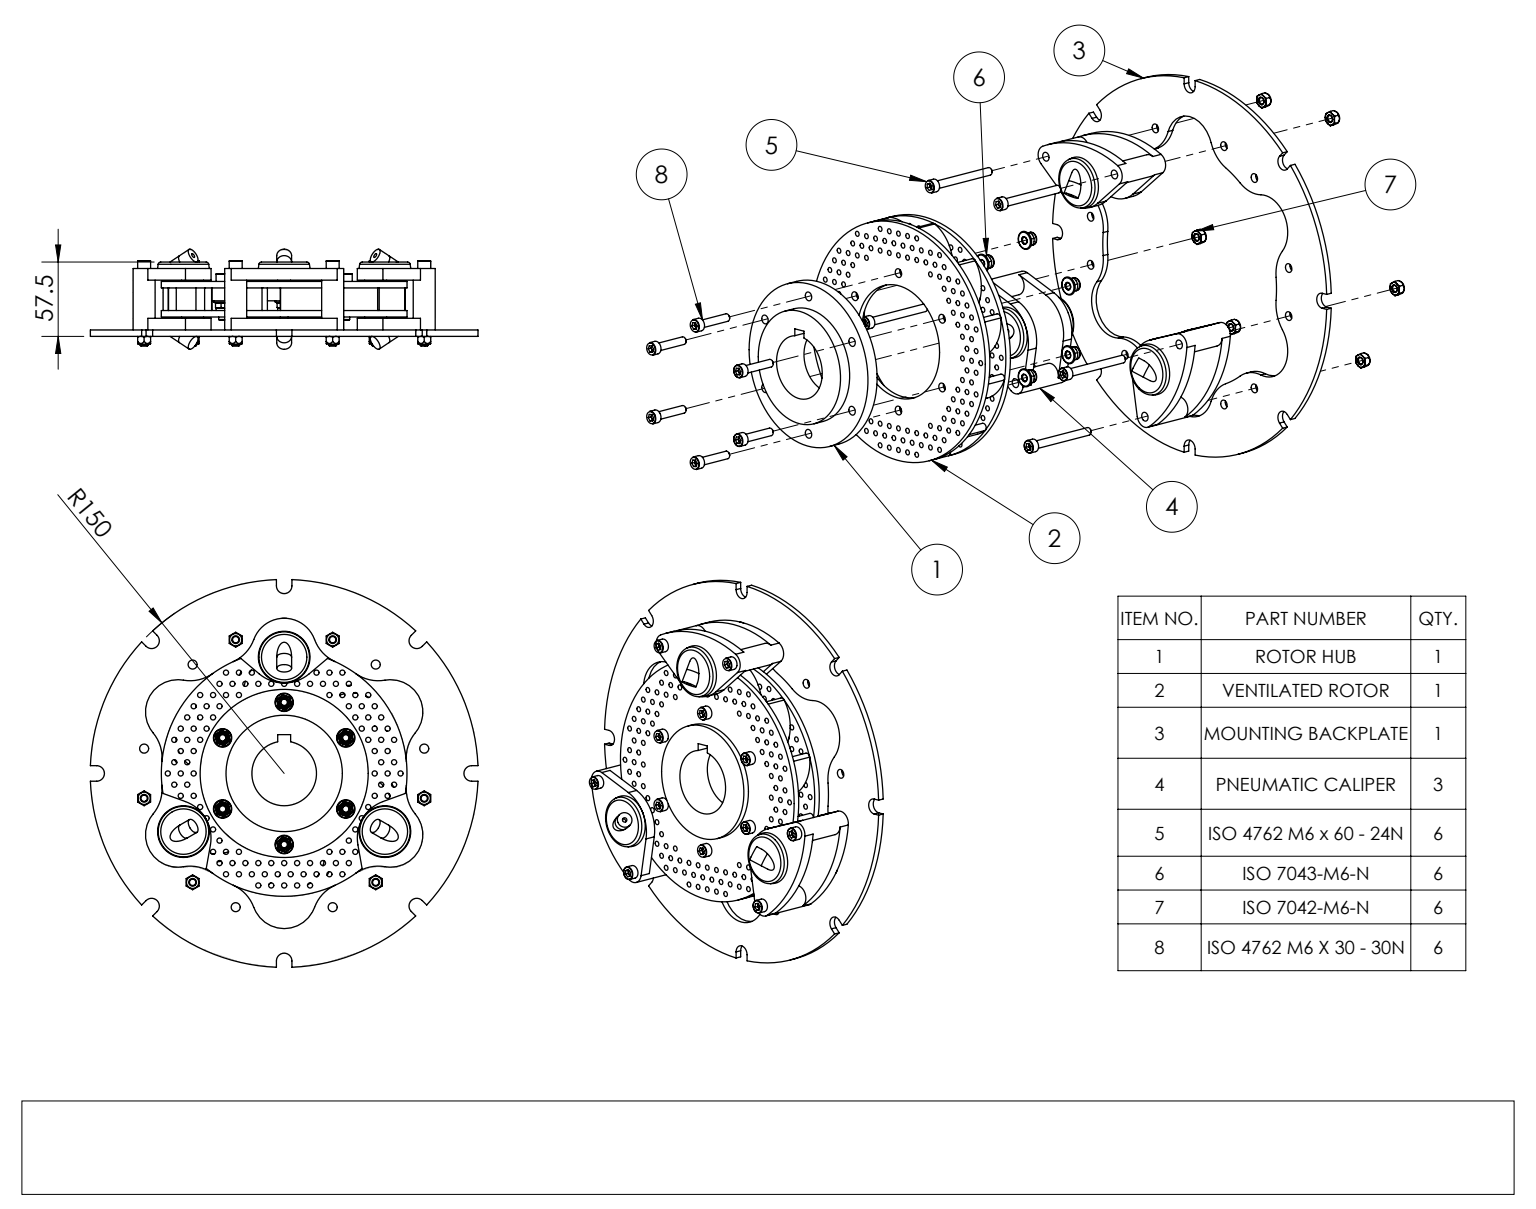
ISO-10303-21;
HEADER;
FILE_DESCRIPTION (('STEP AP214'),
    '1' );
FILE_NAME ('BR-596',
    '2026-09-21T15:58:29',
    ( '' ),
    ( '' ),
    'SwSTEP 2.0',
    'SolidWorks 2026',
    '' );
FILE_SCHEMA (( 'AUTOMOTIVE_DESIGN' ));
ENDSEC;

DATA;
#1 = ORIENTED_EDGE ( 'NONE', *, *, #25263, .F. ) ;
#2 = EDGE_CURVE ( 'NONE', #26836, #23671, #14788, .T. ) ;
#3 = ORIENTED_EDGE ( 'NONE', *, *, #6672, .T. ) ;
#4 = VERTEX_POINT ( 'NONE', #16752 ) ;
#5 = DIRECTION ( 'NONE',  ( 0.000000000000000000, 0.000000000000000000, 1.000000000000000000 ) ) ;
#6 = AXIS2_PLACEMENT_3D ( 'NONE', #11763, #3538, #9529 ) ;
#7 = CARTESIAN_POINT ( 'NONE',  ( 73.47608876694671665, 59.13646009116074964, -4.999999999999997335 ) ) ;
#8 = ADVANCED_FACE ( 'NONE', ( #25357 ), #3421, .T. ) ;
#9 = AXIS2_PLACEMENT_3D ( 'NONE', #11158, #31391, #28593 ) ;
#10 = DIRECTION ( 'NONE',  ( -1.000000000000000000, 0.000000000000000000, 0.000000000000000000 ) ) ;
#11 = DIRECTION ( 'NONE',  ( 0.000000000000000000, 0.000000000000000000, 1.000000000000000000 ) ) ;
#12 = FACE_OUTER_BOUND ( 'NONE', #34219, .T. ) ;
#13 = EDGE_CURVE ( 'NONE', #31164, #27343, #2215, .T. ) ;
#14 = ORIENTED_EDGE ( 'NONE', *, *, #31079, .F. ) ;
#15 = DIRECTION ( 'NONE',  ( 0.000000000000000000, 0.000000000000000000, 1.000000000000000000 ) ) ;
#16 = CARTESIAN_POINT ( 'NONE',  ( 4.999999999999997335, 0.000000000000000000, 0.000000000000000000 ) ) ;
#17 = DIRECTION ( 'NONE',  ( 1.000000000000000000, 0.000000000000000000, 0.000000000000000000 ) ) ;
#18 = EDGE_LOOP ( 'NONE', ( #28205, #32238, #16851 ) ) ;
#19 = AXIS2_PLACEMENT_3D ( 'NONE', #6620, #12200, #4183 ) ;
#20 = FACE_OUTER_BOUND ( 'NONE', #1538, .T. ) ;
#21 = CARTESIAN_POINT ( 'NONE',  ( -85.00000337463092137, -25.98076211353322051, -9.999999999999998224 ) ) ;
#22 = EDGE_CURVE ( 'NONE', #8678, #8115, #12991, .T. ) ;
#23 = ORIENTED_EDGE ( 'NONE', *, *, #7418, .F. ) ;
#24 = EDGE_CURVE ( 'NONE', #14526, #29968, #7006, .T. ) ;
#25 = ORIENTED_EDGE ( 'NONE', *, *, #3813, .F. ) ;
#26 = DIRECTION ( 'NONE',  ( 0.000000000000000000, 0.4999999999999951150, -0.8660254037844414832 ) ) ;
#27 = EDGE_CURVE ( 'NONE', #13680, #28909, #27960, .T. ) ;
#28 = CARTESIAN_POINT ( 'NONE',  ( 31.46585318596250502, 86.45172111230321832, 12.49999999999999822 ) ) ;
#29 = AXIS2_PLACEMENT_3D ( 'NONE', #25718, #14617, #11988 ) ;
#30 = DIRECTION ( 'NONE',  ( 0.000000000000000000, 0.000000000000000000, 1.000000000000000000 ) ) ;
#31 = EDGE_CURVE ( 'NONE', #24795, #10704, #408, .T. ) ;
#32 = DIRECTION ( 'NONE',  ( 0.000000000000000000, 0.000000000000000000, -1.000000000000000000 ) ) ;
#33 = VERTEX_POINT ( 'NONE', #15201 ) ;
#34 = ORIENTED_EDGE ( 'NONE', *, *, #16794, .F. ) ;
#35 = AXIS2_PLACEMENT_3D ( 'NONE', #3567, #23609, #24168 ) ;
#36 = DIRECTION ( 'NONE',  ( 0.000000000000000000, 0.000000000000000000, 1.000000000000000000 ) ) ;
#37 = CARTESIAN_POINT ( 'NONE',  ( -5.999999999999998224, -145.0000000000000568, 27.50000000000000000 ) ) ;
#38 = ORIENTED_EDGE ( 'NONE', *, *, #10995, .T. ) ;
#39 = DIRECTION ( 'NONE',  ( 0.000000000000000000, 0.000000000000000000, -1.000000000000000000 ) ) ;
#40 = VERTEX_POINT ( 'NONE', #29073 ) ;
#41 = B_SPLINE_CURVE_WITH_KNOTS ( 'NONE', 3,
 ( #1307, #24180, #18746, #30167, #7133, #7874, #14025, #11030, #2597, #10859, #22124, #25848, #25677, #17230, #22672, #5430, #8588, #5792, #22296, #5042, #34557, #25296, #13675, #2430, #10681, #28652, #33922, #25131, #25473, #19674, #2985, #16478, #17025, #14220, #34121 ),
 .UNSPECIFIED., .F., .F.,
 ( 4, 2, 1, 1, 2, 2, 1, 2, 2, 2, 2, 1, 2, 2, 1, 2, 2, 1, 1, 2, 4 ),
 ( 0.05563282717606015532, 0.06778080578355423491, 0.07992878439104830757, 0.1042247416060363280, 0.1163727202135303451, 0.1285206988210243761, 0.1528166560360122717, 0.1771126132510001672, 0.1892605918584941982, 0.2014085704659882570, 0.2500004848959641035, 0.2985923993259401166, 0.3107403779334341754, 0.3228883565409281786, 0.3471843137559161296, 0.3714802709709040252, 0.3836282495783980284, 0.3957762281858920317, 0.4200721854008799272, 0.4322201640083740415, 0.4443681426158681003 ),
 .UNSPECIFIED. ) ;
#42 = CARTESIAN_POINT ( 'NONE',  ( -51.68138994340220904, 113.8157894736842053, 27.50000000000000000 ) ) ;
#43 = LINE ( 'NONE', #5489, #22981 ) ;
#44 = EDGE_CURVE ( 'NONE', #12727, #16632, #5220, .T. ) ;
#45 = DIRECTION ( 'NONE',  ( 0.000000000000000000, 0.000000000000000000, 1.000000000000000000 ) ) ;
#46 = ORIENTED_EDGE ( 'NONE', *, *, #8957, .F. ) ;
#47 = ORIENTED_EDGE ( 'NONE', *, *, #25069, .T. ) ;
#48 = DIRECTION ( 'NONE',  ( 0.000000000000000000, 0.000000000000000000, 1.000000000000000000 ) ) ;
#49 = LINE ( 'NONE', #17110, #26195 ) ;
#50 = DIRECTION ( 'NONE',  ( 1.000000000000000000, 0.000000000000000000, 0.000000000000000000 ) ) ;
#51 = ORIENTED_EDGE ( 'NONE', *, *, #17262, .T. ) ;
#52 = CARTESIAN_POINT ( 'NONE',  ( 7.122621931239992550E-13, 68.00000000000000000, -49.86348611802629449 ) ) ;
#53 = AXIS2_PLACEMENT_3D ( 'NONE', #21369, #24177, #27163 ) ;
#54 = FACE_BOUND ( 'NONE', #30415, .T. ) ;
#55 = EDGE_CURVE ( 'NONE', #24891, #6532, #23685, .T. ) ;
#56 = DIRECTION ( 'NONE',  ( 1.000000000000000000, 0.000000000000000000, 0.000000000000000000 ) ) ;
#57 = CARTESIAN_POINT ( 'NONE',  ( 9.999996625368625658, 86.60254037844397601, 12.50000000000000000 ) ) ;
#58 = DIRECTION ( 'NONE',  ( 1.000000000000000000, 0.000000000000000000, 0.000000000000000000 ) ) ;
#59 = CYLINDRICAL_SURFACE ( 'NONE', #323, 2.000000000000001776 ) ;
#60 = CARTESIAN_POINT ( 'NONE',  ( 89.99999662536828282, 0.000000000000000000, 17.49999999999999645 ) ) ;
#61 = FACE_OUTER_BOUND ( 'NONE', #20749, .T. ) ;
#62 = ORIENTED_EDGE ( 'NONE', *, *, #28158, .F. ) ;
#63 = CARTESIAN_POINT ( 'NONE',  ( 34.00000000000068923, 58.88972745734143643, 12.49999999999999822 ) ) ;
#64 = DIRECTION ( 'NONE',  ( 0.000000000000000000, 0.000000000000000000, -1.000000000000000000 ) ) ;
#65 = LINE ( 'NONE', #14323, #21127 ) ;
#66 = EDGE_LOOP ( 'NONE', ( #17669, #12617 ) ) ;
#67 = EDGE_CURVE ( 'NONE', #35240, #2856, #17838, .T. ) ;
#68 = VERTEX_POINT ( 'NONE', #26089 ) ;
#69 = ORIENTED_EDGE ( 'NONE', *, *, #4639, .T. ) ;
#70 = EDGE_CURVE ( 'NONE', #12832, #7029, #18901, .T. ) ;
#71 = EDGE_CURVE ( 'NONE', #553, #16094, #23467, .T. ) ;
#72 = DIRECTION ( 'NONE',  ( 0.000000000000000000, 0.000000000000000000, 1.000000000000000000 ) ) ;
#73 = FACE_OUTER_BOUND ( 'NONE', #6428, .T. ) ;
#74 = CARTESIAN_POINT ( 'NONE',  ( -5.750000000000000000, 96.68456697298042002, 32.49999999999999289 ) ) ;
#75 = EDGE_LOOP ( 'NONE', ( #16524, #10873, #23457, #7165 ) ) ;
#76 = CIRCLE ( 'NONE', #28807, 2.000000000000001776 ) ;
#77 = DIRECTION ( 'NONE',  ( 1.000000000000000000, 0.000000000000000000, 0.000000000000000000 ) ) ;
#78 = ORIENTED_EDGE ( 'NONE', *, *, #9389, .F. ) ;
#79 = DIRECTION ( 'NONE',  ( -0.000000000000000000, -0.000000000000000000, -1.000000000000000000 ) ) ;
#80 = EDGE_LOOP ( 'NONE', ( #13593, #3847 ) ) ;
#81 = CYLINDRICAL_SURFACE ( 'NONE', #36890, 3.000000000000002665 ) ;
#82 = ORIENTED_EDGE ( 'NONE', *, *, #8215, .F. ) ;
#83 = ORIENTED_EDGE ( 'NONE', *, *, #27457, .T. ) ;
#84 = FACE_OUTER_BOUND ( 'NONE', #29361, .T. ) ;
#85 = DIRECTION ( 'NONE',  ( 1.000000000000000000, 0.000000000000000000, 0.000000000000000000 ) ) ;
#86 = DIRECTION ( 'NONE',  ( 0.000000000000000000, 0.000000000000000000, 1.000000000000000000 ) ) ;
#87 = ORIENTED_EDGE ( 'NONE', *, *, #14475, .T. ) ;
#88 = DIRECTION ( 'NONE',  ( 0.000000000000000000, 0.000000000000000000, 1.000000000000000000 ) ) ;
#89 = EDGE_CURVE ( 'NONE', #15444, #13344, #33274, .T. ) ;
#90 = DIRECTION ( 'NONE',  ( 0.000000000000000000, 0.000000000000000000, 1.000000000000000000 ) ) ;
#91 = CARTESIAN_POINT ( 'NONE',  ( 0.000000000000000000, 0.000000000000000000, -4.599999999999999645 ) ) ;
#92 = EDGE_LOOP ( 'NONE', ( #21704, #496, #2169, #36469 ) ) ;
#93 = CYLINDRICAL_SURFACE ( 'NONE', #7565, 2.000000000000001776 ) ;
#94 = DIRECTION ( 'NONE',  ( 0.000000000000000000, 0.000000000000000000, 1.000000000000000000 ) ) ;
#95 = CIRCLE ( 'NONE', #3102, 2.000000000000001776 ) ;
#96 = ORIENTED_EDGE ( 'NONE', *, *, #17102, .T. ) ;
#97 = DIRECTION ( 'NONE',  ( 1.000000000000000000, 0.000000000000000000, 0.000000000000000000 ) ) ;
#98 = CIRCLE ( 'NONE', #10881, 2.000000000000001776 ) ;
#99 = FACE_OUTER_BOUND ( 'NONE', #4741, .T. ) ;
#100 = CYLINDRICAL_SURFACE ( 'NONE', #2791, 2.000000000000001776 ) ;
#101 = CARTESIAN_POINT ( 'NONE',  ( 77.99999662536832545, -34.64101615137759183, -9.999999999999998224 ) ) ;
#102 = ORIENTED_EDGE ( 'NONE', *, *, #25257, .T. ) ;
#103 = DIRECTION ( 'NONE',  ( 1.000000000000000000, 0.000000000000000000, 0.000000000000000000 ) ) ;
#104 = FACE_OUTER_BOUND ( 'NONE', #24735, .T. ) ;
#105 = VERTEX_POINT ( 'NONE', #9030 ) ;
#106 = ORIENTED_EDGE ( 'NONE', *, *, #23165, .T. ) ;
#107 = EDGE_CURVE ( 'NONE', #34831, #10183, #17101, .T. ) ;
#108 = FACE_OUTER_BOUND ( 'NONE', #27387, .T. ) ;
#109 = CARTESIAN_POINT ( 'NONE',  ( 7.999996625368656744, -69.28203230275519786, 17.49999999999999645 ) ) ;
#110 = DIRECTION ( 'NONE',  ( -1.000000000000000000, -4.625929269271482956E-15, 0.000000000000000000 ) ) ;
#111 = VERTEX_POINT ( 'NONE', #9201 ) ;
#112 = CIRCLE ( 'NONE', #7327, 33.00000000000002132 ) ;
#113 = DIRECTION ( 'NONE',  ( 0.000000000000000000, 0.000000000000000000, 1.000000000000000000 ) ) ;
#114 = VERTEX_POINT ( 'NONE', #394 ) ;
#115 = CYLINDRICAL_SURFACE ( 'NONE', #8938, 2.000000000000001776 ) ;
#116 = ORIENTED_EDGE ( 'NONE', *, *, #4433, .F. ) ;
#117 = DIRECTION ( 'NONE',  ( 1.000000000000000000, 0.000000000000000000, 0.000000000000000000 ) ) ;
#118 = DIRECTION ( 'NONE',  ( -0.7071067811865463515, 0.7071067811865487940, 0.000000000000000000 ) ) ;
#119 = CARTESIAN_POINT ( 'NONE',  ( 0.000000000000000000, 0.000000000000000000, 12.49999999999999822 ) ) ;
#120 = ORIENTED_EDGE ( 'NONE', *, *, #22119, .T. ) ;
#121 = EDGE_CURVE ( 'NONE', #28672, #5777, #21894, .T. ) ;
#122 = DIRECTION ( 'NONE',  ( -0.4999999999999919509, 0.8660254037844432595, 0.000000000000000000 ) ) ;
#123 = CARTESIAN_POINT ( 'NONE',  ( -65.00000337463106348, -60.62177826491083010, -9.999999999999998224 ) ) ;
#124 = DIRECTION ( 'NONE',  ( -1.000000000000000000, 0.000000000000000000, 0.000000000000000000 ) ) ;
#125 = DIRECTION ( 'NONE',  ( -1.000000000000000000, 0.000000000000000000, 0.000000000000000000 ) ) ;
#126 = VERTEX_POINT ( 'NONE', #20628 ) ;
#127 = CARTESIAN_POINT ( 'NONE',  ( -56.67878100130369035, 27.78182860042797131, 12.49999999999999822 ) ) ;
#128 = DIRECTION ( 'NONE',  ( 0.000000000000000000, 0.000000000000000000, -1.000000000000000000 ) ) ;
#129 = DIRECTION ( 'NONE',  ( -1.000000000000000000, 0.000000000000000000, 0.000000000000000000 ) ) ;
#130 = ORIENTED_EDGE ( 'NONE', *, *, #1368, .T. ) ;
#131 = EDGE_CURVE ( 'NONE', #32452, #18237, #7927, .T. ) ;
#132 = EDGE_LOOP ( 'NONE', ( #17716, #15446, #15780, #32806 ) ) ;
#133 = CIRCLE ( 'NONE', #36688, 33.00000000000001421 ) ;
#134 = ORIENTED_EDGE ( 'NONE', *, *, #2252, .T. ) ;
#135 = DIRECTION ( 'NONE',  ( 1.000000000000000000, 0.000000000000000000, 0.000000000000000000 ) ) ;
#136 = CARTESIAN_POINT ( 'NONE',  ( -20.00000337463123756, -86.60254037844400443, -9.999999999999998224 ) ) ;
#137 = EDGE_CURVE ( 'NONE', #22617, #21874, #32058, .T. ) ;
#138 = CARTESIAN_POINT ( 'NONE',  ( 71.99999662536838230, -34.64101615137759183, -9.999999999999998224 ) ) ;
#139 = CARTESIAN_POINT ( 'NONE',  ( 98.28784258492957804, -106.7731239591692116, 32.50000000000000000 ) ) ;
#140 = DIRECTION ( 'NONE',  ( -1.000000000000000000, -9.765850679573131385E-15, 0.000000000000000000 ) ) ;
#141 = CARTESIAN_POINT ( 'NONE',  ( -5.000000000000000888, 3.082654106983011122, -4.288941049016753659 ) ) ;
#142 = ORIENTED_EDGE ( 'NONE', *, *, #26390, .F. ) ;
#143 = ORIENTED_EDGE ( 'NONE', *, *, #17525, .F. ) ;
#144 = CIRCLE ( 'NONE', #10915, 3.499999999999996003 ) ;
#145 = FACE_OUTER_BOUND ( 'NONE', #19323, .T. ) ;
#146 = FACE_OUTER_BOUND ( 'NONE', #12482, .T. ) ;
#147 = DIRECTION ( 'NONE',  ( 0.000000000000000000, 0.000000000000000000, 1.000000000000000000 ) ) ;
#148 = VERTEX_POINT ( 'NONE', #32628 ) ;
#149 = PRODUCT_DEFINITION_CONTEXT ( 'detailed design', #18530, 'design' ) ;
#150 = EDGE_CURVE ( 'NONE', #5895, #27049, #26455, .T. ) ;
#151 = FACE_BOUND ( 'NONE', #17768, .T. ) ;
#152 = ORIENTED_EDGE ( 'NONE', *, *, #34112, .F. ) ;
#153 = CIRCLE ( 'NONE', #7373, 2.000000000000001776 ) ;
#154 = ORIENTED_EDGE ( 'NONE', *, *, #13664, .T. ) ;
#155 = EDGE_CURVE ( 'NONE', #32663, #9761, #30082, .T. ) ;
#156 = AXIS2_PLACEMENT_3D ( 'NONE', #424, #5891, #17129 ) ;
#157 = CARTESIAN_POINT ( 'NONE',  ( 81.99999662536832545, -17.32050807568879591, -9.999999999999998224 ) ) ;
#158 = ORIENTED_EDGE ( 'NONE', *, *, #26934, .T. ) ;
#159 = ADVANCED_FACE ( 'NONE', ( #762 ), #32267, .F. ) ;
#160 = PRODUCT ( 'Pneumatic caliper', 'Pneumatic caliper', '', ( #18111 ) ) ;
#161 = CARTESIAN_POINT ( 'NONE',  ( 47.99999662536846756, 51.96152422706637708, -5.000000000000000000 ) ) ;
#162 = CARTESIAN_POINT ( 'NONE',  ( -2.448772250512182280E-15, 99.94802294027086020, -19.99999999999999645 ) ) ;
#163 = ORIENTED_EDGE ( 'NONE', *, *, #28659, .F. ) ;
#164 = ORIENTED_EDGE ( 'NONE', *, *, #35718, .T. ) ;
#165 = EDGE_CURVE ( 'NONE', #35067, #9776, #18024, .T. ) ;
#166 = AXIS2_PLACEMENT_3D ( 'NONE', #2144, #21659, #19396 ) ;
#167 = VERTEX_POINT ( 'NONE', #9594 ) ;
#168 = ORIENTED_EDGE ( 'NONE', *, *, #20538, .F. ) ;
#169 = AXIS2_PLACEMENT_3D ( 'NONE', #10141, #18184, #29613 ) ;
#170 = EDGE_CURVE ( 'NONE', #35280, #21315, #27084, .T. ) ;
#171 = ORIENTED_EDGE ( 'NONE', *, *, #5884, .T. ) ;
#172 = DIRECTION ( 'NONE',  ( 0.000000000000000000, 0.000000000000000000, 1.000000000000000000 ) ) ;
#173 = FILL_AREA_STYLE_COLOUR ( '', #11405 ) ;
#174 = DIRECTION ( 'NONE',  ( 0.000000000000000000, 0.000000000000000000, 1.000000000000000000 ) ) ;
#175 = CARTESIAN_POINT ( 'NONE',  ( -37.50000000000000000, 103.4105893997321886, -19.99999999999999645 ) ) ;
#176 = DIRECTION ( 'NONE',  ( 0.000000000000000000, 0.000000000000000000, 1.000000000000000000 ) ) ;
#177 = ORIENTED_EDGE ( 'NONE', *, *, #12686, .T. ) ;
#178 = CARTESIAN_POINT ( 'NONE',  ( 0.000000000000000000, 0.000000000000000000, -15.00000000000000000 ) ) ;
#179 = CARTESIAN_POINT ( 'NONE',  ( 76.99999662536836809, -8.660254037844401509, -5.000000000000000000 ) ) ;
#180 = AXIS2_PLACEMENT_3D ( 'NONE', #17663, #11656, #14493 ) ;
#181 = CARTESIAN_POINT ( 'NONE',  ( -87.00000337463093558, 25.98076211353317433, -9.999999999999998224 ) ) ;
#182 = VERTEX_POINT ( 'NONE', #6760 ) ;
#183 = LINE ( 'NONE', #25523, #9480 ) ;
#184 = CARTESIAN_POINT ( 'NONE',  ( -67.00000337463102085, 43.30127018922198801, -9.999999999999998224 ) ) ;
#185 = ORIENTED_EDGE ( 'NONE', *, *, #1729, .T. ) ;
#186 = EDGE_LOOP ( 'NONE', ( #37032, #34199, #35351 ) ) ;
#187 = ADVANCED_FACE ( 'NONE', ( #3211 ), #1327, .T. ) ;
#188 = DIRECTION ( 'NONE',  ( 0.7071067811865512365, 0.7071067811865439090, -0.000000000000000000 ) ) ;
#189 = DIRECTION ( 'NONE',  ( -1.000000000000000000, 0.000000000000000000, 0.000000000000000000 ) ) ;
#190 = DIRECTION ( 'NONE',  ( 0.000000000000000000, 0.000000000000000000, 1.000000000000000000 ) ) ;
#191 = FACE_OUTER_BOUND ( 'NONE', #12059, .T. ) ;
#192 = ORIENTED_EDGE ( 'NONE', *, *, #24443, .F. ) ;
#193 = ORIENTED_EDGE ( 'NONE', *, *, #28677, .F. ) ;
#194 = CIRCLE ( 'NONE', #12140, 30.00000000000000000 ) ;
#195 = FACE_OUTER_BOUND ( 'NONE', #26488, .T. ) ;
#196 = EDGE_CURVE ( 'NONE', #666, #24271, #33682, .T. ) ;
#197 = CARTESIAN_POINT ( 'NONE',  ( 0.000000000000000000, 0.000000000000000000, 13.31572692736085095 ) ) ;
#198 = CYLINDRICAL_SURFACE ( 'NONE', #3922, 2.000000000000001776 ) ;
#199 = CIRCLE ( 'NONE', #27130, 2.000000000000001776 ) ;
#200 = VERTEX_POINT ( 'NONE', #18959 ) ;
#201 = ADVANCED_FACE ( 'NONE', ( #30385 ), #30581, .F. ) ;
#202 = DIRECTION ( 'NONE',  ( 0.000000000000000000, 0.000000000000000000, -1.000000000000000000 ) ) ;
#203 = VERTEX_POINT ( 'NONE', #33394 ) ;
#204 = ORIENTED_EDGE ( 'NONE', *, *, #23510, .F. ) ;
#205 = CIRCLE ( 'NONE', #19978, 1.999999999999998224 ) ;
#206 = CARTESIAN_POINT ( 'NONE',  ( -55.00000337463107059, 43.30127018922197379, -9.999999999999998224 ) ) ;
#207 = AXIS2_PLACEMENT_3D ( 'NONE', #7351, #10726, #24618 ) ;
#208 = LINE ( 'NONE', #6596, #28035 ) ;
#209 = EDGE_LOOP ( 'NONE', ( #36772, #14646 ) ) ;
#210 = VERTEX_POINT ( 'NONE', #1504 ) ;
#211 = FACE_OUTER_BOUND ( 'NONE', #12219, .T. ) ;
#212 = CIRCLE ( 'NONE', #9335, 3.500000000000003109 ) ;
#213 = DIRECTION ( 'NONE',  ( 0.000000000000000000, 0.000000000000000000, 1.000000000000000000 ) ) ;
#214 = DIRECTION ( 'NONE',  ( -1.000000000000000000, 0.000000000000000000, 0.000000000000000000 ) ) ;
#215 = EDGE_CURVE ( 'NONE', #20361, #36249, #4334, .T. ) ;
#216 = ORIENTED_EDGE ( 'NONE', *, *, #28158, .T. ) ;
#217 = CARTESIAN_POINT ( 'NONE',  ( 54.99999662536846046, -43.30127018922200222, -9.999999999999998224 ) ) ;
#218 = FACE_BOUND ( 'NONE', #809, .T. ) ;
#219 = LINE ( 'NONE', #29087, #28624 ) ;
#220 = DIRECTION ( 'NONE',  ( 1.000000000000000000, 0.000000000000000000, 0.000000000000000000 ) ) ;
#221 = CARTESIAN_POINT ( 'NONE',  ( -13.00000337463126066, 77.94228634059957983, 17.49999999999999645 ) ) ;
#222 = DIRECTION ( 'NONE',  ( 1.000000000000000000, 0.000000000000000000, 0.000000000000000000 ) ) ;
#223 = CIRCLE ( 'NONE', #20559, 2.000000000000000000 ) ;
#224 = DIRECTION ( 'NONE',  ( 0.000000000000000000, 0.000000000000000000, 1.000000000000000000 ) ) ;
#225 = DIRECTION ( 'NONE',  ( 0.000000000000000000, 0.000000000000000000, -1.000000000000000000 ) ) ;
#226 = ORIENTED_EDGE ( 'NONE', *, *, #20326, .F. ) ;
#227 = CARTESIAN_POINT ( 'NONE',  ( -60.00000337463108480, -51.96152422706641971, -9.999999999999998224 ) ) ;
#228 = DIRECTION ( 'NONE',  ( 0.000000000000000000, 0.000000000000000000, -1.000000000000000000 ) ) ;
#229 = CARTESIAN_POINT ( 'NONE',  ( 0.000000000000000000, -55.00000000000000000, 5.000000000000000888 ) ) ;
#230 = VECTOR ( 'NONE', #24200, 1000.000000000000000 ) ;
#231 = ORIENTED_EDGE ( 'NONE', *, *, #33765, .T. ) ;
#232 = EDGE_LOOP ( 'NONE', ( #6616, #28930, #1676, #8816 ) ) ;
#233 = EDGE_CURVE ( 'NONE', #35279, #34770, #16155, .T. ) ;
#234 = ORIENTED_EDGE ( 'NONE', *, *, #11721, .F. ) ;
#235 = CIRCLE ( 'NONE', #13432, 1.999999999999998224 ) ;
#236 = DIRECTION ( 'NONE',  ( -1.000000000000000000, 0.000000000000000000, 0.000000000000000000 ) ) ;
#237 = CYLINDRICAL_SURFACE ( 'NONE', #14553, 2.000000000000001776 ) ;
#238 = EDGE_CURVE ( 'NONE', #20810, #35505, #23500, .T. ) ;
#239 = CARTESIAN_POINT ( 'NONE',  ( 79.99999662536833966, 34.64101615137759183, -5.000000000000000000 ) ) ;
#240 = EDGE_LOOP ( 'NONE', ( #25593, #21234, #28289, #3164 ) ) ;
#241 = EDGE_CURVE ( 'NONE', #35128, #3947, #28283, .T. ) ;
#242 = DIRECTION ( 'NONE',  ( 0.8660254037844418162, 0.4999999999999946709, 0.000000000000000000 ) ) ;
#243 = ORIENTED_EDGE ( 'NONE', *, *, #24473, .T. ) ;
#244 = CARTESIAN_POINT ( 'NONE',  ( -70.00000337463099243, 51.96152422706637708, -5.000000000000000000 ) ) ;
#246 = EDGE_CURVE ( 'NONE', #24313, #6247, #31847, .T. ) ;
#245 = VERTEX_POINT ( 'NONE', #21754 ) ;
#247 = CARTESIAN_POINT ( 'NONE',  ( -47.63139720814438505, -27.49999999999955591, -5.000000000000000888 ) ) ;
#248 = ORIENTED_EDGE ( 'NONE', *, *, #1490, .F. ) ;
#249 = EDGE_CURVE ( 'NONE', #20086, #13680, #36679, .T. ) ;
#250 = ORIENTED_EDGE ( 'NONE', *, *, #33993, .T. ) ;
#251 = CIRCLE ( 'NONE', #9840, 27.00000000000001421 ) ;
#252 = FACE_OUTER_BOUND ( 'NONE', #33217, .T. ) ;
#253 = CARTESIAN_POINT ( 'NONE',  ( -31.00000000000027356, -58.88972745734168512, -4.999999999999997335 ) ) ;
#254 = CARTESIAN_POINT ( 'NONE',  ( -3.374631303565411855E-06, -86.60254037844400443, -9.999999999999998224 ) ) ;
#255 = ORIENTED_EDGE ( 'NONE', *, *, #21076, .T. ) ;
#256 = DIRECTION ( 'NONE',  ( 1.000000000000000000, 0.000000000000000000, 0.000000000000000000 ) ) ;
#257 = EDGE_CURVE ( 'NONE', #28630, #6061, #8948, .T. ) ;
#258 = AXIS2_PLACEMENT_3D ( 'NONE', #28130, #2453, #13872 ) ;
#259 = CARTESIAN_POINT ( 'NONE',  ( 0.000000000000000000, 0.000000000000000000, 12.49999999999999822 ) ) ;
#260 = AXIS2_PLACEMENT_3D ( 'NONE', #12321, #32216, #32783 ) ;
#261 = EDGE_CURVE ( 'NONE', #2865, #30153, #36198, .T. ) ;
#262 = DIRECTION ( 'NONE',  ( -1.000000000000000000, 0.000000000000000000, 0.000000000000000000 ) ) ;
#263 = ADVANCED_FACE ( 'NONE', ( #24402 ), #10505, .F. ) ;
#264 = EDGE_LOOP ( 'NONE', ( #8446, #2459 ) ) ;
#265 = VECTOR ( 'NONE', #23619, 1000.000000000000000 ) ;
#266 = CARTESIAN_POINT ( 'NONE',  ( 51.99999662536848888, -51.96152422706640550, 12.50000000000000000 ) ) ;
#267 = CARTESIAN_POINT ( 'NONE',  ( 0.000000000000000000, 0.000000000000000000, -6.000000000000000000 ) ) ;
#268 = EDGE_CURVE ( 'NONE', #8353, #34330, #5962, .T. ) ;
#269 = ORIENTED_EDGE ( 'NONE', *, *, #4961, .F. ) ;
#270 = CARTESIAN_POINT ( 'NONE',  ( -40.00000337463113453, 69.28203230275516944, -9.999999999999998224 ) ) ;
#271 = CARTESIAN_POINT ( 'NONE',  ( 68.00000000000000000, 0.000000000000000000, -49.86348611802629449 ) ) ;
#272 = FACE_OUTER_BOUND ( 'NONE', #19222, .T. ) ;
#273 = DIRECTION ( 'NONE',  ( 1.000000000000000000, 0.000000000000000000, 0.000000000000000000 ) ) ;
#274 = DIRECTION ( 'NONE',  ( 1.000000000000000000, 0.000000000000000000, 0.000000000000000000 ) ) ;
#275 = AXIS2_PLACEMENT_3D ( 'NONE', #18372, #12551, #4489 ) ;
#276 = ORIENTED_EDGE ( 'NONE', *, *, #16312, .T. ) ;
#277 = AXIS2_PLACEMENT_3D ( 'NONE', #26246, #15000, #11980 ) ;
#278 = CARTESIAN_POINT ( 'NONE',  ( 3.057313426867659167, 4.281874658697558900, -4.057628883416042775 ) ) ;
#279 = DIRECTION ( 'NONE',  ( 0.000000000000000000, 0.000000000000000000, 1.000000000000000000 ) ) ;
#280 = B_SPLINE_CURVE_WITH_KNOTS ( 'NONE', 3,
 ( #34801, #31774, #15096, #20918, #14722, #278, #26525, #21088, #35175, #6104 ),
 .UNSPECIFIED., .F., .F.,
 ( 4, 2, 2, 2, 4 ),
 ( 8.020416891258658357E-20, 0.001528561485809837349, 0.003057122971619673831, 0.004585684457429509663, 0.006114245943239347662 ),
 .UNSPECIFIED. ) ;
#281 = VERTEX_POINT ( 'NONE', #22145 ) ;
#282 = CIRCLE ( 'NONE', #23627, 2.000000000000001776 ) ;
#283 = ORIENTED_EDGE ( 'NONE', *, *, #11463, .F. ) ;
#284 = ORIENTED_EDGE ( 'NONE', *, *, #26597, .T. ) ;
#285 =( LENGTH_UNIT ( ) NAMED_UNIT ( * ) SI_UNIT ( .MILLI., .METRE. ) );
#286 = DIRECTION ( 'NONE',  ( 0.000000000000000000, 0.000000000000000000, 1.000000000000000000 ) ) ;
#287 = DIRECTION ( 'NONE',  ( -1.000000000000000000, 0.000000000000000000, 0.000000000000000000 ) ) ;
#288 = AXIS2_PLACEMENT_3D ( 'NONE', #11552, #26000, #31627 ) ;
#289 = CIRCLE ( 'NONE', #2710, 2.000000000000001776 ) ;
#290 = DIRECTION ( 'NONE',  ( 0.000000000000000000, 0.000000000000000000, -1.000000000000000000 ) ) ;
#291 = ORIENTED_EDGE ( 'NONE', *, *, #20174, .T. ) ;
#292 = FACE_OUTER_BOUND ( 'NONE', #26627, .T. ) ;
#293 = ORIENTED_EDGE ( 'NONE', *, *, #27242, .F. ) ;
#294 = FACE_BOUND ( 'NONE', #33628, .T. ) ;
#295 = DIRECTION ( 'NONE',  ( 1.000000000000000000, 0.000000000000000000, 0.000000000000000000 ) ) ;
#296 = CIRCLE ( 'NONE', #6888, 2.000000000000001776 ) ;
#297 = CARTESIAN_POINT ( 'NONE',  ( -60.00000337463104216, 34.64101615137757051, -9.999999999999998224 ) ) ;
#298 = CIRCLE ( 'NONE', #6279, 95.00000000000001421 ) ;
#299 = DIRECTION ( 'NONE',  ( 0.000000000000000000, 0.000000000000000000, 1.000000000000000000 ) ) ;
#300 = DIRECTION ( 'NONE',  ( 0.000000000000000000, 0.000000000000000000, 1.000000000000000000 ) ) ;
#301 = VECTOR ( 'NONE', #9104, 1000.000000000000000 ) ;
#302 = AXIS2_PLACEMENT_3D ( 'NONE', #13859, #25139, #31280 ) ;
#303 = DIRECTION ( 'NONE',  ( 0.000000000000000000, 0.000000000000000000, 1.000000000000000000 ) ) ;
#304 = CARTESIAN_POINT ( 'NONE',  ( 64.99999662536839651, -43.30127018922199511, -9.999999999999998224 ) ) ;
#305 = DIRECTION ( 'NONE',  ( 0.000000000000000000, 0.000000000000000000, 1.000000000000000000 ) ) ;
#306 = EDGE_CURVE ( 'NONE', #32244, #30221, #25138, .T. ) ;
#307 = ORIENTED_EDGE ( 'NONE', *, *, #13420, .T. ) ;
#308 = CARTESIAN_POINT ( 'NONE',  ( -40.00000337463113453, -69.28203230275519786, 17.49999999999999645 ) ) ;
#309 = CYLINDRICAL_SURFACE ( 'NONE', #34030, 2.000000000000001776 ) ;
#310 = VECTOR ( 'NONE', #20718, 1000.000000000000000 ) ;
#311 = CARTESIAN_POINT ( 'NONE',  ( -48.49679504533954599, -67.96280346788670101, 12.50000000000000000 ) ) ;
#312 = AXIS2_PLACEMENT_3D ( 'NONE', #1612, #13051, #12846 ) ;
#313 = CIRCLE ( 'NONE', #17111, 33.00000000000001421 ) ;
#314 = EDGE_LOOP ( 'NONE', ( #13805, #27625, #5618, #19237 ) ) ;
#315 = ORIENTED_EDGE ( 'NONE', *, *, #9812, .T. ) ;
#316 = APPLICATION_CONTEXT ( 'automotive_design' ) ;
#317 = ORIENTED_EDGE ( 'NONE', *, *, #23310, .F. ) ;
#318 = CYLINDRICAL_SURFACE ( 'NONE', #26736, 2.000000000000001776 ) ;
#319 = CARTESIAN_POINT ( 'NONE',  ( -4.749999999999999112, 0.000000000000000000, 0.000000000000000000 ) ) ;
#320 = VECTOR ( 'NONE', #25378, 1000.000000000000000 ) ;
#321 = LINE ( 'NONE', #703, #22374 ) ;
#322 = CARTESIAN_POINT ( 'NONE',  ( 0.000000000000000000, 0.000000000000000000, -6.000000000000000000 ) ) ;
#323 = AXIS2_PLACEMENT_3D ( 'NONE', #34020, #22562, #31540 ) ;
#324 = CARTESIAN_POINT ( 'NONE',  ( 34.99999662536855283, -77.94228634059960825, -9.999999999999998224 ) ) ;
#325 = VECTOR ( 'NONE', #1638, 1000.000000000000000 ) ;
#326 = EDGE_CURVE ( 'NONE', #14473, #5023, #12520, .T. ) ;
#327 = AXIS2_PLACEMENT_3D ( 'NONE', #16910, #9026, #2860 ) ;
#328 = DIRECTION ( 'NONE',  ( 1.000000000000000000, 0.000000000000000000, 0.000000000000000000 ) ) ;
#329 = EDGE_CURVE ( 'NONE', #27070, #4355, #10750, .T. ) ;
#330 = ORIENTED_EDGE ( 'NONE', *, *, #17401, .T. ) ;
#331 = ORIENTED_EDGE ( 'NONE', *, *, #15606, .T. ) ;
#332 = DIRECTION ( 'NONE',  ( 1.000000000000000000, 0.000000000000000000, 0.000000000000000000 ) ) ;
#333 = DIRECTION ( 'NONE',  ( 0.000000000000000000, 0.000000000000000000, 1.000000000000000000 ) ) ;
#334 = LINE ( 'NONE', #8600, #4130 ) ;
#335 = ORIENTED_EDGE ( 'NONE', *, *, #20881, .T. ) ;
#336 = AXIS2_PLACEMENT_3D ( 'NONE', #30480, #30096, #21491 ) ;
#337 = EDGE_CURVE ( 'NONE', #3085, #32118, #36511, .T. ) ;
#338 = FACE_BOUND ( 'NONE', #19821, .T. ) ;
#339 = EDGE_LOOP ( 'NONE', ( #32117, #28572, #22647 ) ) ;
#340 = ORIENTED_EDGE ( 'NONE', *, *, #13858, .F. ) ;
#341 = CARTESIAN_POINT ( 'NONE',  ( 31.99999662536857770, -69.28203230275519786, 17.49999999999999645 ) ) ;
#342 = ORIENTED_EDGE ( 'NONE', *, *, #22958, .F. ) ;
#343 = FILL_AREA_STYLE_COLOUR ( '', #32786 ) ;
#344 = DIRECTION ( 'NONE',  ( 1.000000000000000000, 0.000000000000000000, 0.000000000000000000 ) ) ;
#345 = AXIS2_PLACEMENT_3D ( 'NONE', #12956, #10173, #16343 ) ;
#346 = CARTESIAN_POINT ( 'NONE',  ( 35.99999999999999289, 0.000000000000000000, 0.000000000000000000 ) ) ;
#347 = EDGE_CURVE ( 'NONE', #5750, #19941, #18596, .T. ) ;
#348 = ORIENTED_EDGE ( 'NONE', *, *, #23113, .F. ) ;
#349 = ORIENTED_EDGE ( 'NONE', *, *, #15856, .F. ) ;
#350 = PRESENTATION_LAYER_ASSIGNMENT (  '', '', ( #29690 ) ) ;
#351 = CIRCLE ( 'NONE', #30901, 27.00000000000001421 ) ;
#352 = ORIENTED_EDGE ( 'NONE', *, *, #4867, .T. ) ;
#353 = VECTOR ( 'NONE', #6522, 1000.000000000000000 ) ;
#354 = AXIS2_PLACEMENT_3D ( 'NONE', #1393, #4597, #16033 ) ;
#355 = EDGE_LOOP ( 'NONE', ( #5631, #10944 ) ) ;
#356 = CIRCLE ( 'NONE', #29106, 2.000000000000001776 ) ;
#357 = VERTEX_POINT ( 'NONE', #11426 ) ;
#358 = CARTESIAN_POINT ( 'NONE',  ( 64.99999662536839651, -60.62177826491080168, 12.50000000000000000 ) ) ;
#359 = DIRECTION ( 'NONE',  ( 0.000000000000000000, 0.000000000000000000, 1.000000000000000000 ) ) ;
#360 = CARTESIAN_POINT ( 'NONE',  ( 61.99999662536842493, 51.96152422706639129, -9.999999999999998224 ) ) ;
#361 = CARTESIAN_POINT ( 'NONE',  ( 67.30619744049005249, 84.18124734178236679, 32.50000000000000000 ) ) ;
#362 = DIRECTION ( 'NONE',  ( 0.000000000000000000, 0.000000000000000000, 1.000000000000000000 ) ) ;
#363 = ORIENTED_EDGE ( 'NONE', *, *, #17772, .T. ) ;
#364 = DIRECTION ( 'NONE',  ( 4.625929269271481378E-15, 1.000000000000000000, 0.000000000000000000 ) ) ;
#365 = VECTOR ( 'NONE', #5528, 1000.000000000000000 ) ;
#366 = CARTESIAN_POINT ( 'NONE',  ( -3.374631289687624047E-06, -69.28203230275519786, 17.49999999999999645 ) ) ;
#367 = EDGE_CURVE ( 'NONE', #31278, #23804, #18545, .T. ) ;
#368 = DIRECTION ( 'NONE',  ( 0.000000000000000000, 0.000000000000000000, 1.000000000000000000 ) ) ;
#369 = ORIENTED_EDGE ( 'NONE', *, *, #22241, .T. ) ;
#370 = DIRECTION ( 'NONE',  ( 1.000000000000000000, 0.000000000000000000, 0.000000000000000000 ) ) ;
#371 = CARTESIAN_POINT ( 'NONE',  ( -50.00000337463112032, -51.96152422706641971, -9.999999999999998224 ) ) ;
#372 = ORIENTED_EDGE ( 'NONE', *, *, #6789, .F. ) ;
#373 = AXIS2_PLACEMENT_3D ( 'NONE', #34364, #17849, #12387 ) ;
#374 = VERTEX_POINT ( 'NONE', #8609 ) ;
#375 = CARTESIAN_POINT ( 'NONE',  ( -145.0000000000000000, 6.000000000001517009, 32.50000000000000000 ) ) ;
#376 = CIRCLE ( 'NONE', #15948, 2.000000000000001776 ) ;
#377 = PRODUCT_DEFINITION ( 'UNKNOWN', '', #6977, #25310 ) ;
#378 = DIRECTION ( 'NONE',  ( -1.000000000000000000, 0.000000000000000000, 0.000000000000000000 ) ) ;
#379 = DIRECTION ( 'NONE',  ( 1.000000000000000000, 0.000000000000000000, 0.000000000000000000 ) ) ;
#380 = DIRECTION ( 'NONE',  ( 0.000000000000000000, 0.000000000000000000, -1.000000000000000000 ) ) ;
#381 = EDGE_CURVE ( 'NONE', #31393, #2483, #23330, .T. ) ;
#382 = AXIS2_PLACEMENT_3D ( 'NONE', #31082, #5410, #34450 ) ;
#383 = ORIENTED_EDGE ( 'NONE', *, *, #2638, .F. ) ;
#384 = AXIS2_PLACEMENT_3D ( 'NONE', #15641, #24247, #35700 ) ;
#385 = AXIS2_PLACEMENT_3D ( 'NONE', #13978, #33868, #34423 ) ;
#386 = CARTESIAN_POINT ( 'NONE',  ( 44.99999662536851019, 77.94228634059959404, -9.999999999999998224 ) ) ;
#387 = CARTESIAN_POINT ( 'NONE',  ( 46.99999662536849598, 60.62177826491077326, -9.999999999999998224 ) ) ;
#388 = CARTESIAN_POINT ( 'NONE',  ( 3.000000000000000000, 0.000000000000000000, 0.000000000000000000 ) ) ;
#389 = AXIS2_PLACEMENT_3D ( 'NONE', #3869, #35759, #30111 ) ;
#390 = ADVANCED_FACE ( 'NONE', ( #34309 ), #8442, .F. ) ;
#391 = ORIENTED_EDGE ( 'NONE', *, *, #32304, .T. ) ;
#392 = CARTESIAN_POINT ( 'NONE',  ( 3.000000000000000000, 1.467624384280029615, 2.541999999999997151 ) ) ;
#393 = VERTEX_POINT ( 'NONE', #19504 ) ;
#394 = CARTESIAN_POINT ( 'NONE',  ( 96.53048327204960799, 102.5304832720492527, 32.50000000000000000 ) ) ;
#395 = CIRCLE ( 'NONE', #5209, 2.000000000000001776 ) ;
#396 = DIRECTION ( 'NONE',  ( 0.000000000000000000, 0.000000000000000000, 1.000000000000000000 ) ) ;
#397 = CARTESIAN_POINT ( 'NONE',  ( -8.000003374631278419, -69.28203230275519786, -9.999999999999998224 ) ) ;
#398 = ORIENTED_EDGE ( 'NONE', *, *, #9596, .T. ) ;
#399 = ORIENTED_EDGE ( 'NONE', *, *, #27886, .T. ) ;
#400 = CARTESIAN_POINT ( 'NONE',  ( 0.000000000000000000, 0.000000000000000000, -0.3851141460153411078 ) ) ;
#401 = VECTOR ( 'NONE', #13709, 1000.000000000000000 ) ;
#402 = CARTESIAN_POINT ( 'NONE',  ( 54.99999662536846046, -43.30127018922200222, -5.000000000000000000 ) ) ;
#403 = FACE_OUTER_BOUND ( 'NONE', #1715, .T. ) ;
#404 = EDGE_CURVE ( 'NONE', #30547, #29314, #28481, .T. ) ;
#405 = CIRCLE ( 'NONE', #23176, 2.000000000000001776 ) ;
#406 = VERTEX_POINT ( 'NONE', #31295 ) ;
#407 = CARTESIAN_POINT ( 'NONE',  ( -75.00000337463097821, -8.660254037844422825, -5.000000000000000000 ) ) ;
#408 = CIRCLE ( 'NONE', #21379, 95.00000000000000000 ) ;
#409 = FACE_BOUND ( 'NONE', #25954, .T. ) ;
#410 = DIRECTION ( 'NONE',  ( 0.000000000000000000, 0.000000000000000000, 1.000000000000000000 ) ) ;
#411 = CARTESIAN_POINT ( 'NONE',  ( 84.99999662536832545, 25.98076211353319565, -5.000000000000000000 ) ) ;
#412 = CARTESIAN_POINT ( 'NONE',  ( -55.27226924886181791, -77.26562141134519379, 27.50000000000000000 ) ) ;
#413 = STYLED_ITEM ( 'NONE', ( #19324 ), #17045 ) ;
#414 = CYLINDRICAL_SURFACE ( 'NONE', #5727, 2.000000000000001776 ) ;
#415 = EDGE_CURVE ( 'NONE', #9776, #6234, #17336, .T. ) ;
#416 = AXIS2_PLACEMENT_3D ( 'NONE', #33124, #10826, #22083 ) ;
#417 = CIRCLE ( 'NONE', #24987, 2.000000000000001776 ) ;
#418 = CARTESIAN_POINT ( 'NONE',  ( -72.00000337463100664, 34.64101615137758472, -9.999999999999998224 ) ) ;
#419 = EDGE_CURVE ( 'NONE', #33801, #10648, #30929, .T. ) ;
#420 = FACE_OUTER_BOUND ( 'NONE', #10081, .T. ) ;
#421 = ORIENTED_EDGE ( 'NONE', *, *, #12604, .F. ) ;
#422 = DIRECTION ( 'NONE',  ( -1.000000000000000000, 0.000000000000000000, 0.000000000000000000 ) ) ;
#423 = DIRECTION ( 'NONE',  ( 0.8191520442889913545, 1.003171929053524254E-16, -0.5735764363510468256 ) ) ;
#424 = CARTESIAN_POINT ( 'NONE',  ( 0.000000000000000000, 0.000000000000000000, 32.50000000000000000 ) ) ;
#425 = AXIS2_PLACEMENT_3D ( 'NONE', #16423, #2545, #16814 ) ;
#426 = ORIENTED_EDGE ( 'NONE', *, *, #31754, .T. ) ;
#427 = AXIS2_PLACEMENT_3D ( 'NONE', #36028, #27183, #30185 ) ;
#428 = ORIENTED_EDGE ( 'NONE', *, *, #23008, .T. ) ;
#429 = EDGE_LOOP ( 'NONE', ( #21064, #7984 ) ) ;
#430 = CARTESIAN_POINT ( 'NONE',  ( 3.000000000000000000, 0.000000000000000000, -25.03750572909317285 ) ) ;
#431 = DIRECTION ( 'NONE',  ( 1.000000000000000000, 0.000000000000000000, 0.000000000000000000 ) ) ;
#432 = CARTESIAN_POINT ( 'NONE',  ( -30.00000337463118427, 69.28203230275516944, -9.999999999999998224 ) ) ;
#433 = ORIENTED_EDGE ( 'NONE', *, *, #32932, .F. ) ;
#434 = CIRCLE ( 'NONE', #22609, 3.500000000000003109 ) ;
#435 = CIRCLE ( 'NONE', #1059, 2.000000000000001776 ) ;
#436 = CARTESIAN_POINT ( 'NONE',  ( 51.68138994340220904, -113.8157894736842053, 32.50002500000000083 ) ) ;
#437 = EDGE_CURVE ( 'NONE', #14230, #21660, #8801, .T. ) ;
#438 = AXIS2_PLACEMENT_3D ( 'NONE', #22022, #2338, #36089 ) ;
#439 = ORIENTED_EDGE ( 'NONE', *, *, #25001, .T. ) ;
#440 = CARTESIAN_POINT ( 'NONE',  ( -18.19096825468298206, -112.1612438786420256, 32.50000000000000000 ) ) ;
#441 = ORIENTED_EDGE ( 'NONE', *, *, #21012, .F. ) ;
#442 = LINE ( 'NONE', #35143, #33928 ) ;
#443 = ORIENTED_EDGE ( 'NONE', *, *, #11812, .T. ) ;
#444 = ORIENTED_EDGE ( 'NONE', *, *, #10489, .T. ) ;
#445 = CIRCLE ( 'NONE', #21413, 2.000000000000001776 ) ;
#446 = AXIS2_PLACEMENT_3D ( 'NONE', #13189, #27434, #32882 ) ;
#447 = CARTESIAN_POINT ( 'NONE',  ( -65.00000337463104927, -43.30127018922202353, -9.999999999999998224 ) ) ;
#448 = LINE ( 'NONE', #18241, #25630 ) ;
#449 = DIRECTION ( 'NONE',  ( 0.000000000000000000, 0.000000000000000000, 1.000000000000000000 ) ) ;
#450 = ORIENTED_EDGE ( 'NONE', *, *, #35879, .F. ) ;
#451 = CARTESIAN_POINT ( 'NONE',  ( 6.249999999999998224, 0.000000000000000000, -3.250000000000001332 ) ) ;
#452 = AXIS2_PLACEMENT_3D ( 'NONE', #7985, #34244, #8372 ) ;
#453 = DIRECTION ( 'NONE',  ( -0.000000000000000000, 0.000000000000000000, -1.000000000000000000 ) ) ;
#454 = CARTESIAN_POINT ( 'NONE',  ( 35.19434990244975126, -52.39915983220758022, 12.49999999999999822 ) ) ;
#455 = EDGE_CURVE ( 'NONE', #28642, #34166, #20183, .T. ) ;
#456 = ORIENTED_EDGE ( 'NONE', *, *, #33462, .T. ) ;
#457 = FACE_OUTER_BOUND ( 'NONE', #6118, .T. ) ;
#459 = CARTESIAN_POINT ( 'NONE',  ( -55.00000337463107059, 60.62177826491078747, -9.999999999999998224 ) ) ;
#458 = AXIS2_PLACEMENT_3D ( 'NONE', #31556, #28758, #23130 ) ;
#460 = VERTEX_POINT ( 'NONE', #14249 ) ;
#461 = EDGE_CURVE ( 'NONE', #15417, #12117, #25697, .T. ) ;
#462 = CARTESIAN_POINT ( 'NONE',  ( 79.83584911142594365, 32.64776363509508883, 12.50000000000000000 ) ) ;
#463 = AXIS2_PLACEMENT_3D ( 'NONE', #20717, #23541, #16991 ) ;
#464 = VECTOR ( 'NONE', #22327, 1000.000000000000000 ) ;
#465 = DIRECTION ( 'NONE',  ( 1.000000000000000000, 0.000000000000000000, 0.000000000000000000 ) ) ;
#466 = DIRECTION ( 'NONE',  ( 0.000000000000000000, 0.000000000000000000, -1.000000000000000000 ) ) ;
#468 = VECTOR ( 'NONE', #869, 1000.000000000000000 ) ;
#467 = CARTESIAN_POINT ( 'NONE',  ( 59.99999662536845335, 34.64101615137759893, -5.000000000000000000 ) ) ;
#469 = EDGE_CURVE ( 'NONE', #105, #36472, #11048, .T. ) ;
#470 = LINE ( 'NONE', #31594, #559 ) ;
#471 = CIRCLE ( 'NONE', #6443, 2.000000000000001776 ) ;
#472 = CARTESIAN_POINT ( 'NONE',  ( -37.00000337463116296, 60.62177826491077326, -5.000000000000000000 ) ) ;
#473 = ORIENTED_EDGE ( 'NONE', *, *, #22699, .T. ) ;
#474 = DIRECTION ( 'NONE',  ( 0.000000000000000000, 0.000000000000000000, 1.000000000000000000 ) ) ;
#475 = EDGE_CURVE ( 'NONE', #21726, #32663, #25496, .T. ) ;
#476 = DIRECTION ( 'NONE',  ( -1.000000000000000000, 0.000000000000000000, 0.000000000000000000 ) ) ;
#477 = DIRECTION ( 'NONE',  ( -0.000000000000000000, -0.000000000000000000, 1.000000000000000000 ) ) ;
#478 = ADVANCED_FACE ( 'NONE', ( #16501 ), #22494, .F. ) ;
#479 = ORIENTED_EDGE ( 'NONE', *, *, #28678, .T. ) ;
#480 = ORIENTED_EDGE ( 'NONE', *, *, #7602, .T. ) ;
#481 = ORIENTED_EDGE ( 'NONE', *, *, #15113, .F. ) ;
#482 = DIRECTION ( 'NONE',  ( 0.8660254037844347108, -0.5000000000000067724, 0.000000000000000000 ) ) ;
#483 = CARTESIAN_POINT ( 'NONE',  ( 35.99999999999999289, 0.000000000000000000, 2.445500000000000007 ) ) ;
#484 = DIRECTION ( 'NONE',  ( 0.000000000000000000, 0.000000000000000000, 1.000000000000000000 ) ) ;
#485 = CIRCLE ( 'NONE', #14278, 2.000000000000001776 ) ;
#486 = EDGE_CURVE ( 'NONE', #21666, #32300, #22317, .T. ) ;
#487 = EDGE_CURVE ( 'NONE', #18803, #9986, #30966, .T. ) ;
#488 = PRODUCT_DEFINITION_SHAPE ( 'NONE', 'NONE',  #14827 ) ;
#489 = EDGE_CURVE ( 'NONE', #8845, #17624, #29750, .T. ) ;
#490 = AXIS2_PLACEMENT_3D ( 'NONE', #34543, #3216, #9032 ) ;
#491 = CARTESIAN_POINT ( 'NONE',  ( 95.00000000000001421, 0.000000000000000000, 27.50000000000000000 ) ) ;
#493 = EDGE_CURVE ( 'NONE', #20027, #19694, #7016, .T. ) ;
#492 = ORIENTED_EDGE ( 'NONE', *, *, #13456, .T. ) ;
#494 = EDGE_CURVE ( 'NONE', #22235, #8449, #26177, .T. ) ;
#495 = DIRECTION ( 'NONE',  ( 0.000000000000000000, 0.000000000000000000, 1.000000000000000000 ) ) ;
#496 = ORIENTED_EDGE ( 'NONE', *, *, #6778, .F. ) ;
#497 = CIRCLE ( 'NONE', #16671, 2.000000000000001776 ) ;
#498 = AXIS2_PLACEMENT_3D ( 'NONE', #15560, #26807, #26606 ) ;
#499 = FACE_BOUND ( 'NONE', #23878, .T. ) ;
#500 = AXIS2_PLACEMENT_3D ( 'NONE', #24873, #22243, #28401 ) ;
#501 = VECTOR ( 'NONE', #13470, 1000.000000000000000 ) ;
#502 = DIRECTION ( 'NONE',  ( 0.000000000000000000, 0.000000000000000000, 1.000000000000000000 ) ) ;
#503 = CARTESIAN_POINT ( 'NONE',  ( 49.99999662536848177, -51.96152422706640550, -5.000000000000000000 ) ) ;
#504 = ORIENTED_EDGE ( 'NONE', *, *, #24797, .F. ) ;
#505 = CARTESIAN_POINT ( 'NONE',  ( 5.236872748402765509, 0.5087250997262705576, -4.057689166958450500 ) ) ;
#506 = APPLICATION_PROTOCOL_DEFINITION ( 'draft international standard', 'automotive_design', 1998, #5099 ) ;
#507 = AXIS2_PLACEMENT_3D ( 'NONE', #23833, #9582, #9188 ) ;
#508 = DIRECTION ( 'NONE',  ( 0.000000000000000000, 0.000000000000000000, 1.000000000000000000 ) ) ;
#509 = CIRCLE ( 'NONE', #25684, 33.00000000000001421 ) ;
#510 = CARTESIAN_POINT ( 'NONE',  ( -65.00000337463106348, -60.62177826491083010, -5.000000000000000000 ) ) ;
#511 = CARTESIAN_POINT ( 'NONE',  ( -6.284666409917640040E-14, -6.000000000000000000, 27.50000000000000000 ) ) ;
#512 = ORIENTED_EDGE ( 'NONE', *, *, #1242, .T. ) ;
#513 = CARTESIAN_POINT ( 'NONE',  ( 46.99999662536851019, 77.94228634059959404, -9.999999999999998224 ) ) ;
#514 = CARTESIAN_POINT ( 'NONE',  ( 79.99999662536833966, 34.64101615137759183, 12.50000000000000000 ) ) ;
#515 = AXIS2_PLACEMENT_3D ( 'NONE', #34654, #34457, #12285 ) ;
#516 = CARTESIAN_POINT ( 'NONE',  ( -77.00000337463097821, 43.30127018922197379, -9.999999999999998224 ) ) ;
#517 = ORIENTED_EDGE ( 'NONE', *, *, #24288, .F. ) ;
#518 = EDGE_LOOP ( 'NONE', ( #20740, #16897, #25527, #2907, #12930 ) ) ;
#519 = VECTOR ( 'NONE', #3730, 1000.000000000000000 ) ;
#520 = VERTEX_POINT ( 'NONE', #10263 ) ;
#521 = AXIS2_PLACEMENT_3D ( 'NONE', #20689, #29495, #32120 ) ;
#522 = LINE ( 'NONE', #18315, #353 ) ;
#523 = FACE_OUTER_BOUND ( 'NONE', #3503, .T. ) ;
#524 = VECTOR ( 'NONE', #22950, 1000.000000000000000 ) ;
#525 = CARTESIAN_POINT ( 'NONE',  ( 96.53048327204888324, -102.5304832720499633, 27.50000000000000000 ) ) ;
#526 = PLANE ( 'NONE',  #25503 ) ;
#527 = CARTESIAN_POINT ( 'NONE',  ( 149.8799519615616589, 5.999999999999476863, 32.55002500000000509 ) ) ;
#529 = CYLINDRICAL_SURFACE ( 'NONE', #4228, 2.000000000000000000 ) ;
#528 = CIRCLE ( 'NONE', #2341, 27.00000000000001421 ) ;
#530 = VERTEX_POINT ( 'NONE', #7444 ) ;
#532 = ORIENTED_EDGE ( 'NONE', *, *, #24422, .F. ) ;
#531 = EDGE_CURVE ( 'NONE', #35883, #4900, #15393, .T. ) ;
#533 = LINE ( 'NONE', #26023, #19487 ) ;
#534 = VECTOR ( 'NONE', #24717, 1000.000000000000000 ) ;
#535 = DIRECTION ( 'NONE',  ( 1.000000000000000000, 0.000000000000000000, 0.000000000000000000 ) ) ;
#536 = EDGE_CURVE ( 'NONE', #19811, #13357, #11783, .T. ) ;
#537 = CARTESIAN_POINT ( 'NONE',  ( -37.50000000000000000, 103.4105893997321886, 27.49999999999999645 ) ) ;
#538 = VERTEX_POINT ( 'NONE', #33526 ) ;
#539 = CARTESIAN_POINT ( 'NONE',  ( -3.374631303565411855E-06, -86.60254037844400443, 12.50000000000000000 ) ) ;
#540 = CIRCLE ( 'NONE', #34686, 5.999999999999999112 ) ;
#541 = ORIENTED_EDGE ( 'NONE', *, *, #11291, .F. ) ;
#542 = ORIENTED_EDGE ( 'NONE', *, *, #25215, .T. ) ;
#543 = AXIS2_PLACEMENT_3D ( 'NONE', #29779, #32409, #21345 ) ;
#544 = CARTESIAN_POINT ( 'NONE',  ( 40.98360655737705116, 111.1639425680974398, -19.99999999999999645 ) ) ;
#545 = VERTEX_POINT ( 'NONE', #15886 ) ;
#546 = CARTESIAN_POINT ( 'NONE',  ( -15.00000337463126066, 77.94228634059957983, 12.50000000000000000 ) ) ;
#547 = CARTESIAN_POINT ( 'NONE',  ( -25.00000337463120914, 77.94228634059957983, -5.000000000000000000 ) ) ;
#548 = PLANE ( 'NONE',  #20272 ) ;
#549 = AXIS2_PLACEMENT_3D ( 'NONE', #29523, #28026, #13587 ) ;
#550 = VERTEX_POINT ( 'NONE', #27865 ) ;
#551 = ORIENTED_EDGE ( 'NONE', *, *, #18723, .F. ) ;
#552 = AXIS2_PLACEMENT_3D ( 'NONE', #10097, #4282, #15895 ) ;
#553 = VERTEX_POINT ( 'NONE', #35970 ) ;
#554 = EDGE_CURVE ( 'NONE', #14180, #7296, #6835, .T. ) ;
#555 = ORIENTED_EDGE ( 'NONE', *, *, #20326, .T. ) ;
#556 = VECTOR ( 'NONE', #15858, 1000.000000000000000 ) ;
#557 = ORIENTED_EDGE ( 'NONE', *, *, #18007, .T. ) ;
#558 = CARTESIAN_POINT ( 'NONE',  ( -2.500000000000022204, 4.330127018922177662, 0.000000000000000000 ) ) ;
#559 = VECTOR ( 'NONE', #17364, 1000.000000000000000 ) ;
#560 = ORIENTED_EDGE ( 'NONE', *, *, #23769, .T. ) ;
#561 = DIRECTION ( 'NONE',  ( 0.000000000000000000, 0.000000000000000000, 1.000000000000000000 ) ) ;
#562 = CARTESIAN_POINT ( 'NONE',  ( 82.38629821025696742, 72.56049487126330177, 32.49999999999998579 ) ) ;
#563 = DIRECTION ( 'NONE',  ( 0.000000000000000000, 0.000000000000000000, 1.000000000000000000 ) ) ;
#564 = ORIENTED_EDGE ( 'NONE', *, *, #32404, .T. ) ;
#565 = DIRECTION ( 'NONE',  ( 1.000000000000000000, 0.000000000000000000, 0.000000000000000000 ) ) ;
#566 = ADVANCED_FACE ( 'NONE', ( #36328 ), #1621, .T. ) ;
#567 = CARTESIAN_POINT ( 'NONE',  ( 31.46585318596250502, 86.45172111230321832, -4.999999999999997335 ) ) ;
#568 = VECTOR ( 'NONE', #23561, 1000.000000000000000 ) ;
#569 = DIRECTION ( 'NONE',  ( 0.000000000000000000, 0.000000000000000000, 1.000000000000000000 ) ) ;
#570 = EDGE_LOOP ( 'NONE', ( #30471, #6213, #2466, #12851 ) ) ;
#571 = FACE_OUTER_BOUND ( 'NONE', #12516, .T. ) ;
#572 = CIRCLE ( 'NONE', #33545, 2.000000000000000000 ) ;
#573 = DIRECTION ( 'NONE',  ( 1.000000000000000000, 0.000000000000000000, 0.000000000000000000 ) ) ;
#574 = EDGE_LOOP ( 'NONE', ( #29728, #17619, #5808 ) ) ;
#575 = VERTEX_POINT ( 'NONE', #13630 ) ;
#576 = CARTESIAN_POINT ( 'NONE',  ( 3.368272016354729725, 78.44802294027070388, 32.49999999999999289 ) ) ;
#577 = DIRECTION ( 'NONE',  ( -0.000000000000000000, -0.000000000000000000, 1.000000000000000000 ) ) ;
#578 = EDGE_CURVE ( 'NONE', #33610, #19047, #7627, .T. ) ;
#579 = DIRECTION ( 'NONE',  ( 1.000000000000000000, 0.000000000000000000, 0.000000000000000000 ) ) ;
#580 = CARTESIAN_POINT ( 'NONE',  ( -4.999999999999999112, 2.691270400161067666, -1.881368198414903548 ) ) ;
#581 = ORIENTED_EDGE ( 'NONE', *, *, #7822, .T. ) ;
#582 = CIRCLE ( 'NONE', #23347, 2.000000000000001776 ) ;
#583 = DIRECTION ( 'NONE',  ( 1.000000000000000000, 0.000000000000000000, 0.000000000000000000 ) ) ;
#584 = CARTESIAN_POINT ( 'NONE',  ( -85.00000337463092137, 25.98076211353317433, -9.999999999999998224 ) ) ;
#585 = DIRECTION ( 'NONE',  ( 0.000000000000000000, -0.000000000000000000, 1.000000000000000000 ) ) ;
#586 = AXIS2_PLACEMENT_3D ( 'NONE', #7498, #4888, #30917 ) ;
#587 = ORIENTED_EDGE ( 'NONE', *, *, #4431, .F. ) ;
#588 = VECTOR ( 'NONE', #15784, 1000.000000000000000 ) ;
#589 = FACE_OUTER_BOUND ( 'NONE', #27728, .T. ) ;
#590 = CIRCLE ( 'NONE', #1189, 2.000000000000001776 ) ;
#591 = ORIENTED_EDGE ( 'NONE', *, *, #22851, .F. ) ;
#592 = DIRECTION ( 'NONE',  ( 1.000000000000000000, 0.000000000000000000, 0.000000000000000000 ) ) ;
#593 = CARTESIAN_POINT ( 'NONE',  ( 0.000000000000000000, 0.000000000000000000, -6.000000000000000000 ) ) ;
#594 = AXIS2_PLACEMENT_3D ( 'NONE', #28395, #2721, #11351 ) ;
#595 = EDGE_CURVE ( 'NONE', #13005, #8407, #4838, .T. ) ;
#596 = CARTESIAN_POINT ( 'NONE',  ( 4.279621169095998212, -62.97617850287780072, -4.999999999999997335 ) ) ;
#597 = ORIENTED_EDGE ( 'NONE', *, *, #25808, .T. ) ;
#598 = VERTEX_POINT ( 'NONE', #27124 ) ;
#599 = PLANE ( 'NONE',  #19659 ) ;
#600 = EDGE_CURVE ( 'NONE', #15155, #20425, #19004, .T. ) ;
#601 = DIRECTION ( 'NONE',  ( 0.000000000000000000, 0.000000000000000000, 1.000000000000000000 ) ) ;
#602 = CARTESIAN_POINT ( 'NONE',  ( -5.000003374631307729, 77.94228634059957983, -5.000000000000000000 ) ) ;
#603 = VERTEX_POINT ( 'NONE', #27313 ) ;
#604 = CARTESIAN_POINT ( 'NONE',  ( -10.00000337463125000, -86.60254037844400443, -9.999999999999998224 ) ) ;
#605 = FACE_BOUND ( 'NONE', #24109, .T. ) ;
#606 = CIRCLE ( 'NONE', #19787, 27.00000000000001421 ) ;
#607 = EDGE_CURVE ( 'NONE', #27018, #35698, #9402, .T. ) ;
#608 = CARTESIAN_POINT ( 'NONE',  ( 3.000000000000000000, 0.000000000000000000, 2.541999999999999815 ) ) ;
#609 = LINE ( 'NONE', #1339, #13284 ) ;
#610 = DIRECTION ( 'NONE',  ( -0.000000000000000000, -0.000000000000000000, 1.000000000000000000 ) ) ;
#611 = CIRCLE ( 'NONE', #14987, 2.000000000000000000 ) ;
#612 = EDGE_LOOP ( 'NONE', ( #26487, #9451, #450, #4104, #36029, #18289 ) ) ;
#613 = FACE_OUTER_BOUND ( 'NONE', #23040, .T. ) ;
#614 = FILL_AREA_STYLE ('',( #23664 ) ) ;
#615 = EDGE_CURVE ( 'NONE', #4570, #3560, #17776, .T. ) ;
#616 = AXIS2_PLACEMENT_3D ( 'NONE', #20434, #3187, #26434 ) ;
#617 = FACE_OUTER_BOUND ( 'NONE', #10249, .T. ) ;
#618 = ORIENTED_EDGE ( 'NONE', *, *, #36591, .T. ) ;
#619 = CARTESIAN_POINT ( 'NONE',  ( 1.999996625368710257, -69.28203230275519786, -9.999999999999998224 ) ) ;
#620 = CARTESIAN_POINT ( 'NONE',  ( -1.738521435313295838, 5.045405839192962816, -4.085926550512736455 ) ) ;
#621 = AXIS2_PLACEMENT_3D ( 'NONE', #34504, #28693, #34320 ) ;
#622 = DIRECTION ( 'NONE',  ( 0.000000000000000000, 0.000000000000000000, 1.000000000000000000 ) ) ;
#623 = VERTEX_POINT ( 'NONE', #30682 ) ;
#624 = ORIENTED_EDGE ( 'NONE', *, *, #18049, .F. ) ;
#625 = VERTEX_POINT ( 'NONE', #19092 ) ;
#626 = CARTESIAN_POINT ( 'NONE',  ( 3.357433326862127476, -3.835087656846213555, -0.07080520455423547355 ) ) ;
#627 = EDGE_CURVE ( 'NONE', #19009, #36783, #8211, .T. ) ;
#628 = DIRECTION ( 'NONE',  ( -1.000000000000000000, 0.000000000000000000, 0.000000000000000000 ) ) ;
#629 = DIRECTION ( 'NONE',  ( -0.000000000000000000, 0.000000000000000000, -1.000000000000000000 ) ) ;
#630 = VERTEX_POINT ( 'NONE', #10639 ) ;
#631 = EDGE_LOOP ( 'NONE', ( #37043, #1357 ) ) ;
#632 = DIRECTION ( 'NONE',  ( -0.000000000000000000, -0.000000000000000000, 1.000000000000000000 ) ) ;
#633 = EDGE_LOOP ( 'NONE', ( #17490, #25632, #16229, #1140, #21792 ) ) ;
#634 = CYLINDRICAL_SURFACE ( 'NONE', #1798, 2.000000000000001776 ) ;
#635 = ORIENTED_EDGE ( 'NONE', *, *, #13792, .F. ) ;
#636 = CARTESIAN_POINT ( 'NONE',  ( 52.39915983220795681, 35.19434990244919703, 12.49999999999999822 ) ) ;
#637 = ORIENTED_EDGE ( 'NONE', *, *, #2357, .T. ) ;
#638 = ORIENTED_EDGE ( 'NONE', *, *, #3699, .F. ) ;
#639 = EDGE_CURVE ( 'NONE', #14986, #12253, #2835, .T. ) ;
#640 = FACE_OUTER_BOUND ( 'NONE', #21210, .T. ) ;
#641 = CARTESIAN_POINT ( 'NONE',  ( -98.28784258492883907, 106.7731239591698937, 32.50000000000000000 ) ) ;
#642 = EDGE_CURVE ( 'NONE', #7415, #15541, #36961, .T. ) ;
#644 = CIRCLE ( 'NONE', #15017, 3.000000000000006661 ) ;
#643 = CYLINDRICAL_SURFACE ( 'NONE', #1498, 30.00000000000000000 ) ;
#645 = ORIENTED_EDGE ( 'NONE', *, *, #31138, .F. ) ;
#646 = DIRECTION ( 'NONE',  ( -0.000000000000000000, -0.000000000000000000, 1.000000000000000000 ) ) ;
#647 = FACE_OUTER_BOUND ( 'NONE', #33083, .T. ) ;
#648 = CARTESIAN_POINT ( 'NONE',  ( -5.000000000000001776, 2.092572385047308359, -4.100081683154419565 ) ) ;
#649 = ORIENTED_EDGE ( 'NONE', *, *, #1353, .F. ) ;
#650 = CARTESIAN_POINT ( 'NONE',  ( 82.99999662536831124, -25.98076211353319565, -9.999999999999998224 ) ) ;
#651 = DIRECTION ( 'NONE',  ( 1.000000000000000000, 0.000000000000000000, 0.000000000000000000 ) ) ;
#652 = ORIENTED_EDGE ( 'NONE', *, *, #5571, .T. ) ;
#653 = DIRECTION ( 'NONE',  ( 0.000000000000000000, 0.000000000000000000, 1.000000000000000000 ) ) ;
#654 = ADVANCED_FACE ( 'NONE', ( #5002 ), #21520, .F. ) ;
#655 = CARTESIAN_POINT ( 'NONE',  ( 14.99999662536859901, 77.94228634059957983, -9.999999999999998224 ) ) ;
#656 = DIRECTION ( 'NONE',  ( 0.000000000000000000, 0.000000000000000000, 1.000000000000000000 ) ) ;
#657 = CARTESIAN_POINT ( 'NONE',  ( 2.500000000000000000, 0.000000000000000000, -5.624496230895140947 ) ) ;
#658 = DIRECTION ( 'NONE',  ( -0.000000000000000000, -0.000000000000000000, 1.000000000000000000 ) ) ;
#659 = EDGE_CURVE ( 'NONE', #25006, #4037, #16002, .T. ) ;
#660 = LINE ( 'NONE', #31939, #34328 ) ;
#661 = ORIENTED_EDGE ( 'NONE', *, *, #1413, .T. ) ;
#662 = FACE_OUTER_BOUND ( 'NONE', #1246, .T. ) ;
#663 = CARTESIAN_POINT ( 'NONE',  ( 62.99999662536841072, 25.98076211353318854, 17.49999999999999645 ) ) ;
#664 = DIRECTION ( 'NONE',  ( 1.000000000000000000, 0.000000000000000000, 0.000000000000000000 ) ) ;
#665 = ORIENTED_EDGE ( 'NONE', *, *, #34374, .T. ) ;
#666 = VERTEX_POINT ( 'NONE', #28244 ) ;
#667 = ORIENTED_EDGE ( 'NONE', *, *, #30676, .T. ) ;
#668 = CIRCLE ( 'NONE', #30002, 2.000000000000000000 ) ;
#669 = DIRECTION ( 'NONE',  ( 1.000000000000000000, 0.000000000000000000, 0.000000000000000000 ) ) ;
#670 = CARTESIAN_POINT ( 'NONE',  ( 0.000000000000000000, 0.000000000000000000, 12.49999999999999822 ) ) ;
#671 = CARTESIAN_POINT ( 'NONE',  ( -78.00000337463094979, 17.32050807568878525, -5.000000000000000000 ) ) ;
#672 = CARTESIAN_POINT ( 'NONE',  ( 67.99999662536836809, -51.96152422706639840, 12.50000000000000000 ) ) ;
#673 = EDGE_CURVE ( 'NONE', #16100, #33530, #36691, .T. ) ;
#674 = DIRECTION ( 'NONE',  ( 0.000000000000000000, 0.000000000000000000, 1.000000000000000000 ) ) ;
#675 = ORIENTED_EDGE ( 'NONE', *, *, #18137, .F. ) ;
#676 = DIRECTION ( 'NONE',  ( 1.000000000000000000, 0.000000000000000000, 0.000000000000000000 ) ) ;
#677 = ORIENTED_EDGE ( 'NONE', *, *, #11143, .T. ) ;
#678 = FACE_BOUND ( 'NONE', #26621, .T. ) ;
#679 = EDGE_CURVE ( 'NONE', #31822, #13995, #25431, .T. ) ;
#680 = FACE_OUTER_BOUND ( 'NONE', #28882, .T. ) ;
#681 = EDGE_CURVE ( 'NONE', #4131, #30183, #32146, .T. ) ;
#682 = DIRECTION ( 'NONE',  ( 1.000000000000000000, 0.000000000000000000, 0.000000000000000000 ) ) ;
#683 = EDGE_CURVE ( 'NONE', #26110, #31910, #34436, .T. ) ;
#684 = EDGE_LOOP ( 'NONE', ( #31991, #3562, #3930, #7996 ) ) ;
#685 = DIRECTION ( 'NONE',  ( 0.000000000000000000, 0.000000000000000000, 1.000000000000000000 ) ) ;
#686 = CIRCLE ( 'NONE', #33621, 3.000000000000007550 ) ;
#687 = CARTESIAN_POINT ( 'NONE',  ( 47.63139720814438505, -27.49999999999955946, 10.70000000000000107 ) ) ;
#688 = CARTESIAN_POINT ( 'NONE',  ( 29.99999662536857770, -69.28203230275519786, 12.50000000000000000 ) ) ;
#689 = DIRECTION ( 'NONE',  ( -0.000000000000000000, 1.625241993126352989E-15, 1.000000000000000000 ) ) ;
#690 = DIRECTION ( 'NONE',  ( 0.000000000000000000, 0.000000000000000000, -1.000000000000000000 ) ) ;
#691 = VERTEX_POINT ( 'NONE', #5196 ) ;
#692 = CYLINDRICAL_SURFACE ( 'NONE', #6427, 5.750000000000005329 ) ;
#693 = DIRECTION ( 'NONE',  ( -1.000000000000000000, 0.000000000000000000, 0.000000000000000000 ) ) ;
#694 = CARTESIAN_POINT ( 'NONE',  ( 149.8799519615616589, 5.999999999999476863, 27.50000000000000000 ) ) ;
#695 = VERTEX_POINT ( 'NONE', #8386 ) ;
#696 = ORIENTED_EDGE ( 'NONE', *, *, #22729, .F. ) ;
#697 = EDGE_CURVE ( 'NONE', #34083, #21168, #25636, .T. ) ;
#698 = VERTEX_POINT ( 'NONE', #11372 ) ;
#699 = DIRECTION ( 'NONE',  ( -0.000000000000000000, -0.000000000000000000, -1.000000000000000000 ) ) ;
#700 = PLANE ( 'NONE',  #28473 ) ;
#701 = ORIENTED_EDGE ( 'NONE', *, *, #12852, .F. ) ;
#702 = CIRCLE ( 'NONE', #28823, 2.000000000000001776 ) ;
#703 = CARTESIAN_POINT ( 'NONE',  ( -83.00000337463092137, -25.98076211353322051, -9.999999999999998224 ) ) ;
#704 = DIRECTION ( 'NONE',  ( -1.000000000000000000, 0.000000000000000000, 0.000000000000000000 ) ) ;
#705 = FACE_OUTER_BOUND ( 'NONE', #31997, .T. ) ;
#706 = EDGE_LOOP ( 'NONE', ( #6808, #12784, #32734, #8007 ) ) ;
#707 = ORIENTED_EDGE ( 'NONE', *, *, #14675, .T. ) ;
#708 = CARTESIAN_POINT ( 'NONE',  ( -45.00000337463112743, -60.62177826491080168, 12.50000000000000000 ) ) ;
#709 = EDGE_CURVE ( 'NONE', #31147, #12977, #28614, .T. ) ;
#710 = FACE_OUTER_BOUND ( 'NONE', #35150, .T. ) ;
#711 = EDGE_CURVE ( 'NONE', #22882, #22692, #14376, .T. ) ;
#712 = DIRECTION ( 'NONE',  ( 0.000000000000000000, 0.000000000000000000, 1.000000000000000000 ) ) ;
#713 = ORIENTED_EDGE ( 'NONE', *, *, #26824, .T. ) ;
#714 = FACE_BOUND ( 'NONE', #20933, .T. ) ;
#715 = EDGE_LOOP ( 'NONE', ( #3359, #25390, #2714, #32200 ) ) ;
#716 = VERTEX_POINT ( 'NONE', #23179 ) ;
#717 = EDGE_CURVE ( 'NONE', #28135, #24339, #28066, .T. ) ;
#718 = CARTESIAN_POINT ( 'NONE',  ( -65.00000337463102085, 25.98076211353317433, -9.999999999999998224 ) ) ;
#719 = VERTEX_POINT ( 'NONE', #31606 ) ;
#720 =( NAMED_UNIT ( * ) SI_UNIT ( $, .STERADIAN. ) SOLID_ANGLE_UNIT ( ) );
#721 = CARTESIAN_POINT ( 'NONE',  ( 40.98360655737705116, 111.1639425680974398, 27.49999999999999645 ) ) ;
#722 = CIRCLE ( 'NONE', #22285, 27.00000000000001776 ) ;
#723 = CYLINDRICAL_SURFACE ( 'NONE', #543, 2.000000000000001776 ) ;
#724 = DIRECTION ( 'NONE',  ( 0.000000000000000000, -1.034244904716769672E-15, -1.000000000000000000 ) ) ;
#725 = VERTEX_POINT ( 'NONE', #2743 ) ;
#726 = ORIENTED_EDGE ( 'NONE', *, *, #70, .F. ) ;
#727 = EDGE_CURVE ( 'NONE', #10440, #26731, #22992, .T. ) ;
#728 = ORIENTED_EDGE ( 'NONE', *, *, #34251, .T. ) ;
#729 = EDGE_CURVE ( 'NONE', #6234, #9776, #26632, .T. ) ;
#730 = ORIENTED_EDGE ( 'NONE', *, *, #12828, .F. ) ;
#731 = VERTEX_POINT ( 'NONE', #2393 ) ;
#732 = EDGE_CURVE ( 'NONE', #13981, #15311, #19439, .T. ) ;
#733 = DIRECTION ( 'NONE',  ( -1.000000000000000000, 0.000000000000000000, -0.000000000000000000 ) ) ;
#734 = EDGE_CURVE ( 'NONE', #35238, #6394, #7477, .T. ) ;
#735 = CARTESIAN_POINT ( 'NONE',  ( -37.50000000000000000, -103.4105893997321743, 32.50000000000000000 ) ) ;
#736 = ORIENTED_EDGE ( 'NONE', *, *, #15630, .T. ) ;
#737 = FACE_BOUND ( 'NONE', #17060, .T. ) ;
#738 = CARTESIAN_POINT ( 'NONE',  ( 105.8342059669409281, 39.11274920687675660, 32.50000000000000000 ) ) ;
#739 = DIRECTION ( 'NONE',  ( 1.000000000000000000, 0.000000000000000000, 0.000000000000000000 ) ) ;
#740 = ORIENTED_EDGE ( 'NONE', *, *, #13061, .T. ) ;
#741 = CARTESIAN_POINT ( 'NONE',  ( -22.00000337463124112, 69.28203230275516944, -9.999999999999998224 ) ) ;
#742 = AXIS2_PLACEMENT_3D ( 'NONE', #35133, #6623, #15055 ) ;
#743 = DIRECTION ( 'NONE',  ( -1.000000000000000000, 0.000000000000000000, 0.000000000000000000 ) ) ;
#744 = PLANE ( 'NONE',  #1446 ) ;
#745 = VERTEX_POINT ( 'NONE', #8736 ) ;
#746 = CARTESIAN_POINT ( 'NONE',  ( 13.89091430021463935, 62.33939050065170306, 12.49999999999999822 ) ) ;
#747 = CYLINDRICAL_SURFACE ( 'NONE', #18394, 2.000000000000001776 ) ;
#748 = ORIENTED_EDGE ( 'NONE', *, *, #21903, .T. ) ;
#749 = EDGE_LOOP ( 'NONE', ( #27988, #21421, #30787, #25803 ) ) ;
#750 = CARTESIAN_POINT ( 'NONE',  ( -7.041719095097282852E-16, 78.44802294027068967, 32.49999999999999289 ) ) ;
#751 = FACE_OUTER_BOUND ( 'NONE', #21916, .T. ) ;
#752 = DIRECTION ( 'NONE',  ( 0.000000000000000000, 0.000000000000000000, 1.000000000000000000 ) ) ;
#753 = AXIS2_PLACEMENT_3D ( 'NONE', #3835, #26714, #32706 ) ;
#754 = CARTESIAN_POINT ( 'NONE',  ( -4.999999999999999112, 1.831554690317574341, -1.158389257021580576 ) ) ;
#755 = VERTEX_POINT ( 'NONE', #25262 ) ;
#756 = ADVANCED_FACE ( 'NONE', ( #5558 ), #5945, .F. ) ;
#757 = CARTESIAN_POINT ( 'NONE',  ( -62.00000337463104927, 34.64101615137757051, 12.50000000000000000 ) ) ;
#758 = DIRECTION ( 'NONE',  ( 1.000000000000000000, 0.000000000000000000, 0.000000000000000000 ) ) ;
#759 = ORIENTED_EDGE ( 'NONE', *, *, #20397, .T. ) ;
#760 = CARTESIAN_POINT ( 'NONE',  ( -68.00000337463099243, 34.64101615137758472, 17.49999999999999645 ) ) ;
#761 = ORIENTED_EDGE ( 'NONE', *, *, #12359, .F. ) ;
#762 = FACE_OUTER_BOUND ( 'NONE', #15936, .T. ) ;
#763 = DIRECTION ( 'NONE',  ( 1.000000000000000000, 0.000000000000000000, 0.000000000000000000 ) ) ;
#764 = CARTESIAN_POINT ( 'NONE',  ( -5.000000000000000000, 24.49489742783178414, 15.00000000000000000 ) ) ;
#765 = ORIENTED_EDGE ( 'NONE', *, *, #33305, .T. ) ;
#766 = ORIENTED_EDGE ( 'NONE', *, *, #35554, .F. ) ;
#767 = LINE ( 'NONE', #10464, #5296 ) ;
#768 = DIRECTION ( 'NONE',  ( 0.000000000000000000, 0.000000000000000000, 1.000000000000000000 ) ) ;
#769 = LINE ( 'NONE', #35993, #5932 ) ;
#770 = ORIENTED_EDGE ( 'NONE', *, *, #3390, .F. ) ;
#771 = CARTESIAN_POINT ( 'NONE',  ( -72.00000337463100664, -17.32050807568882078, 17.49999999999999645 ) ) ;
#772 = CIRCLE ( 'NONE', #2581, 3.000000000000002665 ) ;
#773 = ADVANCED_FACE ( 'NONE', ( #14178 ), #33878, .F. ) ;
#774 = B_SPLINE_CURVE_WITH_KNOTS ( 'NONE', 3,
 ( #8176, #19617, #16816, #18875, #13614, #30843 ),
 .UNSPECIFIED., .F., .F.,
 ( 4, 2, 4 ),
 ( 0.000000000000000000, 0.0002514304509865738471, 0.0005028609019731476943 ),
 .UNSPECIFIED. ) ;
#775 = FACE_BOUND ( 'NONE', #29543, .T. ) ;
#776 = DIRECTION ( 'NONE',  ( 0.000000000000000000, 0.000000000000000000, 1.000000000000000000 ) ) ;
#777 = CARTESIAN_POINT ( 'NONE',  ( 0.000000000000000000, 0.000000000000000000, 2.266666666666666607 ) ) ;
#778 = DIRECTION ( 'NONE',  ( 0.000000000000000000, 0.000000000000000000, 1.000000000000000000 ) ) ;
#779 = ORIENTED_EDGE ( 'NONE', *, *, #8998, .T. ) ;
#780 = CARTESIAN_POINT ( 'NONE',  ( 62.99999662536839651, -43.30127018922199511, -5.000000000000000000 ) ) ;
#781 = PRODUCT_DEFINITION_SHAPE ( 'NONE', 'NONE',  #37111 ) ;
#782 = CARTESIAN_POINT ( 'NONE',  ( -2.500000000000000444, 3.061616997868383634E-16, -5.700000000000000178 ) ) ;
#783 = CARTESIAN_POINT ( 'NONE',  ( -32.00000337463119848, -69.28203230275522628, -9.999999999999998224 ) ) ;
#784 = ORIENTED_EDGE ( 'NONE', *, *, #3551, .F. ) ;
#785 = DIRECTION ( 'NONE',  ( -0.000000000000000000, -0.000000000000000000, -1.000000000000000000 ) ) ;
#786 = CARTESIAN_POINT ( 'NONE',  ( 36.97203788309026606, -58.48108235278833433, -4.999999999999997335 ) ) ;
#787 = AXIS2_PLACEMENT_3D ( 'NONE', #34385, #9057, #8687 ) ;
#788 = CARTESIAN_POINT ( 'NONE',  ( -60.00000337463108480, -51.96152422706641971, -9.999999999999998224 ) ) ;
#789 = ORIENTED_EDGE ( 'NONE', *, *, #19478, .T. ) ;
#790 = AXIS2_PLACEMENT_3D ( 'NONE', #20031, #32206, #6536 ) ;
#791 = EDGE_LOOP ( 'NONE', ( #7696, #29616, #13253, #10658 ) ) ;
#792 = VERTEX_POINT ( 'NONE', #3121 ) ;
#793 = CARTESIAN_POINT ( 'NONE',  ( 4.191707736911197912, -3.353419101626359478, -0.2701150775514091773 ) ) ;
#794 = DIRECTION ( 'NONE',  ( 1.000000000000000000, 0.000000000000000000, 0.000000000000000000 ) ) ;
#795 = DIRECTION ( 'NONE',  ( -1.000000000000000000, 0.000000000000000000, 0.000000000000000000 ) ) ;
#796 = ORIENTED_EDGE ( 'NONE', *, *, #30510, .T. ) ;
#797 = ORIENTED_EDGE ( 'NONE', *, *, #31619, .F. ) ;
#798 = EDGE_LOOP ( 'NONE', ( #23448, #6697, #696, #2063 ) ) ;
#799 = EDGE_CURVE ( 'NONE', #33595, #36282, #8557, .T. ) ;
#800 = EDGE_CURVE ( 'NONE', #167, #22384, #5680, .T. ) ;
#801 = AXIS2_PLACEMENT_3D ( 'NONE', #454, #8709, #11888 ) ;
#802 = LINE ( 'NONE', #10191, #24500 ) ;
#803 = CIRCLE ( 'NONE', #9770, 2.000000000000001776 ) ;
#804 = ORIENTED_EDGE ( 'NONE', *, *, #25973, .T. ) ;
#805 = CARTESIAN_POINT ( 'NONE',  ( 2.577124608817066953, -119.9999535335656162, 32.50000000000000000 ) ) ;
#806 = EDGE_CURVE ( 'NONE', #8770, #16892, #29355, .T. ) ;
#807 = VERTEX_POINT ( 'NONE', #1041 ) ;
#808 = CYLINDRICAL_SURFACE ( 'NONE', #12350, 2.000000000000000000 ) ;
#809 = EDGE_LOOP ( 'NONE', ( #29970, #18235 ) ) ;
#810 = AXIS2_PLACEMENT_3D ( 'NONE', #9275, #29702, #32516 ) ;
#811 = ORIENTED_EDGE ( 'NONE', *, *, #30891, .F. ) ;
#812 = EDGE_CURVE ( 'NONE', #10608, #13259, #17726, .T. ) ;
#813 = CYLINDRICAL_SURFACE ( 'NONE', #32755, 30.00000000000000000 ) ;
#814 = FACE_BOUND ( 'NONE', #2745, .T. ) ;
#815 = CARTESIAN_POINT ( 'NONE',  ( -23.49188638668713480, -103.5527587461262442, 32.50001250000000397 ) ) ;
#816 = VERTEX_POINT ( 'NONE', #31784 ) ;
#817 = ORIENTED_EDGE ( 'NONE', *, *, #3496, .F. ) ;
#818 = CARTESIAN_POINT ( 'NONE',  ( 84.99999662536831124, -25.98076211353319565, 12.50000000000000000 ) ) ;
#819 = DIRECTION ( 'NONE',  ( 0.000000000000000000, 0.000000000000000000, 1.000000000000000000 ) ) ;
#820 = CARTESIAN_POINT ( 'NONE',  ( -45.00000337463111322, 60.62177826491077326, -5.000000000000000000 ) ) ;
#821 = CIRCLE ( 'NONE', #26565, 2.000000000000001776 ) ;
#822 = ORIENTED_EDGE ( 'NONE', *, *, #12407, .F. ) ;
#823 = CARTESIAN_POINT ( 'NONE',  ( -70.00000337463102085, -51.96152422706641971, 12.50000000000000000 ) ) ;
#824 = LINE ( 'NONE', #20902, #10192 ) ;
#825 = ORIENTED_EDGE ( 'NONE', *, *, #23189, .T. ) ;
#826 = EDGE_CURVE ( 'NONE', #5699, #16797, #15258, .T. ) ;
#827 = DIRECTION ( 'NONE',  ( 1.000000000000000000, 0.000000000000000000, 0.000000000000000000 ) ) ;
#828 = LINE ( 'NONE', #12240, #30455 ) ;
#829 = DIRECTION ( 'NONE',  ( 0.000000000000000000, 0.000000000000000000, -1.000000000000000000 ) ) ;
#830 = CARTESIAN_POINT ( 'NONE',  ( -8.000003374631278419, -69.28203230275519786, 17.49999999999999645 ) ) ;
#831 = AXIS2_PLACEMENT_3D ( 'NONE', #34408, #28226, #31762 ) ;
#832 = DIRECTION ( 'NONE',  ( 1.000000000000000000, 0.000000000000000000, 0.000000000000000000 ) ) ;
#833 = AXIS2_PLACEMENT_3D ( 'NONE', #2841, #5634, #5469 ) ;
#834 = LINE ( 'NONE', #21084, #6157 ) ;
#835 = EDGE_LOOP ( 'NONE', ( #25371, #30049 ) ) ;
#836 = CARTESIAN_POINT ( 'NONE',  ( 74.99999662536836809, -8.660254037844401509, -5.000000000000000000 ) ) ;
#837 = CARTESIAN_POINT ( 'NONE',  ( -68.00000337463102085, -34.64101615137762025, -5.000000000000000000 ) ) ;
#838 = DIRECTION ( 'NONE',  ( -1.000000000000000000, 0.000000000000000000, 0.000000000000000000 ) ) ;
#839 = ORIENTED_EDGE ( 'NONE', *, *, #21442, .F. ) ;
#840 = EDGE_LOOP ( 'NONE', ( #9665, #15054 ) ) ;
#841 = ORIENTED_EDGE ( 'NONE', *, *, #18335, .T. ) ;
#842 = ADVANCED_FACE ( 'NONE', ( #26365 ), #3674, .F. ) ;
#843 = PLANE ( 'NONE',  #24821 ) ;
#844 = FACE_OUTER_BOUND ( 'NONE', #14924, .T. ) ;
#845 = CARTESIAN_POINT ( 'NONE',  ( -6.069707180676227632E-15, 5.773502691896268857, -5.700000000000000178 ) ) ;
#846 = AXIS2_PLACEMENT_3D ( 'NONE', #8926, #5744, #482 ) ;
#847 = CARTESIAN_POINT ( 'NONE',  ( 29.99999662536856349, 69.28203230275518365, 17.49999999999999645 ) ) ;
#848 = CARTESIAN_POINT ( 'NONE',  ( -72.00000337463100664, -2.404119930384582903E-14, -9.999999999999998224 ) ) ;
#849 = ORIENTED_EDGE ( 'NONE', *, *, #6512, .F. ) ;
#850 = CARTESIAN_POINT ( 'NONE',  ( -83.00000337463092137, -8.660254037844422825, -9.999999999999998224 ) ) ;
#851 = EDGE_CURVE ( 'NONE', #36107, #18101, #12892, .T. ) ;
#852 = ORIENTED_EDGE ( 'NONE', *, *, #32604, .T. ) ;
#853 = FACE_BOUND ( 'NONE', #31139, .T. ) ;
#854 = AXIS2_PLACEMENT_3D ( 'NONE', #593, #17839, #15403 ) ;
#855 = EDGE_CURVE ( 'NONE', #30871, #2722, #28965, .T. ) ;
#856 = CARTESIAN_POINT ( 'NONE',  ( 19.31922176934805435, 76.99660315353983719, -11.00000000000000000 ) ) ;
#857 = CIRCLE ( 'NONE', #21821, 2.000000000000001776 ) ;
#858 = CARTESIAN_POINT ( 'NONE',  ( 0.000000000000000000, 0.000000000000000000, -5.000000000000000000 ) ) ;
#859 = VERTEX_POINT ( 'NONE', #6113 ) ;
#860 = LINE ( 'NONE', #3858, #22442 ) ;
#861 = DIRECTION ( 'NONE',  ( 0.000000000000000000, 0.000000000000000000, 1.000000000000000000 ) ) ;
#862 = DIRECTION ( 'NONE',  ( -1.000000000000000000, 0.000000000000000000, 0.000000000000000000 ) ) ;
#863 = AXIS2_PLACEMENT_3D ( 'NONE', #5084, #16525, #22516 ) ;
#864 = FACE_OUTER_BOUND ( 'NONE', #1884, .T. ) ;
#865 = DIRECTION ( 'NONE',  ( 1.000000000000000000, 0.000000000000000000, 0.000000000000000000 ) ) ;
#866 = ORIENTED_EDGE ( 'NONE', *, *, #31804, .F. ) ;
#867 = CARTESIAN_POINT ( 'NONE',  ( 51.67316999614278217, 68.18636315956837279, 12.50000000000000000 ) ) ;
#868 = VECTOR ( 'NONE', #29592, 1000.000000000000000 ) ;
#869 = DIRECTION ( 'NONE',  ( 0.000000000000000000, 0.000000000000000000, 1.000000000000000000 ) ) ;
#870 = CARTESIAN_POINT ( 'NONE',  ( 69.99999662536839651, -3.469446951953614189E-15, 12.50000000000000000 ) ) ;
#871 = ORIENTED_EDGE ( 'NONE', *, *, #36928, .T. ) ;
#872 = AXIS2_PLACEMENT_3D ( 'NONE', #12562, #12163, #34891 ) ;
#873 = EDGE_CURVE ( 'NONE', #24444, #18009, #21278, .T. ) ;
#874 = ORIENTED_EDGE ( 'NONE', *, *, #19101, .F. ) ;
#875 = VERTEX_POINT ( 'NONE', #6840 ) ;
#876 = CARTESIAN_POINT ( 'NONE',  ( 9.999996625368655856, -86.60254037844400443, -5.000000000000000000 ) ) ;
#877 = CARTESIAN_POINT ( 'NONE',  ( -72.72667006429185221, -101.6652913307173662, 27.50000000000000000 ) ) ;
#878 = VECTOR ( 'NONE', #28436, 1000.000000000000000 ) ;
#879 = EDGE_CURVE ( 'NONE', #21303, #29936, #13484, .T. ) ;
#880 = AXIS2_PLACEMENT_3D ( 'NONE', #11968, #17424, #28839 ) ;
#881 = AXIS2_PLACEMENT_3D ( 'NONE', #8194, #34259, #31066 ) ;
#882 = CARTESIAN_POINT ( 'NONE',  ( 0.000000000000000000, 0.000000000000000000, -4.599999999999999645 ) ) ;
#883 = AXIS2_PLACEMENT_3D ( 'NONE', #35948, #19415, #7250 ) ;
#884 = EDGE_CURVE ( 'NONE', #12035, #22989, #33869, .T. ) ;
#885 = CARTESIAN_POINT ( 'NONE',  ( -77.00000337463097821, 43.30127018922197379, -9.999999999999998224 ) ) ;
#886 = CARTESIAN_POINT ( 'NONE',  ( 57.99999662536842493, -51.96152422706639840, 12.50000000000000000 ) ) ;
#887 = DIRECTION ( 'NONE',  ( 0.000000000000000000, 0.000000000000000000, 1.000000000000000000 ) ) ;
#888 = ORIENTED_EDGE ( 'NONE', *, *, #23980, .F. ) ;
#889 = ORIENTED_EDGE ( 'NONE', *, *, #8422, .F. ) ;
#890 = CARTESIAN_POINT ( 'NONE',  ( 3.000000000000000000, 2.935248768560057453, -3.903127820947815962E-15 ) ) ;
#891 = CARTESIAN_POINT ( 'NONE',  ( -51.68138994340220904, -113.8157894736842053, 32.50002500000000083 ) ) ;
#892 = ORIENTED_EDGE ( 'NONE', *, *, #31404, .F. ) ;
#893 = CARTESIAN_POINT ( 'NONE',  ( -5.170224855064533998, -2.788471980053888188, -4.289066185948688492 ) ) ;
#894 = ORIENTED_EDGE ( 'NONE', *, *, #9878, .T. ) ;
#895 = B_SPLINE_CURVE_WITH_KNOTS ( 'NONE', 3,
 ( #8671, #10768, #25766, #37009, #36459, #33643 ),
 .UNSPECIFIED., .F., .F.,
 ( 4, 2, 4 ),
 ( 0.003058795990767219572, 0.004586520967003283183, 0.006114245943239346795 ),
 .UNSPECIFIED. ) ;
#896 = VECTOR ( 'NONE', #1089, 1000.000000000000000 ) ;
#897 = EDGE_CURVE ( 'NONE', #17193, #19877, #2112, .T. ) ;
#898 = FACE_BOUND ( 'NONE', #36335, .T. ) ;
#899 = ORIENTED_EDGE ( 'NONE', *, *, #233, .T. ) ;
#900 = ORIENTED_EDGE ( 'NONE', *, *, #13295, .F. ) ;
#901 = CARTESIAN_POINT ( 'NONE',  ( -94.55012560584668790, 9.234378588655390629, 27.50000000000000000 ) ) ;
#902 = VERTEX_POINT ( 'NONE', #671 ) ;
#903 = CARTESIAN_POINT ( 'NONE',  ( -63.10544949267008974, -59.98094631475026262, -5.000000000000000000 ) ) ;
#904 = DIRECTION ( 'NONE',  ( 1.000000000000000000, 0.000000000000000000, 0.000000000000000000 ) ) ;
#905 = DIRECTION ( 'NONE',  ( 0.000000000000000000, 0.000000000000000000, 1.000000000000000000 ) ) ;
#906 = EDGE_LOOP ( 'NONE', ( #34279, #5541, #36794 ) ) ;
#907 = ORIENTED_EDGE ( 'NONE', *, *, #26589, .T. ) ;
#908 = ORIENTED_EDGE ( 'NONE', *, *, #1147, .T. ) ;
#909 = EDGE_LOOP ( 'NONE', ( #21439, #34161, #11256, #12333, #4938 ) ) ;
#910 = EDGE_CURVE ( 'NONE', #8144, #9228, #21096, .T. ) ;
#911 = VERTEX_POINT ( 'NONE', #18278 ) ;
#913 = DIRECTION ( 'NONE',  ( 0.000000000000000000, 0.000000000000000000, 1.000000000000000000 ) ) ;
#912 = AXIS2_PLACEMENT_3D ( 'NONE', #18681, #29729, #36300 ) ;
#914 = DIRECTION ( 'NONE',  ( 0.000000000000000000, 0.000000000000000000, 1.000000000000000000 ) ) ;
#915 = EDGE_CURVE ( 'NONE', #21808, #7036, #34459, .T. ) ;
#916 = ORIENTED_EDGE ( 'NONE', *, *, #2941, .T. ) ;
#917 = AXIS2_PLACEMENT_3D ( 'NONE', #8500, #13762, #25212 ) ;
#918 = CARTESIAN_POINT ( 'NONE',  ( -35.00000337463116296, 60.62177826491077326, -9.999999999999998224 ) ) ;
#919 = DIRECTION ( 'NONE',  ( 0.000000000000000000, 0.000000000000000000, -1.000000000000000000 ) ) ;
#920 = CARTESIAN_POINT ( 'NONE',  ( 65.44550000000002399, 0.000000000000000000, 0.000000000000000000 ) ) ;
#921 = CIRCLE ( 'NONE', #14715, 27.00000000000001066 ) ;
#922 = EDGE_LOOP ( 'NONE', ( #32769, #22190, #15278, #22129 ) ) ;
#923 = AXIS2_PLACEMENT_3D ( 'NONE', #31422, #14380, #8742 ) ;
#924 = FACE_OUTER_BOUND ( 'NONE', #20592, .T. ) ;
#925 = EDGE_CURVE ( 'NONE', #25902, #22136, #23069, .T. ) ;
#926 = AXIS2_PLACEMENT_3D ( 'NONE', #28788, #28957, #26356 ) ;
#927 = CARTESIAN_POINT ( 'NONE',  ( 46.00000000000000000, 103.4105893997321743, -19.99999999999999645 ) ) ;
#928 = AXIS2_PLACEMENT_3D ( 'NONE', #26837, #26283, #3955 ) ;
#929 = CARTESIAN_POINT ( 'NONE',  ( 37.99999662536853151, -69.28203230275519786, 12.50000000000000000 ) ) ;
#930 = ORIENTED_EDGE ( 'NONE', *, *, #5467, .F. ) ;
#931 = PLANE ( 'NONE',  #1685 ) ;
#932 = EDGE_CURVE ( 'NONE', #8794, #23016, #6904, .T. ) ;
#933 = DIRECTION ( 'NONE',  ( 1.000000000000000000, 0.000000000000000000, 0.000000000000000000 ) ) ;
#934 = EDGE_CURVE ( 'NONE', #953, #6746, #26534, .T. ) ;
#935 = ORIENTED_EDGE ( 'NONE', *, *, #19624, .F. ) ;
#936 = AXIS2_PLACEMENT_3D ( 'NONE', #30512, #16262, #33521 ) ;
#937 = ORIENTED_EDGE ( 'NONE', *, *, #24324, .F. ) ;
#938 = LINE ( 'NONE', #12358, #6254 ) ;
#939 = LINE ( 'NONE', #6031, #30693 ) ;
#940 = DIRECTION ( 'NONE',  ( 0.000000000000000000, 0.000000000000000000, 1.000000000000000000 ) ) ;
#941 = DIRECTION ( 'NONE',  ( 0.000000000000000000, 0.000000000000000000, 1.000000000000000000 ) ) ;
#942 = VERTEX_POINT ( 'NONE', #35187 ) ;
#943 = EDGE_CURVE ( 'NONE', #36107, #2483, #9102, .T. ) ;
#944 = DIRECTION ( 'NONE',  ( 0.000000000000000000, 0.000000000000000000, 1.000000000000000000 ) ) ;
#945 = EDGE_CURVE ( 'NONE', #2623, #23562, #30850, .T. ) ;
#946 = CARTESIAN_POINT ( 'NONE',  ( 64.99999662536839651, -60.62177826491080168, 17.49999999999999645 ) ) ;
#947 = ADVANCED_FACE ( 'NONE', ( #26919 ), #20364, .F. ) ;
#948 = ORIENTED_EDGE ( 'NONE', *, *, #26845, .F. ) ;
#949 = EDGE_CURVE ( 'NONE', #34902, #24063, #3319, .T. ) ;
#950 = EDGE_CURVE ( 'NONE', #15883, #26378, #23725, .T. ) ;
#951 = CIRCLE ( 'NONE', #25501, 65.00000000000000000 ) ;
#952 = CARTESIAN_POINT ( 'NONE',  ( -62.97617850287781494, -4.279621169095772615, 12.49999999999999822 ) ) ;
#953 = VERTEX_POINT ( 'NONE', #16261 ) ;
#954 = AXIS2_PLACEMENT_3D ( 'NONE', #30315, #18885, #12300 ) ;
#955 = AXIS2_PLACEMENT_3D ( 'NONE', #4511, #24395, #36023 ) ;
#956 = CIRCLE ( 'NONE', #34476, 2.000000000000000000 ) ;
#957 = DIRECTION ( 'NONE',  ( 0.000000000000000000, 0.000000000000000000, 1.000000000000000000 ) ) ;
#958 = VECTOR ( 'NONE', #35917, 1000.000000000000000 ) ;
#959 = CARTESIAN_POINT ( 'NONE',  ( -3.374631327851540519E-06, 86.60254037844397601, -5.000000000000000000 ) ) ;
#960 = AXIS2_PLACEMENT_3D ( 'NONE', #19464, #27895, #25458 ) ;
#961 = CARTESIAN_POINT ( 'NONE',  ( -75.00000337463097821, 8.660254037844374864, 12.50000000000000000 ) ) ;
#962 = ORIENTED_EDGE ( 'NONE', *, *, #11615, .T. ) ;
#963 = EDGE_LOOP ( 'NONE', ( #4579, #25349, #35849, #2137 ) ) ;
#964 = CIRCLE ( 'NONE', #30303, 2.000000000000001776 ) ;
#965 = CIRCLE ( 'NONE', #3965, 2.000000000000001776 ) ;
#966 = DIRECTION ( 'NONE',  ( 1.000000000000000000, 0.000000000000000000, 0.000000000000000000 ) ) ;
#967 = EDGE_LOOP ( 'NONE', ( #28944, #3441 ) ) ;
#968 = CARTESIAN_POINT ( 'NONE',  ( -68.00000337463100664, -17.32050807568882078, 17.49999999999999645 ) ) ;
#969 = CARTESIAN_POINT ( 'NONE',  ( -50.00000337463110611, -69.28203230275519786, -9.999999999999998224 ) ) ;
#970 = CARTESIAN_POINT ( 'NONE',  ( 17.99999662536861678, -69.28203230275519786, -5.000000000000000000 ) ) ;
#971 = CARTESIAN_POINT ( 'NONE',  ( -45.00000000000000000, 0.000000000000000000, -15.00000000000000000 ) ) ;
#972 = CYLINDRICAL_SURFACE ( 'NONE', #26727, 2.000000000000001776 ) ;
#973 = ORIENTED_EDGE ( 'NONE', *, *, #22437, .F. ) ;
#974 = DIRECTION ( 'NONE',  ( 0.000000000000000000, 0.000000000000000000, 1.000000000000000000 ) ) ;
#975 = AXIS2_PLACEMENT_3D ( 'NONE', #823, #1018, #3654 ) ;
#976 = CYLINDRICAL_SURFACE ( 'NONE', #1827, 3.500000000000003109 ) ;
#977 = DIRECTION ( 'NONE',  ( 0.000000000000000000, 0.000000000000000000, 1.000000000000000000 ) ) ;
#978 = ORIENTED_EDGE ( 'NONE', *, *, #16782, .T. ) ;
#979 = FACE_OUTER_BOUND ( 'NONE', #1371, .T. ) ;
#980 = DIRECTION ( 'NONE',  ( 0.000000000000000000, 0.000000000000000000, 1.000000000000000000 ) ) ;
#981 = DIRECTION ( 'NONE',  ( 0.000000000000000000, 0.000000000000000000, 1.000000000000000000 ) ) ;
#982 = AXIS2_PLACEMENT_3D ( 'NONE', #6069, #26123, #12207 ) ;
#983 = AXIS2_PLACEMENT_3D ( 'NONE', #1559, #4573, #18819 ) ;
#984 = CIRCLE ( 'NONE', #23122, 2.000000000000001776 ) ;
#985 = VERTEX_POINT ( 'NONE', #2388 ) ;
#986 = AXIS2_PLACEMENT_3D ( 'NONE', #19892, #19180, #30599 ) ;
#987 = ORIENTED_EDGE ( 'NONE', *, *, #34811, .T. ) ;
#988 = CIRCLE ( 'NONE', #389, 2.000000000000001776 ) ;
#989 = CARTESIAN_POINT ( 'NONE',  ( -50.00000337463112032, -51.96152422706641971, -5.000000000000000000 ) ) ;
#990 = CARTESIAN_POINT ( 'NONE',  ( 49.99999662536846756, 51.96152422706637708, -9.999999999999998224 ) ) ;
#991 = DIRECTION ( 'NONE',  ( 0.000000000000000000, 0.000000000000000000, 1.000000000000000000 ) ) ;
#992 = ORIENTED_EDGE ( 'NONE', *, *, #21226, .F. ) ;
#993 = ORIENTED_EDGE ( 'NONE', *, *, #35591, .T. ) ;
#994 = ORIENTED_EDGE ( 'NONE', *, *, #17122, .F. ) ;
#995 = VECTOR ( 'NONE', #19238, 1000.000000000000000 ) ;
#996 = FACE_OUTER_BOUND ( 'NONE', #23548, .T. ) ;
#997 = EDGE_LOOP ( 'NONE', ( #28170, #14819 ) ) ;
#998 = EDGE_CURVE ( 'NONE', #15802, #18239, #5937, .T. ) ;
#999 = FACE_OUTER_BOUND ( 'NONE', #16357, .T. ) ;
#1000 = VERTEX_POINT ( 'NONE', #25083 ) ;
#1001 = DIRECTION ( 'NONE',  ( -1.000000000000000000, 0.000000000000000000, 0.000000000000000000 ) ) ;
#1002 = EDGE_LOOP ( 'NONE', ( #30017, #31364, #12211, #17517 ) ) ;
#1003 = CIRCLE ( 'NONE', #23764, 2.000000000000001776 ) ;
#1004 = EDGE_LOOP ( 'NONE', ( #26799, #907, #2975, #34427 ) ) ;
#1005 =( NAMED_UNIT ( * ) SI_UNIT ( $, .STERADIAN. ) SOLID_ANGLE_UNIT ( ) );
#1006 = FACE_OUTER_BOUND ( 'NONE', #8509, .T. ) ;
#1007 = CIRCLE ( 'NONE', #6381, 2.000000000000001776 ) ;
#1008 = CARTESIAN_POINT ( 'NONE',  ( 93.55673653615997409, 16.49657687835710362, 12.49999999999999822 ) ) ;
#1009 = ORIENTED_EDGE ( 'NONE', *, *, #1750, .F. ) ;
#1010 = ORIENTED_EDGE ( 'NONE', *, *, #2395, .T. ) ;
#1011 = DIRECTION ( 'NONE',  ( -0.000000000000000000, -0.000000000000000000, 1.000000000000000000 ) ) ;
#1012 = DIRECTION ( 'NONE',  ( -1.000000000000000000, 0.000000000000000000, 0.000000000000000000 ) ) ;
#1013 = VECTOR ( 'NONE', #2939, 1000.000000000000000 ) ;
#1014 = CARTESIAN_POINT ( 'NONE',  ( 21.99999662536862033, -69.28203230275519786, -9.999999999999998224 ) ) ;
#1015 = DIRECTION ( 'NONE',  ( 0.000000000000000000, -0.5000000000000013323, -0.8660254037844379305 ) ) ;
#1016 = AXIS2_PLACEMENT_3D ( 'NONE', #1384, #21079, #21258 ) ;
#1017 = ORIENTED_EDGE ( 'NONE', *, *, #32627, .F. ) ;
#1018 = DIRECTION ( 'NONE',  ( 0.000000000000000000, 0.000000000000000000, 1.000000000000000000 ) ) ;
#1019 = DIRECTION ( 'NONE',  ( 1.000000000000000000, 0.000000000000000000, 0.000000000000000000 ) ) ;
#1020 = ORIENTED_EDGE ( 'NONE', *, *, #1892, .T. ) ;
#1021 = DIRECTION ( 'NONE',  ( 0.000000000000000000, 0.000000000000000000, 1.000000000000000000 ) ) ;
#1022 = CARTESIAN_POINT ( 'NONE',  ( -53.00000337463106348, 43.30127018922197379, -9.999999999999998224 ) ) ;
#1023 = DIRECTION ( 'NONE',  ( 0.000000000000000000, 0.000000000000000000, 1.000000000000000000 ) ) ;
#1024 = EDGE_CURVE ( 'NONE', #2754, #11413, #27298, .T. ) ;
#1025 = CARTESIAN_POINT ( 'NONE',  ( -48.00000337463110611, -69.28203230275519786, -9.999999999999998224 ) ) ;
#1026 = VECTOR ( 'NONE', #13351, 1000.000000000000000 ) ;
#1027 = CARTESIAN_POINT ( 'NONE',  ( -33.99999999999999289, 103.4105893997321886, -19.99999999999999645 ) ) ;
#1028 = CARTESIAN_POINT ( 'NONE',  ( 9.999996625368655856, -69.28203230275519786, 17.49999999999999645 ) ) ;
#1029 = ORIENTED_EDGE ( 'NONE', *, *, #11490, .T. ) ;
#1030 = CARTESIAN_POINT ( 'NONE',  ( 77.99999662536833966, 17.32050807568879236, -9.999999999999998224 ) ) ;
#1031 = CIRCLE ( 'NONE', #24408, 3.000000000000002665 ) ;
#1032 = CARTESIAN_POINT ( 'NONE',  ( -56.67878100130369035, 27.78182860042797131, -4.999999999999997335 ) ) ;
#1033 = LINE ( 'NONE', #12458, #22337 ) ;
#1034 = CIRCLE ( 'NONE', #21993, 2.000000000000001776 ) ;
#1035 = ORIENTED_EDGE ( 'NONE', *, *, #24175, .F. ) ;
#1036 = ORIENTED_EDGE ( 'NONE', *, *, #15845, .T. ) ;
#1037 = ORIENTED_EDGE ( 'NONE', *, *, #29724, .T. ) ;
#1038 = CIRCLE ( 'NONE', #14201, 2.000000000000001776 ) ;
#1039 = FACE_OUTER_BOUND ( 'NONE', #15280, .T. ) ;
#1040 = CARTESIAN_POINT ( 'NONE',  ( 0.000000000000000000, 55.00000000000000000, -15.00000000000000000 ) ) ;
#1041 = CARTESIAN_POINT ( 'NONE',  ( -23.00000337463121980, -77.94228634059963667, -9.999999999999998224 ) ) ;
#1042 = CIRCLE ( 'NONE', #36971, 2.000000000000001776 ) ;
#1043 = AXIS2_PLACEMENT_3D ( 'NONE', #27055, #12989, #4375 ) ;
#1044 = DIRECTION ( 'NONE',  ( 1.000000000000000000, 0.000000000000000000, 0.000000000000000000 ) ) ;
#1045 = CARTESIAN_POINT ( 'NONE',  ( 69.99999662536838230, -34.64101615137759183, 17.49999999999999645 ) ) ;
#1046 = EDGE_LOOP ( 'NONE', ( #22360, #11853, #18757, #7790, #2460, #9786 ) ) ;
#1047 = EDGE_CURVE ( 'NONE', #27815, #5261, #964, .T. ) ;
#1048 = CARTESIAN_POINT ( 'NONE',  ( 44.99999662536851019, 77.94228634059959404, -9.999999999999998224 ) ) ;
#1049 = ORIENTED_EDGE ( 'NONE', *, *, #165, .T. ) ;
#1050 = FACE_BOUND ( 'NONE', #27215, .T. ) ;
#1051 = CIRCLE ( 'NONE', #5850, 2.000000000000001776 ) ;
#1052 = CARTESIAN_POINT ( 'NONE',  ( 66.00000000000000000, 0.000000000000000000, 0.000000000000000000 ) ) ;
#1053 = CIRCLE ( 'NONE', #33994, 95.00000000000001421 ) ;
#1054 = VERTEX_POINT ( 'NONE', #13816 ) ;
#1055 = CARTESIAN_POINT ( 'NONE',  ( -60.93295298010992411, -19.13981058454771755, 12.49999999999999822 ) ) ;
#1056 = CIRCLE ( 'NONE', #24436, 2.000000000000001776 ) ;
#1057 = AXIS2_PLACEMENT_3D ( 'NONE', #1167, #24039, #35484 ) ;
#1058 = DIRECTION ( 'NONE',  ( -0.9788780789851958541, -0.2044448739446721452, 0.000000000000000000 ) ) ;
#1059 = AXIS2_PLACEMENT_3D ( 'NONE', #21546, #35806, #33152 ) ;
#1060 = DIRECTION ( 'NONE',  ( 0.000000000000000000, 0.000000000000000000, 1.000000000000000000 ) ) ;
#1061 = AXIS2_PLACEMENT_3D ( 'NONE', #22379, #8133, #22771 ) ;
#1062 = CARTESIAN_POINT ( 'NONE',  ( 47.63139720814418610, 27.49999999999988987, -10.00000000000000000 ) ) ;
#1063 = CARTESIAN_POINT ( 'NONE',  ( -40.00000337463113453, -69.28203230275519786, -5.000000000000000000 ) ) ;
#1064 = ADVANCED_FACE ( 'NONE', ( #19431 ), #5188, .F. ) ;
#1065 = ORIENTED_EDGE ( 'NONE', *, *, #33685, .T. ) ;
#1066 = CARTESIAN_POINT ( 'NONE',  ( 0.000000000000000000, 0.000000000000000000, -5.000000000000000000 ) ) ;
#1067 = CYLINDRICAL_SURFACE ( 'NONE', #23786, 2.000000000000001776 ) ;
#1068 = FACE_OUTER_BOUND ( 'NONE', #28300, .T. ) ;
#1069 = EDGE_CURVE ( 'NONE', #7812, #13352, #36887, .T. ) ;
#1070 = ORIENTED_EDGE ( 'NONE', *, *, #28796, .T. ) ;
#1071 = CIRCLE ( 'NONE', #5871, 2.000000000000001776 ) ;
#1072 = VERTEX_POINT ( 'NONE', #27856 ) ;
#1073 = ORIENTED_EDGE ( 'NONE', *, *, #23008, .F. ) ;
#1074 = EDGE_CURVE ( 'NONE', #17068, #21597, #33308, .T. ) ;
#1075 = CARTESIAN_POINT ( 'NONE',  ( 0.000000000000000000, 55.00000000000000000, -10.00000000000000178 ) ) ;
#1076 = AXIS2_PLACEMENT_3D ( 'NONE', #7946, #19931, #31356 ) ;
#1077 = CARTESIAN_POINT ( 'NONE',  ( -27.00000337463120914, 77.94228634059957983, -9.999999999999998224 ) ) ;
#1078 = DIRECTION ( 'NONE',  ( 1.000000000000000000, 0.000000000000000000, 0.000000000000000000 ) ) ;
#1079 = EDGE_CURVE ( 'NONE', #21959, #18966, #18933, .T. ) ;
#1080 = AXIS2_PLACEMENT_3D ( 'NONE', #23094, #15030, #8849 ) ;
#1081 = CARTESIAN_POINT ( 'NONE',  ( 70.47608876694671665, 59.13646009116074964, 12.49999999999999822 ) ) ;
#1082 = CARTESIAN_POINT ( 'NONE',  ( 37.50000000000000000, 103.4105893997321743, -19.99999999999999645 ) ) ;
#1083 = AXIS2_PLACEMENT_3D ( 'NONE', #4604, #30814, #13385 ) ;
#1084 = AXIS2_PLACEMENT_3D ( 'NONE', #2463, #36213, #13884 ) ;
#1085 = DIRECTION ( 'NONE',  ( 0.000000000000000000, 0.000000000000000000, 1.000000000000000000 ) ) ;
#1086 = EDGE_LOOP ( 'NONE', ( #35105, #22460, #36309, #3044 ) ) ;
#1087 = AXIS2_PLACEMENT_3D ( 'NONE', #24691, #35407, #10071 ) ;
#1088 = ORIENTED_EDGE ( 'NONE', *, *, #5950, .F. ) ;
#1089 = DIRECTION ( 'NONE',  ( 0.000000000000000000, 0.000000000000000000, 1.000000000000000000 ) ) ;
#1090 = AXIS2_PLACEMENT_3D ( 'NONE', #23449, #35457, #14620 ) ;
#1091 = DIRECTION ( 'NONE',  ( 0.000000000000000000, 0.000000000000000000, -1.000000000000000000 ) ) ;
#1092 = VERTEX_POINT ( 'NONE', #7438 ) ;
#1093 = DIRECTION ( 'NONE',  ( -1.000000000000000000, 0.000000000000000000, 0.000000000000000000 ) ) ;
#1094 = VERTEX_POINT ( 'NONE', #10981 ) ;
#1095 = AXIS2_PLACEMENT_3D ( 'NONE', #24644, #4937, #10373 ) ;
#1096 = ADVANCED_FACE ( 'NONE', ( #4641 ), #16081, .F. ) ;
#1097 = DIRECTION ( 'NONE',  ( 0.000000000000000000, -0.8660254037844420383, -0.4999999999999945599 ) ) ;
#1098 = ORIENTED_EDGE ( 'NONE', *, *, #4957, .T. ) ;
#1099 = ORIENTED_EDGE ( 'NONE', *, *, #3575, .F. ) ;
#1100 = DIRECTION ( 'NONE',  ( 0.000000000000000000, 0.000000000000000000, 1.000000000000000000 ) ) ;
#1101 = ORIENTED_EDGE ( 'NONE', *, *, #5950, .T. ) ;
#1102 = AXIS2_PLACEMENT_3D ( 'NONE', #22107, #13103, #24557 ) ;
#1103 = EDGE_CURVE ( 'NONE', #35240, #21723, #21928, .T. ) ;
#1104 = PRODUCT_DEFINITION_SHAPE ( 'NONE', 'NONE',  #37123 ) ;
#1105 = DIRECTION ( 'NONE',  ( 0.000000000000000000, 0.000000000000000000, 1.000000000000000000 ) ) ;
#1106 = TOROIDAL_SURFACE ( 'NONE', #22662, 4.700000000000000178, 0.2999999999999999889 ) ;
#1107 = CARTESIAN_POINT ( 'NONE',  ( 4.180704885107411783, 3.359771601077109260, -5.801655677627843843 ) ) ;
#1108 = DIRECTION ( 'NONE',  ( 1.000000000000000000, 0.000000000000000000, 0.000000000000000000 ) ) ;
#1109 = EDGE_CURVE ( 'NONE', #15541, #7415, #6337, .T. ) ;
#1110 = VERTEX_POINT ( 'NONE', #16626 ) ;
#1111 = ORIENTED_EDGE ( 'NONE', *, *, #5859, .T. ) ;
#1112 = AXIS2_PLACEMENT_3D ( 'NONE', #7901, #19336, #19521 ) ;
#1113 = ORIENTED_EDGE ( 'NONE', *, *, #12601, .F. ) ;
#1114 = CIRCLE ( 'NONE', #35845, 2.000000000000000000 ) ;
#1115 = ORIENTED_EDGE ( 'NONE', *, *, #14379, .F. ) ;
#1116 = VECTOR ( 'NONE', #33369, 1000.000000000000000 ) ;
#1117 = ORIENTED_EDGE ( 'NONE', *, *, #28870, .T. ) ;
#1118 = DIRECTION ( 'NONE',  ( 1.000000000000000000, 0.000000000000000000, 0.000000000000000000 ) ) ;
#1119 = LINE ( 'NONE', #4305, #27581 ) ;
#1120 = ORIENTED_EDGE ( 'NONE', *, *, #709, .T. ) ;
#1121 = DIRECTION ( 'NONE',  ( -1.000000000000000000, 0.000000000000000000, 0.000000000000000000 ) ) ;
#1122 = CARTESIAN_POINT ( 'NONE',  ( 97.20669606277387231, 67.55917549538906997, 32.49999999999999289 ) ) ;
#1123 = DIRECTION ( 'NONE',  ( 0.000000000000000000, 0.000000000000000000, 1.000000000000000000 ) ) ;
#1124 = CIRCLE ( 'NONE', #13086, 95.00000000000001421 ) ;
#1125 = VERTEX_POINT ( 'NONE', #36130 ) ;
#1126 = CARTESIAN_POINT ( 'NONE',  ( 5.000000000000000888, -2.886751345948134873, -2.080000000000000071 ) ) ;
#1127 = AXIS2_PLACEMENT_3D ( 'NONE', #25556, #11105, #22757 ) ;
#1128 = CARTESIAN_POINT ( 'NONE',  ( 2.999996625368645198, 77.94228634059957983, 12.50000000000000000 ) ) ;
#1129 = EDGE_CURVE ( 'NONE', #35481, #15444, #20708, .T. ) ;
#1130 = DIRECTION ( 'NONE',  ( 0.000000000000000000, 0.000000000000000000, 1.000000000000000000 ) ) ;
#1131 = ORIENTED_EDGE ( 'NONE', *, *, #27826, .T. ) ;
#1132 = DIRECTION ( 'NONE',  ( 0.000000000000000000, 0.000000000000000000, 1.000000000000000000 ) ) ;
#1133 = CARTESIAN_POINT ( 'NONE',  ( 21.99999662536859191, 69.28203230275516944, -9.999999999999998224 ) ) ;
#1134 = ORIENTED_EDGE ( 'NONE', *, *, #35531, .T. ) ;
#1135 = VERTEX_POINT ( 'NONE', #28239 ) ;
#1136 = CARTESIAN_POINT ( 'NONE',  ( 4.467624384280048488, 0.000000000000000000, 0.000000000000000000 ) ) ;
#1137 = VECTOR ( 'NONE', #19117, 1000.000000000000000 ) ;
#1138 = LINE ( 'NONE', #32821, #11547 ) ;
#1139 = DIRECTION ( 'NONE',  ( 0.000000000000000000, 0.000000000000000000, 1.000000000000000000 ) ) ;
#1140 = ORIENTED_EDGE ( 'NONE', *, *, #5610, .F. ) ;
#1141 = CIRCLE ( 'NONE', #14312, 2.000000000000001776 ) ;
#1142 = DIRECTION ( 'NONE',  ( 0.000000000000000000, 0.000000000000000000, 1.000000000000000000 ) ) ;
#1143 = DIRECTION ( 'NONE',  ( 1.000000000000000000, 0.000000000000000000, 0.000000000000000000 ) ) ;
#1144 = ADVANCED_FACE ( 'NONE', ( #2556 ), #28058, .F. ) ;
#1145 = ORIENTED_EDGE ( 'NONE', *, *, #27137, .T. ) ;
#1146 = AXIS2_PLACEMENT_3D ( 'NONE', #33482, #1791, #19048 ) ;
#1147 = EDGE_CURVE ( 'NONE', #8445, #4612, #10257, .T. ) ;
#1148 = LINE ( 'NONE', #15588, #32767 ) ;
#1149 = ORIENTED_EDGE ( 'NONE', *, *, #2072, .F. ) ;
#1150 = AXIS2_PLACEMENT_3D ( 'NONE', #16145, #35836, #30371 ) ;
#1151 = DIRECTION ( 'NONE',  ( 1.000000000000000000, 0.000000000000000000, 0.000000000000000000 ) ) ;
#1152 = EDGE_CURVE ( 'NONE', #3514, #5093, #3808, .T. ) ;
#1153 = DIRECTION ( 'NONE',  ( -0.000000000000000000, -0.000000000000000000, 1.000000000000000000 ) ) ;
#1154 = AXIS2_PLACEMENT_3D ( 'NONE', #29769, #23981, #32780 ) ;
#1155 = DIRECTION ( 'NONE',  ( 1.000000000000000000, 0.000000000000000000, 0.000000000000000000 ) ) ;
#1156 = EDGE_CURVE ( 'NONE', #30650, #21828, #6105, .T. ) ;
#1157 = ORIENTED_EDGE ( 'NONE', *, *, #34773, .T. ) ;
#1158 = AXIS2_PLACEMENT_3D ( 'NONE', #18655, #15470, #18473 ) ;
#1159 = ORIENTED_EDGE ( 'NONE', *, *, #12376, .F. ) ;
#1160 = ADVANCED_FACE ( 'NONE', ( #104 ), #36862, .F. ) ;
#1161 = ADVANCED_FACE ( 'NONE', ( #2940 ), #9094, .F. ) ;
#1162 = AXIS2_PLACEMENT_3D ( 'NONE', #27745, #7331, #35846 ) ;
#1163 = EDGE_LOOP ( 'NONE', ( #23509, #19777, #32309, #19486, #17635 ) ) ;
#1164 = CARTESIAN_POINT ( 'NONE',  ( 4.242640687119292764, 4.242640687119187071, 27.50000000000000000 ) ) ;
#1165 = VECTOR ( 'NONE', #23204, 1000.000000000000000 ) ;
#1166 = CARTESIAN_POINT ( 'NONE',  ( 0.000000000000000000, 0.000000000000000000, -6.000000000000000000 ) ) ;
#1167 = CARTESIAN_POINT ( 'NONE',  ( 64.99999662536841072, -25.98076211353320275, 17.49999999999999645 ) ) ;
#1168 = CARTESIAN_POINT ( 'NONE',  ( -73.00000337463097821, -8.660254037844422825, -5.000000000000000000 ) ) ;
#1169 = CARTESIAN_POINT ( 'NONE',  ( -8.000003374631249997, -86.60254037844400443, -9.999999999999998224 ) ) ;
#1170 = EDGE_CURVE ( 'NONE', #9726, #1919, #14589, .T. ) ;
#1171 = ORIENTED_EDGE ( 'NONE', *, *, #26583, .T. ) ;
#1172 = DIRECTION ( 'NONE',  ( 0.000000000000000000, 0.000000000000000000, -1.000000000000000000 ) ) ;
#1173 = EDGE_CURVE ( 'NONE', #17720, #12612, #31236, .T. ) ;
#1174 = DIRECTION ( 'NONE',  ( 1.000000000000000000, 0.000000000000000000, 0.000000000000000000 ) ) ;
#1175 = EDGE_CURVE ( 'NONE', #30254, #25902, #5739, .T. ) ;
#1176 = LINE ( 'NONE', #20856, #10978 ) ;
#1177 = ORIENTED_EDGE ( 'NONE', *, *, #12201, .T. ) ;
#1178 = CARTESIAN_POINT ( 'NONE',  ( -34.00000000000027711, -58.88972745734168512, -4.999999999999997335 ) ) ;
#1179 = DIRECTION ( 'NONE',  ( 1.000000000000000000, 0.000000000000000000, 0.000000000000000000 ) ) ;
#1180 = DIRECTION ( 'NONE',  ( -0.000000000000000000, -0.000000000000000000, 1.000000000000000000 ) ) ;
#1181 = AXIS2_PLACEMENT_3D ( 'NONE', #26923, #11728, #23741 ) ;
#1182 = EDGE_LOOP ( 'NONE', ( #19164, #37024 ) ) ;
#1183 = ORIENTED_EDGE ( 'NONE', *, *, #215, .F. ) ;
#1184 = DIRECTION ( 'NONE',  ( 1.000000000000000000, 0.000000000000000000, 0.000000000000000000 ) ) ;
#1185 = CARTESIAN_POINT ( 'NONE',  ( 69.99999662536839651, 34.64101615137758472, 12.50000000000000000 ) ) ;
#1186 = CARTESIAN_POINT ( 'NONE',  ( -53.00000337463109190, -60.62177826491083010, -9.999999999999998224 ) ) ;
#1187 = ORIENTED_EDGE ( 'NONE', *, *, #32304, .F. ) ;
#1188 = EDGE_LOOP ( 'NONE', ( #33444, #30548, #5664, #10870 ) ) ;
#1189 = AXIS2_PLACEMENT_3D ( 'NONE', #28308, #7717, #13883 ) ;
#1190 = ORIENTED_EDGE ( 'NONE', *, *, #24796, .T. ) ;
#1191 = CARTESIAN_POINT ( 'NONE',  ( -50.00000337463109190, 69.28203230275518365, -9.999999999999998224 ) ) ;
#1192 = EDGE_CURVE ( 'NONE', #12047, #25810, #10398, .T. ) ;
#1193 = ORIENTED_EDGE ( 'NONE', *, *, #196, .T. ) ;
#1194 = ADVANCED_FACE ( 'NONE', ( #37063 ), #17719, .F. ) ;
#1195 = VERTEX_POINT ( 'NONE', #20169 ) ;
#1196 = CYLINDRICAL_SURFACE ( 'NONE', #14748, 3.500000000000003109 ) ;
#1197 = ORIENTED_EDGE ( 'NONE', *, *, #18865, .T. ) ;
#1198 = ORIENTED_EDGE ( 'NONE', *, *, #21038, .T. ) ;
#1199 = DIRECTION ( 'NONE',  ( 0.000000000000000000, 0.000000000000000000, 1.000000000000000000 ) ) ;
#1200 = DIRECTION ( 'NONE',  ( -0.000000000000000000, -0.000000000000000000, 1.000000000000000000 ) ) ;
#1201 = ORIENTED_EDGE ( 'NONE', *, *, #3906, .T. ) ;
#1202 = ORIENTED_EDGE ( 'NONE', *, *, #22250, .T. ) ;
#1203 = EDGE_CURVE ( 'NONE', #14529, #21657, #26559, .T. ) ;
#1204 = CARTESIAN_POINT ( 'NONE',  ( 3.000000000000000000, 0.000000000000000000, -6.000000000000001776 ) ) ;
#1205 = DIRECTION ( 'NONE',  ( 1.000000000000000000, 0.000000000000000000, 0.000000000000000000 ) ) ;
#1206 = CIRCLE ( 'NONE', #22169, 0.5671001622691687061 ) ;
#1207 = CYLINDRICAL_SURFACE ( 'NONE', #4899, 95.00000000000000000 ) ;
#1208 = CARTESIAN_POINT ( 'NONE',  ( -4.999999999999538147, 1.069480574179262788, -3.973098401497047405 ) ) ;
#1209 = ORIENTED_EDGE ( 'NONE', *, *, #23387, .T. ) ;
#1210 = CARTESIAN_POINT ( 'NONE',  ( -23.00000337463120559, 77.94228634059957983, -5.000000000000000000 ) ) ;
#1211 = ORIENTED_EDGE ( 'NONE', *, *, #22703, .F. ) ;
#1212 = AXIS2_PLACEMENT_3D ( 'NONE', #6059, #25767, #35115 ) ;
#1213 = DIRECTION ( 'NONE',  ( 0.000000000000000000, 0.000000000000000000, -1.000000000000000000 ) ) ;
#1214 = CARTESIAN_POINT ( 'NONE',  ( -4.242640687119273224, -4.242640687119226151, 32.50000000000000000 ) ) ;
#1215 = VECTOR ( 'NONE', #21555, 1000.000000000000000 ) ;
#1216 = CYLINDRICAL_SURFACE ( 'NONE', #1016, 2.000000000000001776 ) ;
#1217 = EDGE_CURVE ( 'NONE', #24448, #33082, #4139, .T. ) ;
#1218 = DIRECTION ( 'NONE',  ( 0.000000000000000000, 0.000000000000000000, 1.000000000000000000 ) ) ;
#1219 = EDGE_CURVE ( 'NONE', #26696, #14320, #21772, .T. ) ;
#1220 = CARTESIAN_POINT ( 'NONE',  ( 69.99999662536839651, -17.32050807568879947, -9.999999999999998224 ) ) ;
#1221 = EDGE_CURVE ( 'NONE', #29589, #29318, #16985, .T. ) ;
#1222 = EDGE_CURVE ( 'NONE', #29771, #34151, #3222, .T. ) ;
#1223 = DIRECTION ( 'NONE',  ( -1.000000000000000000, 0.000000000000000000, 0.000000000000000000 ) ) ;
#1224 = VERTEX_POINT ( 'NONE', #20518 ) ;
#1225 = DIRECTION ( 'NONE',  ( 0.000000000000000000, 0.000000000000000000, 1.000000000000000000 ) ) ;
#1226 = DIRECTION ( 'NONE',  ( 0.8660254037844344888, -0.5000000000000069944, 0.000000000000000000 ) ) ;
#1227 = CARTESIAN_POINT ( 'NONE',  ( 82.99999662536831124, -25.98076211353319565, -5.000000000000000000 ) ) ;
#1228 = ORIENTED_EDGE ( 'NONE', *, *, #33762, .F. ) ;
#1229 = ORIENTED_EDGE ( 'NONE', *, *, #4111, .F. ) ;
#1230 = ORIENTED_EDGE ( 'NONE', *, *, #7457, .F. ) ;
#1231 = DIRECTION ( 'NONE',  ( -1.000000000000000000, 0.000000000000000000, 0.000000000000000000 ) ) ;
#1232 = CARTESIAN_POINT ( 'NONE',  ( -31.74999999999995737, 0.000000000000000000, 0.000000000000000000 ) ) ;
#1233 = DIRECTION ( 'NONE',  ( 1.000000000000000000, 0.000000000000000000, 0.000000000000000000 ) ) ;
#1234 = AXIS2_PLACEMENT_3D ( 'NONE', #35121, #9785, #9429 ) ;
#1235 = DIRECTION ( 'NONE',  ( 1.000000000000000000, 0.000000000000000000, 0.000000000000000000 ) ) ;
#1236 = FACE_OUTER_BOUND ( 'NONE', #31327, .T. ) ;
#1237 = CARTESIAN_POINT ( 'NONE',  ( -75.00000337463097821, 43.30127018922197379, 17.49999999999999645 ) ) ;
#1238 = ORIENTED_EDGE ( 'NONE', *, *, #28621, .T. ) ;
#1239 = FACE_OUTER_BOUND ( 'NONE', #35151, .T. ) ;
#1240 = ORIENTED_EDGE ( 'NONE', *, *, #2218, .T. ) ;
#1241 = FACE_BOUND ( 'NONE', #25011, .T. ) ;
#1242 = EDGE_CURVE ( 'NONE', #8606, #35191, #24182, .T. ) ;
#1243 = DIRECTION ( 'NONE',  ( -0.000000000000000000, -0.000000000000000000, 1.000000000000000000 ) ) ;
#1244 = FACE_BOUND ( 'NONE', #25604, .T. ) ;
#1245 = SURFACE_STYLE_USAGE ( .BOTH. , #13045 ) ;
#1246 = EDGE_LOOP ( 'NONE', ( #23678, #30155, #171, #5798 ) ) ;
#1247 = DIRECTION ( 'NONE',  ( -0.000000000000000000, -0.000000000000000000, 1.000000000000000000 ) ) ;
#1248 = ITEM_DEFINED_TRANSFORMATION ( 'NONE', 'NONE', #1599,  #21385 ) ;
#1249 = DIRECTION ( 'NONE',  ( 0.000000000000000000, 0.000000000000000000, 1.000000000000000000 ) ) ;
#1250 = DIRECTION ( 'NONE',  ( -1.000000000000000000, 0.000000000000000000, 0.000000000000000000 ) ) ;
#1251 = DIRECTION ( 'NONE',  ( 1.000000000000000000, 0.000000000000000000, 0.000000000000000000 ) ) ;
#1252 = ORIENTED_EDGE ( 'NONE', *, *, #7122, .T. ) ;
#1253 = DIRECTION ( 'NONE',  ( 0.000000000000000000, 0.000000000000000000, 1.000000000000000000 ) ) ;
#1254 = CARTESIAN_POINT ( 'NONE',  ( 54.99999662536844625, 60.62177826491077326, -9.999999999999998224 ) ) ;
#1255 = DIRECTION ( 'NONE',  ( 0.000000000000000000, 0.000000000000000000, 1.000000000000000000 ) ) ;
#1256 = ORIENTED_EDGE ( 'NONE', *, *, #13954, .F. ) ;
#1257 = ORIENTED_EDGE ( 'NONE', *, *, #6342, .T. ) ;
#1258 = AXIS2_PLACEMENT_3D ( 'NONE', #15742, #21175, #12552 ) ;
#1259 = EDGE_CURVE ( 'NONE', #36782, #30643, #4413, .T. ) ;
#1260 = ORIENTED_EDGE ( 'NONE', *, *, #23433, .T. ) ;
#1261 = DIRECTION ( 'NONE',  ( 1.000000000000000000, 0.000000000000000000, 0.000000000000000000 ) ) ;
#1262 = CARTESIAN_POINT ( 'NONE',  ( 0.000000000000000000, 95.00000000000001421, 32.50000000000000000 ) ) ;
#1263 = DIRECTION ( 'NONE',  ( -1.000000000000000000, 0.000000000000000000, 0.000000000000000000 ) ) ;
#1264 = CARTESIAN_POINT ( 'NONE',  ( 0.000000000000000000, 0.000000000000000000, -5.000000000000000000 ) ) ;
#1265 = CARTESIAN_POINT ( 'NONE',  ( 59.99999662536842493, -51.96152422706639840, -5.000000000000000000 ) ) ;
#1266 = APPLICATION_CONTEXT ( 'automotive_design' ) ;
#1267 = FACE_OUTER_BOUND ( 'NONE', #16876, .T. ) ;
#1268 = EDGE_LOOP ( 'NONE', ( #35515, #24367, #17572, #340 ) ) ;
#1269 = ORIENTED_EDGE ( 'NONE', *, *, #404, .F. ) ;
#1270 = DIRECTION ( 'NONE',  ( 0.000000000000000000, 0.000000000000000000, 1.000000000000000000 ) ) ;
#1271 = CARTESIAN_POINT ( 'NONE',  ( -56.29165124598871017, -32.49999999999966604, 12.49999999999999822 ) ) ;
#1272 = EDGE_LOOP ( 'NONE', ( #23070, #25854, #7139 ) ) ;
#1273 = DIRECTION ( 'NONE',  ( 1.000000000000000000, 0.000000000000000000, 0.000000000000000000 ) ) ;
#1274 = ORIENTED_EDGE ( 'NONE', *, *, #34814, .F. ) ;
#1275 = AXIS2_PLACEMENT_3D ( 'NONE', #35835, #10142, #4887 ) ;
#1276 = CARTESIAN_POINT ( 'NONE',  ( 4.279621169095998212, -62.97617850287780072, -4.999999999999997335 ) ) ;
#1277 = EDGE_CURVE ( 'NONE', #32298, #9210, #18783, .T. ) ;
#1278 = CARTESIAN_POINT ( 'NONE',  ( 49.99999662536846756, -69.28203230275519786, 12.50000000000000000 ) ) ;
#1279 = ORIENTED_EDGE ( 'NONE', *, *, #8302, .F. ) ;
#1280 = ORIENTED_EDGE ( 'NONE', *, *, #25146, .F. ) ;
#1281 = EDGE_CURVE ( 'NONE', #28577, #28380, #32553, .T. ) ;
#1282 = DIRECTION ( 'NONE',  ( 1.000000000000000000, 0.000000000000000000, 0.000000000000000000 ) ) ;
#1283 = ORIENTED_EDGE ( 'NONE', *, *, #14933, .F. ) ;
#1284 = SHAPE_REPRESENTATION_RELATIONSHIP ( 'NONE' , 'NONE' ,  #22738, #4968 ) ;
#1285 = CARTESIAN_POINT ( 'NONE',  ( -5.000000000000000888, 2.886751345948107783, -0.5999999999999836575 ) ) ;
#1286 = ADVANCED_FACE ( 'NONE', ( #10030 ), #17919, .T. ) ;
#1287 = DIRECTION ( 'NONE',  ( -1.000000000000000000, 0.000000000000000000, 0.000000000000000000 ) ) ;
#1288 = DIRECTION ( 'NONE',  ( 0.000000000000000000, 0.000000000000000000, 1.000000000000000000 ) ) ;
#1289 = ORIENTED_EDGE ( 'NONE', *, *, #35342, .F. ) ;
#1290 = ORIENTED_EDGE ( 'NONE', *, *, #13014, .F. ) ;
#1291 = ORIENTED_EDGE ( 'NONE', *, *, #35469, .T. ) ;
#1292 = ORIENTED_EDGE ( 'NONE', *, *, #28666, .T. ) ;
#1293 = CARTESIAN_POINT ( 'NONE',  ( 51.68138994340220904, 113.8157894736842053, 27.50000000000000000 ) ) ;
#1294 = AXIS2_PLACEMENT_3D ( 'NONE', #11887, #20153, #8708 ) ;
#1295 = EDGE_CURVE ( 'NONE', #4453, #33934, #25980, .T. ) ;
#1296 = LINE ( 'NONE', #9915, #16803 ) ;
#1297 = EDGE_LOOP ( 'NONE', ( #315, #8437, #30494, #23979 ) ) ;
#1298 = VECTOR ( 'NONE', #940, 1000.000000000000000 ) ;
#1299 = CARTESIAN_POINT ( 'NONE',  ( -56.56139351304917540, -61.87160258682602176, 12.50000000000000000 ) ) ;
#1300 = DIRECTION ( 'NONE',  ( 1.000000000000000000, 0.000000000000000000, 0.000000000000000000 ) ) ;
#1301 = CARTESIAN_POINT ( 'NONE',  ( -80.00000337463094979, 34.64101615137757051, -9.999999999999998224 ) ) ;
#1302 = ORIENTED_EDGE ( 'NONE', *, *, #17801, .T. ) ;
#1303 = CARTESIAN_POINT ( 'NONE',  ( 69.99999662536841072, 51.96152422706640550, -9.999999999999998224 ) ) ;
#1304 = CARTESIAN_POINT ( 'NONE',  ( 26.97173338359068850, -77.60724282659606388, 12.50000000000000000 ) ) ;
#1305 = DIRECTION ( 'NONE',  ( 0.000000000000000000, 0.000000000000000000, 1.000000000000000000 ) ) ;
#1306 = ORIENTED_EDGE ( 'NONE', *, *, #5534, .F. ) ;
#1307 = CARTESIAN_POINT ( 'NONE',  ( 101.4252494179806661, -31.43181965332042438, 32.50001250000000397 ) ) ;
#1308 = CARTESIAN_POINT ( 'NONE',  ( -37.50000000000000000, 103.4105893997321743, 32.50000000000000000 ) ) ;
#1309 = ORIENTED_EDGE ( 'NONE', *, *, #28870, .F. ) ;
#1310 = EDGE_CURVE ( 'NONE', #14745, #34871, #16401, .T. ) ;
#1311 = ORIENTED_EDGE ( 'NONE', *, *, #7418, .T. ) ;
#1312 = DIRECTION ( 'NONE',  ( 0.000000000000000000, 0.000000000000000000, 1.000000000000000000 ) ) ;
#1313 = EDGE_CURVE ( 'NONE', #11967, #18936, #28347, .T. ) ;
#1314 = CARTESIAN_POINT ( 'NONE',  ( -68.19171733629717380, 52.81598405851951838, -5.000000000000000000 ) ) ;
#1315 = DIRECTION ( 'NONE',  ( -0.000000000000000000, -0.000000000000000000, 1.000000000000000000 ) ) ;
#1316 = DIRECTION ( 'NONE',  ( 1.000000000000000000, 0.000000000000000000, 0.000000000000000000 ) ) ;
#1317 = EDGE_LOOP ( 'NONE', ( #22354, #5648 ) ) ;
#1318 = UNCERTAINTY_MEASURE_WITH_UNIT (LENGTH_MEASURE( 1.000000000000000082E-05 ), #23595, 'distance_accuracy_value', 'NONE');
#1319 = EDGE_CURVE ( 'NONE', #11639, #9216, #27762, .T. ) ;
#1320 = CARTESIAN_POINT ( 'NONE',  ( 56.67878100130369035, -27.78182860042797131, -4.999999999999997335 ) ) ;
#1321 = DIRECTION ( 'NONE',  ( 1.000000000000000000, 0.000000000000000000, 0.000000000000000000 ) ) ;
#1322 = ORIENTED_EDGE ( 'NONE', *, *, #27528, .T. ) ;
#1323 = AXIS2_PLACEMENT_3D ( 'NONE', #777, #20467, #6773 ) ;
#1324 = ADVANCED_FACE ( 'NONE', ( #29903 ), #23727, .F. ) ;
#1325 = CARTESIAN_POINT ( 'NONE',  ( 71.99999662536841072, 51.96152422706640550, -9.999999999999998224 ) ) ;
#1326 = ORIENTED_EDGE ( 'NONE', *, *, #5342, .F. ) ;
#1327 = PLANE ( 'NONE',  #4339 ) ;
#1328 = LINE ( 'NONE', #27392, #230 ) ;
#1329 = ADVANCED_FACE ( 'NONE', ( #32145 ), #4233, .F. ) ;
#1330 = DIRECTION ( 'NONE',  ( 1.000000000000000000, 0.000000000000000000, 0.000000000000000000 ) ) ;
#1331 = ORIENTED_EDGE ( 'NONE', *, *, #33702, .F. ) ;
#1332 = EDGE_LOOP ( 'NONE', ( #26969, #10374, #12947, #269 ) ) ;
#1333 = VECTOR ( 'NONE', #12576, 1000.000000000000000 ) ;
#1334 = VECTOR ( 'NONE', #7184, 1000.000000000000000 ) ;
#1335 = EDGE_LOOP ( 'NONE', ( #28851, #36850, #26335, #27471 ) ) ;
#1336 = CARTESIAN_POINT ( 'NONE',  ( -35.00000337463116296, -60.62177826491080168, 17.49999999999999645 ) ) ;
#1337 = CARTESIAN_POINT ( 'NONE',  ( 0.000000000000000000, 0.000000000000000000, -10.00000000000000000 ) ) ;
#1338 = CARTESIAN_POINT ( 'NONE',  ( -75.00000337463097821, 8.660254037844374864, -9.999999999999998224 ) ) ;
#1339 = CARTESIAN_POINT ( 'NONE',  ( -53.00000337463109190, -60.62177826491083010, -9.999999999999998224 ) ) ;
#1340 = CARTESIAN_POINT ( 'NONE',  ( -3.374631327851540519E-06, 86.60254037844397601, -9.999999999999998224 ) ) ;
#1341 = EDGE_LOOP ( 'NONE', ( #33053, #4985, #34509, #5482 ) ) ;
#1342 = CARTESIAN_POINT ( 'NONE',  ( 0.000000000000000000, 0.000000000000000000, -10.00000000000000000 ) ) ;
#1343 = ADVANCED_FACE ( 'NONE', ( #20710 ), #12251, .F. ) ;
#1344 = DIRECTION ( 'NONE',  ( 0.8660254037844415942, 0.4999999999999949485, 0.000000000000000000 ) ) ;
#1345 = CIRCLE ( 'NONE', #5555, 5.000000000000000000 ) ;
#1346 = FACE_OUTER_BOUND ( 'NONE', #19597, .T. ) ;
#1347 = ORIENTED_EDGE ( 'NONE', *, *, #9423, .F. ) ;
#1348 = CARTESIAN_POINT ( 'NONE',  ( -30.99999999999944933, 58.88972745734214698, -4.999999999999997335 ) ) ;
#1349 = CARTESIAN_POINT ( 'NONE',  ( -60.00000337463107059, -34.64101615137762025, 17.49999999999999645 ) ) ;
#1350 = ORIENTED_EDGE ( 'NONE', *, *, #33790, .T. ) ;
#1351 = ADVANCED_FACE ( 'NONE', ( #35723 ), #29348, .F. ) ;
#1352 = ORIENTED_EDGE ( 'NONE', *, *, #28011, .F. ) ;
#1353 = EDGE_CURVE ( 'NONE', #7436, #25823, #3667, .T. ) ;
#1354 = CARTESIAN_POINT ( 'NONE',  ( -65.00000337463104927, -43.30127018922202353, 17.49999999999999645 ) ) ;
#1355 = DIRECTION ( 'NONE',  ( -0.000000000000000000, -0.000000000000000000, -1.000000000000000000 ) ) ;
#1356 = DIRECTION ( 'NONE',  ( 1.000000000000000000, 0.000000000000000000, 0.000000000000000000 ) ) ;
#1357 = ORIENTED_EDGE ( 'NONE', *, *, #14392, .T. ) ;
#1358 = VERTEX_POINT ( 'NONE', #15276 ) ;
#1359 = EDGE_LOOP ( 'NONE', ( #6598, #23396 ) ) ;
#1360 = CARTESIAN_POINT ( 'NONE',  ( 74.99999662536836809, -8.660254037844401509, -9.999999999999998224 ) ) ;
#1361 = AXIS2_PLACEMENT_3D ( 'NONE', #16489, #36922, #30568 ) ;
#1362 = VERTEX_POINT ( 'NONE', #9664 ) ;
#1363 = ORIENTED_EDGE ( 'NONE', *, *, #19027, .T. ) ;
#1364 = DIRECTION ( 'NONE',  ( 0.000000000000000000, 0.000000000000000000, -1.000000000000000000 ) ) ;
#1365 = ORIENTED_EDGE ( 'NONE', *, *, #257, .T. ) ;
#1366 = ORIENTED_EDGE ( 'NONE', *, *, #25560, .T. ) ;
#1367 = CARTESIAN_POINT ( 'NONE',  ( -3.108944973436880588, -78.59336093177338967, 12.50000000000000000 ) ) ;
#1368 = EDGE_CURVE ( 'NONE', #28369, #25631, #212, .T. ) ;
#1369 = VECTOR ( 'NONE', #22116, 1000.000000000000000 ) ;
#1370 = CARTESIAN_POINT ( 'NONE',  ( 57.99999662536843914, -34.64101615137759893, -9.999999999999998224 ) ) ;
#1371 = EDGE_LOOP ( 'NONE', ( #18126, #16442, #17587, #13499, #32265 ) ) ;
#1372 = CIRCLE ( 'NONE', #19925, 2.000000000000001776 ) ;
#1373 = VERTEX_POINT ( 'NONE', #20919 ) ;
#1374 = LINE ( 'NONE', #29677, #35867 ) ;
#1375 = CARTESIAN_POINT ( 'NONE',  ( 4.999999999999999112, 2.886751345948125991, -3.984345921091767551 ) ) ;
#1376 = FACE_OUTER_BOUND ( 'NONE', #29442, .T. ) ;
#1377 = LINE ( 'NONE', #23349, #6509 ) ;
#1378 = ORIENTED_EDGE ( 'NONE', *, *, #31, .F. ) ;
#1379 = DIRECTION ( 'NONE',  ( 0.000000000000000000, 0.000000000000000000, 1.000000000000000000 ) ) ;
#1380 = ORIENTED_EDGE ( 'NONE', *, *, #29534, .T. ) ;
#1381 = CARTESIAN_POINT ( 'NONE',  ( 124.4080600076931375, 12.15049814296589226, 32.50000000000000000 ) ) ;
#1382 = CYLINDRICAL_SURFACE ( 'NONE', #34584, 2.000000000000001776 ) ;
#1383 = CIRCLE ( 'NONE', #21752, 4.999999999999997335 ) ;
#1384 = CARTESIAN_POINT ( 'NONE',  ( 64.99999662536841072, -25.98076211353320275, -9.999999999999998224 ) ) ;
#1385 = CARTESIAN_POINT ( 'NONE',  ( -85.00000337463092137, -8.660254037844422825, -9.999999999999998224 ) ) ;
#1386 = DIRECTION ( 'NONE',  ( 0.000000000000000000, 0.000000000000000000, 1.000000000000000000 ) ) ;
#1387 = EDGE_CURVE ( 'NONE', #4724, #15870, #6159, .T. ) ;
#1388 = DIRECTION ( 'NONE',  ( -1.000000000000000000, 0.000000000000000000, 0.000000000000000000 ) ) ;
#1389 = CARTESIAN_POINT ( 'NONE',  ( 5.000000000000000000, 2.059541880722000506, -1.329159518034687126 ) ) ;
#1390 = ORIENTED_EDGE ( 'NONE', *, *, #19478, .F. ) ;
#1391 = EDGE_CURVE ( 'NONE', #4682, #26755, #18090, .T. ) ;
#1392 = DIRECTION ( 'NONE',  ( 0.000000000000000000, 0.000000000000000000, -1.000000000000000000 ) ) ;
#1393 = CARTESIAN_POINT ( 'NONE',  ( 74.99999662536836809, 25.98076211353319565, -9.999999999999998224 ) ) ;
#1394 = DIRECTION ( 'NONE',  ( 0.000000000000000000, 0.000000000000000000, 1.000000000000000000 ) ) ;
#1395 = VERTEX_POINT ( 'NONE', #24094 ) ;
#1396 = EDGE_CURVE ( 'NONE', #24986, #6951, #24134, .T. ) ;
#1397 = EDGE_LOOP ( 'NONE', ( #635, #19656 ) ) ;
#1398 = ORIENTED_EDGE ( 'NONE', *, *, #1368, .F. ) ;
#1399 = AXIS2_PLACEMENT_3D ( 'NONE', #7948, #21648, #16029 ) ;
#1400 = DIRECTION ( 'NONE',  ( -0.000000000000000000, -0.000000000000000000, 1.000000000000000000 ) ) ;
#1401 = CARTESIAN_POINT ( 'NONE',  ( 57.99999662536842493, 51.96152422706639129, -5.000000000000000000 ) ) ;
#1402 = FACE_OUTER_BOUND ( 'NONE', #32272, .T. ) ;
#1403 = EDGE_CURVE ( 'NONE', #8057, #11432, #1033, .T. ) ;
#1404 = ORIENTED_EDGE ( 'NONE', *, *, #31414, .F. ) ;
#1405 = EDGE_CURVE ( 'NONE', #5493, #24286, #18269, .T. ) ;
#1406 = CARTESIAN_POINT ( 'NONE',  ( -2.000003374631289521, -69.28203230275519786, -5.000000000000000000 ) ) ;
#1407 = DIRECTION ( 'NONE',  ( 0.000000000000000000, 0.000000000000000000, 1.000000000000000000 ) ) ;
#1408 = ORIENTED_EDGE ( 'NONE', *, *, #15156, .T. ) ;
#1409 = DIRECTION ( 'NONE',  ( 1.000000000000000000, 0.000000000000000000, 0.000000000000000000 ) ) ;
#1410 = VERTEX_POINT ( 'NONE', #1227 ) ;
#1411 = FACE_BOUND ( 'NONE', #34304, .T. ) ;
#1412 = EDGE_CURVE ( 'NONE', #17343, #8449, #18127, .T. ) ;
#1413 = EDGE_CURVE ( 'NONE', #34844, #26265, #35516, .T. ) ;
#1414 = CIRCLE ( 'NONE', #27771, 2.000000000000001776 ) ;
#1415 = DIRECTION ( 'NONE',  ( 1.000000000000000000, 0.000000000000000000, 0.000000000000000000 ) ) ;
#1416 = CARTESIAN_POINT ( 'NONE',  ( -20.00000337463123756, -69.28203230275522628, -9.999999999999998224 ) ) ;
#1417 = ADVANCED_FACE ( 'NONE', ( #10941 ), #24478, .F. ) ;
#1418 = ADVANCED_FACE ( 'NONE', ( #4952 ), #35918, .F. ) ;
#1419 = PRESENTATION_STYLE_ASSIGNMENT (( #1245 ) ) ;
#1420 = EDGE_LOOP ( 'NONE', ( #24774, #7913, #20426, #34060 ) ) ;
#1421 = CARTESIAN_POINT ( 'NONE',  ( 56.67878100130369035, -27.78182860042797131, -4.999999999999997335 ) ) ;
#1422 = PRODUCT_CONTEXT ( 'NONE', #17085, 'mechanical' ) ;
#1423 = CARTESIAN_POINT ( 'NONE',  ( 42.99999662536850309, -60.62177826491080168, -9.999999999999998224 ) ) ;
#1424 = TOROIDAL_SURFACE ( 'NONE', #7427, 4.700000000000000178, 0.2999999999999999889 ) ;
#1425 = CARTESIAN_POINT ( 'NONE',  ( -4.999999999999999112, 24.49489742783178059, 15.00000000000000000 ) ) ;
#1426 = DIRECTION ( 'NONE',  ( 1.000000000000000000, 0.000000000000000000, 0.000000000000000000 ) ) ;
#1427 = EDGE_LOOP ( 'NONE', ( #9390, #29158 ) ) ;
#1428 = DIRECTION ( 'NONE',  ( 0.000000000000000000, 0.000000000000000000, 1.000000000000000000 ) ) ;
#1429 = DIRECTION ( 'NONE',  ( 0.000000000000000000, 0.000000000000000000, 1.000000000000000000 ) ) ;
#1430 = DIRECTION ( 'NONE',  ( -0.000000000000000000, -0.000000000000000000, 1.000000000000000000 ) ) ;
#1431 = ORIENTED_EDGE ( 'NONE', *, *, #16531, .F. ) ;
#1432 = ORIENTED_EDGE ( 'NONE', *, *, #33576, .T. ) ;
#1433 = DIRECTION ( 'NONE',  ( 0.000000000000000000, 0.000000000000000000, 1.000000000000000000 ) ) ;
#1434 = CARTESIAN_POINT ( 'NONE',  ( -12.97563234535667753, 90.60231327712331506, 12.49999999999999822 ) ) ;
#1435 = CIRCLE ( 'NONE', #13418, 1.999999999999998224 ) ;
#1436 = DIRECTION ( 'NONE',  ( -1.000000000000000000, 0.000000000000000000, 0.000000000000000000 ) ) ;
#1437 = ORIENTED_EDGE ( 'NONE', *, *, #3221, .F. ) ;
#1438 = DIRECTION ( 'NONE',  ( 0.000000000000000000, 0.000000000000000000, 1.000000000000000000 ) ) ;
#1439 = DIRECTION ( 'NONE',  ( 0.000000000000000000, 0.000000000000000000, -1.000000000000000000 ) ) ;
#1440 = CARTESIAN_POINT ( 'NONE',  ( 0.000000000000000000, 0.000000000000000000, -6.000000000000000000 ) ) ;
#1441 = DIRECTION ( 'NONE',  ( 1.000000000000000000, 0.000000000000000000, 0.000000000000000000 ) ) ;
#1442 = VERTEX_POINT ( 'NONE', #16390 ) ;
#1443 = VECTOR ( 'NONE', #18597, 1000.000000000000000 ) ;
#1444 = EDGE_LOOP ( 'NONE', ( #13748, #34243, #10343, #4834 ) ) ;
#1445 = CARTESIAN_POINT ( 'NONE',  ( -67.00000337463102085, 43.30127018922198801, -5.000000000000000000 ) ) ;
#1446 = AXIS2_PLACEMENT_3D ( 'NONE', #12156, #3929, #12722 ) ;
#1447 = CARTESIAN_POINT ( 'NONE',  ( -47.00000337463112743, -60.62177826491080168, -5.000000000000000000 ) ) ;
#1448 = ORIENTED_EDGE ( 'NONE', *, *, #31242, .F. ) ;
#1449 = DIRECTION ( 'NONE',  ( 1.000000000000000000, 0.000000000000000000, 0.000000000000000000 ) ) ;
#1450 = VERTEX_POINT ( 'NONE', #33079 ) ;
#1451 = DIRECTION ( 'NONE',  ( 0.000000000000000000, 0.000000000000000000, -1.000000000000000000 ) ) ;
#1452 = FACE_BOUND ( 'NONE', #19243, .T. ) ;
#1453 = EDGE_LOOP ( 'NONE', ( #36341, #23972 ) ) ;
#1454 = EDGE_LOOP ( 'NONE', ( #18816, #5074, #35697, #7195 ) ) ;
#1455 = ADVANCED_FACE ( 'NONE', ( #1583 ), #7952, .F. ) ;
#1456 = CIRCLE ( 'NONE', #277, 3.499999999999996003 ) ;
#1457 = DIRECTION ( 'NONE',  ( -1.000000000000000000, 0.000000000000000000, -0.000000000000000000 ) ) ;
#1458 = EDGE_LOOP ( 'NONE', ( #32965, #6091, #32772, #35012 ) ) ;
#1459 = SURFACE_SIDE_STYLE ('',( #35797 ) ) ;
#1460 = DIRECTION ( 'NONE',  ( 0.000000000000000000, 0.000000000000000000, 1.000000000000000000 ) ) ;
#1461 = CARTESIAN_POINT ( 'NONE',  ( 49.99999662536848177, -51.96152422706640550, -9.999999999999998224 ) ) ;
#1462 = DIRECTION ( 'NONE',  ( -0.000000000000000000, -0.000000000000000000, 1.000000000000000000 ) ) ;
#1463 = ORIENTED_EDGE ( 'NONE', *, *, #22294, .F. ) ;
#1464 = CARTESIAN_POINT ( 'NONE',  ( -70.00000337463099243, -2.428612866367529932E-14, -5.000000000000000000 ) ) ;
#1465 = CYLINDRICAL_SURFACE ( 'NONE', #16620, 2.000000000000001776 ) ;
#1466 = EDGE_LOOP ( 'NONE', ( #1037, #34759 ) ) ;
#1467 = CIRCLE ( 'NONE', #8064, 27.00000000000001776 ) ;
#1468 = ORIENTED_EDGE ( 'NONE', *, *, #30969, .F. ) ;
#1469 = ORIENTED_EDGE ( 'NONE', *, *, #25869, .F. ) ;
#1470 = DIRECTION ( 'NONE',  ( -1.000000000000000000, 0.000000000000000000, -0.000000000000000000 ) ) ;
#1471 = CIRCLE ( 'NONE', #801, 33.00000000000001421 ) ;
#1472 = DIRECTION ( 'NONE',  ( 0.000000000000000000, 0.000000000000000000, 1.000000000000000000 ) ) ;
#1473 = VERTEX_POINT ( 'NONE', #30259 ) ;
#1474 = CARTESIAN_POINT ( 'NONE',  ( 21.99999662536862033, -86.60254037844400443, -9.999999999999998224 ) ) ;
#1475 = DIRECTION ( 'NONE',  ( 1.000000000000000000, 0.000000000000000000, 0.000000000000000000 ) ) ;
#1476 = EDGE_CURVE ( 'NONE', #7505, #6635, #33092, .T. ) ;
#1477 = ORIENTED_EDGE ( 'NONE', *, *, #35526, .F. ) ;
#1478 = FACE_OUTER_BOUND ( 'NONE', #30171, .T. ) ;
#1479 = EDGE_CURVE ( 'NONE', #4566, #16555, #10953, .T. ) ;
#1480 = CARTESIAN_POINT ( 'NONE',  ( 47.99999662536846756, 51.96152422706637708, -9.999999999999998224 ) ) ;
#1481 = AXIS2_PLACEMENT_3D ( 'NONE', #17552, #6123, #28977 ) ;
#1482 = DIRECTION ( 'NONE',  ( 0.000000000000000000, 0.000000000000000000, 1.000000000000000000 ) ) ;
#1483 = DIRECTION ( 'NONE',  ( 0.000000000000000000, 0.000000000000000000, 1.000000000000000000 ) ) ;
#1484 = VECTOR ( 'NONE', #4946, 1000.000000000000000 ) ;
#1485 = CARTESIAN_POINT ( 'NONE',  ( 3.000000000000000000, 0.000000000000000000, 0.000000000000000000 ) ) ;
#1486 = CARTESIAN_POINT ( 'NONE',  ( -63.00000337463102085, 43.30127018922198801, -9.999999999999998224 ) ) ;
#1487 = ORIENTED_EDGE ( 'NONE', *, *, #33305, .F. ) ;
#1488 = CIRCLE ( 'NONE', #28409, 1.750000000000018652 ) ;
#1489 = ORIENTED_EDGE ( 'NONE', *, *, #31945, .T. ) ;
#1490 = EDGE_CURVE ( 'NONE', #35726, #27793, #15131, .T. ) ;
#1491 = CARTESIAN_POINT ( 'NONE',  ( -71.20512444582767841, -36.23716251175871861, 12.50000000000000000 ) ) ;
#1492 = DIRECTION ( 'NONE',  ( -1.000000000000000000, 0.000000000000000000, 0.000000000000000000 ) ) ;
#1493 = DIRECTION ( 'NONE',  ( 0.000000000000000000, 0.000000000000000000, 1.000000000000000000 ) ) ;
#1494 = CARTESIAN_POINT ( 'NONE',  ( 62.97617850287784336, 4.279621169095339184, -4.999999999999997335 ) ) ;
#1495 = ORIENTED_EDGE ( 'NONE', *, *, #19939, .T. ) ;
#1496 = CIRCLE ( 'NONE', #21248, 2.000000000000001776 ) ;
#1497 = DIRECTION ( 'NONE',  ( 1.000000000000000000, 0.000000000000000000, 0.000000000000000000 ) ) ;
#1498 = AXIS2_PLACEMENT_3D ( 'NONE', #17511, #11883, #32492 ) ;
#1499 = FACE_OUTER_BOUND ( 'NONE', #31519, .T. ) ;
#1500 = VERTEX_POINT ( 'NONE', #33651 ) ;
#1501 = ADVANCED_FACE ( 'NONE', ( #13578 ), #30806, .F. ) ;
#1502 = DIRECTION ( 'NONE',  ( 0.8660254037844415942, 0.4999999999999949485, 0.000000000000000000 ) ) ;
#1503 = ORIENTED_EDGE ( 'NONE', *, *, #8246, .T. ) ;
#1504 = CARTESIAN_POINT ( 'NONE',  ( -63.00000337463102085, 60.62177826491077326, -5.000000000000000000 ) ) ;
#1505 = PLANE ( 'NONE',  #24805 ) ;
#1506 = DIRECTION ( 'NONE',  ( 0.000000000000000000, 0.000000000000000000, -1.000000000000000000 ) ) ;
#1507 = ORIENTED_EDGE ( 'NONE', *, *, #7577, .F. ) ;
#1508 = CIRCLE ( 'NONE', #3918, 2.000000000000001776 ) ;
#1509 = ORIENTED_EDGE ( 'NONE', *, *, #29374, .F. ) ;
#1510 = CIRCLE ( 'NONE', #18899, 2.000000000000001776 ) ;
#1511 = AXIS2_PLACEMENT_3D ( 'NONE', #14031, #5250, #11415 ) ;
#1512 = VERTEX_POINT ( 'NONE', #25037 ) ;
#1513 = DIRECTION ( 'NONE',  ( 0.000000000000000000, 0.4999999999999953926, 0.8660254037844412611 ) ) ;
#1514 = EDGE_CURVE ( 'NONE', #5475, #15339, #27261, .T. ) ;
#1515 = DIRECTION ( 'NONE',  ( 1.000000000000000000, 0.000000000000000000, 0.000000000000000000 ) ) ;
#1516 = FACE_OUTER_BOUND ( 'NONE', #15122, .T. ) ;
#1517 = DIRECTION ( 'NONE',  ( 0.000000000000000000, 0.000000000000000000, 1.000000000000000000 ) ) ;
#1518 = DIRECTION ( 'NONE',  ( -0.000000000000000000, -0.000000000000000000, 1.000000000000000000 ) ) ;
#1519 = EDGE_CURVE ( 'NONE', #19586, #29300, #15755, .T. ) ;
#1520 = ORIENTED_EDGE ( 'NONE', *, *, #19030, .F. ) ;
#1521 = CARTESIAN_POINT ( 'NONE',  ( 0.3000000000000016542, 0.000000000000000000, 4.700000000000000178 ) ) ;
#1522 = CONICAL_SURFACE ( 'NONE', #30306, 5.000000000000000888, 1.047197551196596299 ) ;
#1523 = LINE ( 'NONE', #27030, #20347 ) ;
#1524 = DIRECTION ( 'NONE',  ( 1.000000000000000000, 0.000000000000000000, 0.000000000000000000 ) ) ;
#1525 = ORIENTED_EDGE ( 'NONE', *, *, #24071, .F. ) ;
#1526 =( REPRESENTATION_RELATIONSHIP ('NONE','NONE', #15268, #35880 ) REPRESENTATION_RELATIONSHIP_WITH_TRANSFORMATION ( #2536 )SHAPE_REPRESENTATION_RELATIONSHIP( ) );
#1527 = PLANE ( 'NONE',  #22645 ) ;
#1528 = EDGE_CURVE ( 'NONE', #18637, #8974, #28017, .T. ) ;
#1529 = CARTESIAN_POINT ( 'NONE',  ( 74.99999662536836809, -8.660254037844401509, -5.000000000000000000 ) ) ;
#1530 = ORIENTED_EDGE ( 'NONE', *, *, #26753, .T. ) ;
#1531 = ORIENTED_EDGE ( 'NONE', *, *, #950, .F. ) ;
#1532 = EDGE_CURVE ( 'NONE', #203, #14513, #36712, .T. ) ;
#1533 = AXIS2_PLACEMENT_3D ( 'NONE', #19025, #1573, #24260 ) ;
#1534 = CARTESIAN_POINT ( 'NONE',  ( -33.21453780030408609, 78.84345928898012801, 12.50000000000000000 ) ) ;
#1535 = DIRECTION ( 'NONE',  ( 0.8660254037844418162, 0.4999999999999946709, 0.000000000000000000 ) ) ;
#1536 = CIRCLE ( 'NONE', #20030, 2.000000000000001776 ) ;
#1537 = CARTESIAN_POINT ( 'NONE',  ( -3.374631303565411855E-06, -86.60254037844400443, -9.999999999999998224 ) ) ;
#1538 = EDGE_LOOP ( 'NONE', ( #27083, #20318, #20390, #7384 ) ) ;
#1539 = VERTEX_POINT ( 'NONE', #15834 ) ;
#1540 = AXIS2_PLACEMENT_3D ( 'NONE', #7269, #15702, #21694 ) ;
#1541 = ORIENTED_EDGE ( 'NONE', *, *, #26643, .F. ) ;
#1542 = AXIS2_PLACEMENT_3D ( 'NONE', #17829, #32260, #1321 ) ;
#1543 = CIRCLE ( 'NONE', #22505, 2.000000000000001776 ) ;
#1544 = VECTOR ( 'NONE', #1270, 1000.000000000000000 ) ;
#1545 = DIRECTION ( 'NONE',  ( 0.000000000000000000, 0.000000000000000000, -1.000000000000000000 ) ) ;
#1546 = EDGE_LOOP ( 'NONE', ( #8388, #6636, #36440, #37077, #4577 ) ) ;
#1547 = ORIENTED_EDGE ( 'NONE', *, *, #35364, .T. ) ;
#1548 = LINE ( 'NONE', #7553, #15964 ) ;
#1549 = AXIS2_PLACEMENT_3D ( 'NONE', #1991, #5387, #13621 ) ;
#1550 = ORIENTED_EDGE ( 'NONE', *, *, #8819, .T. ) ;
#1551 = ORIENTED_EDGE ( 'NONE', *, *, #3941, .F. ) ;
#1552 = CIRCLE ( 'NONE', #14725, 2.000000000000001776 ) ;
#1553 = EDGE_CURVE ( 'NONE', #22833, #3127, #13021, .T. ) ;
#1554 = DIRECTION ( 'NONE',  ( 0.000000000000000000, 0.000000000000000000, -1.000000000000000000 ) ) ;
#1555 = DIRECTION ( 'NONE',  ( 0.000000000000000000, 0.000000000000000000, 1.000000000000000000 ) ) ;
#1556 = ORIENTED_EDGE ( 'NONE', *, *, #15598, .T. ) ;
#1557 = ORIENTED_EDGE ( 'NONE', *, *, #9070, .F. ) ;
#1558 = CYLINDRICAL_SURFACE ( 'NONE', #1759, 2.000000000000001776 ) ;
#1559 = CARTESIAN_POINT ( 'NONE',  ( 0.000000000000000000, 89.94802294027088863, 27.49999999999999645 ) ) ;
#1560 = CIRCLE ( 'NONE', #34490, 33.00000000000001421 ) ;
#1561 = EDGE_CURVE ( 'NONE', #14131, #20810, #27705, .T. ) ;
#1562 = LINE ( 'NONE', #1014, #26450 ) ;
#1563 = CARTESIAN_POINT ( 'NONE',  ( 35.19434990244975126, -52.39915983220758022, -4.999999999999997335 ) ) ;
#1564 = AXIS2_PLACEMENT_3D ( 'NONE', #35486, #21209, #31310 ) ;
#1565 = ORIENTED_EDGE ( 'NONE', *, *, #10566, .T. ) ;
#1566 = DIRECTION ( 'NONE',  ( 1.000000000000000000, 0.000000000000000000, 0.000000000000000000 ) ) ;
#1568 = ORIENTED_EDGE ( 'NONE', *, *, #6656, .T. ) ;
#1567 = EDGE_CURVE ( 'NONE', #4390, #26755, #33266, .T. ) ;
#1569 = CARTESIAN_POINT ( 'NONE',  ( 1.999996625368665182, 69.28203230275516944, 12.50000000000000000 ) ) ;
#1570 = DIRECTION ( 'NONE',  ( -0.000000000000000000, -0.000000000000000000, 1.000000000000000000 ) ) ;
#1571 = CARTESIAN_POINT ( 'NONE',  ( 56.99999662536844625, 60.62177826491077326, -9.999999999999998224 ) ) ;
#1572 = CIRCLE ( 'NONE', #34528, 2.000000000000001776 ) ;
#1573 = DIRECTION ( 'NONE',  ( 0.000000000000000000, 0.000000000000000000, 1.000000000000000000 ) ) ;
#1574 = AXIS2_PLACEMENT_3D ( 'NONE', #3758, #12169, #9192 ) ;
#1575 = CARTESIAN_POINT ( 'NONE',  ( 57.99999662536842493, 51.96152422706639129, -9.999999999999998224 ) ) ;
#1576 = AXIS2_PLACEMENT_3D ( 'NONE', #33824, #8134, #28196 ) ;
#1577 = CIRCLE ( 'NONE', #9955, 2.000000000000001776 ) ;
#1578 = CARTESIAN_POINT ( 'NONE',  ( -5.000000000000000000, 30.00000000000000355, -15.00000000000000000 ) ) ;
#1579 = CARTESIAN_POINT ( 'NONE',  ( 42.97377950131527058, 96.90768712682506703, -19.99999999999999645 ) ) ;
#1580 = EDGE_LOOP ( 'NONE', ( #25200, #16709 ) ) ;
#1581 = DIRECTION ( 'NONE',  ( 1.000000000000000000, 0.000000000000000000, 0.000000000000000000 ) ) ;
#1582 = DIRECTION ( 'NONE',  ( 1.000000000000000000, 0.000000000000000000, 0.000000000000000000 ) ) ;
#1583 = FACE_OUTER_BOUND ( 'NONE', #16361, .T. ) ;
#1584 = VERTEX_POINT ( 'NONE', #1949 ) ;
#1585 = AXIS2_PLACEMENT_3D ( 'NONE', #25400, #37035, #11339 ) ;
#1586 = ORIENTED_EDGE ( 'NONE', *, *, #29687, .F. ) ;
#1587 = ORIENTED_EDGE ( 'NONE', *, *, #4704, .F. ) ;
#1588 = EDGE_CURVE ( 'NONE', #27568, #6775, #22026, .T. ) ;
#1589 = CYLINDRICAL_SURFACE ( 'NONE', #32182, 3.500000000000003109 ) ;
#1590 = FACE_OUTER_BOUND ( 'NONE', #36859, .T. ) ;
#1591 = ORIENTED_EDGE ( 'NONE', *, *, #11289, .F. ) ;
#1592 = AXIS2_PLACEMENT_3D ( 'NONE', #7939, #13558, #22759 ) ;
#1593 = CARTESIAN_POINT ( 'NONE',  ( 76.99999662536836809, -8.660254037844401509, -9.999999999999998224 ) ) ;
#1594 = VECTOR ( 'NONE', #36557, 1000.000000000000000 ) ;
#1595 = DIRECTION ( 'NONE',  ( -1.000000000000000000, 0.000000000000000000, 0.000000000000000000 ) ) ;
#1596 = ORIENTED_EDGE ( 'NONE', *, *, #13699, .T. ) ;
#1597 = DIRECTION ( 'NONE',  ( 0.000000000000000000, 0.000000000000000000, 1.000000000000000000 ) ) ;
#1598 = VERTEX_POINT ( 'NONE', #5514 ) ;
#1599 = AXIS2_PLACEMENT_3D ( 'NONE', #7852, #7463, #14197 ) ;
#1600 = CARTESIAN_POINT ( 'NONE',  ( 4.999996625368676284, -77.94228634059960825, -9.999999999999998224 ) ) ;
#1601 = CONICAL_SURFACE ( 'NONE', #6387, 2.449999999999998845, 0.9599310885968813656 ) ;
#1602 = VECTOR ( 'NONE', #7826, 1000.000000000000000 ) ;
#1603 = ADVANCED_FACE ( 'NONE', ( #17489 ), #31735, .F. ) ;
#1604 = CARTESIAN_POINT ( 'NONE',  ( -108.3061974404900241, -19.22934205794863516, 27.50000000000000000 ) ) ;
#1605 = CARTESIAN_POINT ( 'NONE',  ( 4.242640687119310527, 4.242640687119267007, 32.50000000000000000 ) ) ;
#1606 = LINE ( 'NONE', #24292, #33163 ) ;
#1607 = EDGE_CURVE ( 'NONE', #14541, #13732, #10344, .T. ) ;
#1608 = EDGE_LOOP ( 'NONE', ( #5690, #20874 ) ) ;
#1609 = FACE_OUTER_BOUND ( 'NONE', #3806, .T. ) ;
#1610 = AXIS2_PLACEMENT_3D ( 'NONE', #2864, #34538, #23465 ) ;
#1611 = EDGE_CURVE ( 'NONE', #18695, #36878, #1372, .T. ) ;
#1612 = CARTESIAN_POINT ( 'NONE',  ( -4.279621169095561228, 62.97617850287782915, 12.49999999999999822 ) ) ;
#1613 = DIRECTION ( 'NONE',  ( 1.000000000000000000, 0.000000000000000000, 0.000000000000000000 ) ) ;
#1614 = DIRECTION ( 'NONE',  ( -0.000000000000000000, -0.000000000000000000, 1.000000000000000000 ) ) ;
#1615 = DIRECTION ( 'NONE',  ( 0.000000000000000000, 0.000000000000000000, 1.000000000000000000 ) ) ;
#1616 = ORIENTED_EDGE ( 'NONE', *, *, #35479, .T. ) ;
#1617 = CARTESIAN_POINT ( 'NONE',  ( 101.7384897088151234, 110.2237710830533217, 32.50000000000000000 ) ) ;
#1618 = EDGE_CURVE ( 'NONE', #32403, #22417, #8507, .T. ) ;
#1619 = DIRECTION ( 'NONE',  ( 0.000000000000000000, -0.000000000000000000, 1.000000000000000000 ) ) ;
#1620 = CARTESIAN_POINT ( 'NONE',  ( 5.000000000000000888, 0.000000000000000000, 13.31572692736085095 ) ) ;
#1621 = CONICAL_SURFACE ( 'NONE', #14196, 5.000000000000000888, 1.047197551196596299 ) ;
#1622 = EDGE_CURVE ( 'NONE', #20027, #10852, #65, .T. ) ;
#1623 = AXIS2_PLACEMENT_3D ( 'NONE', #31306, #2630, #17062 ) ;
#1624 = ORIENTED_EDGE ( 'NONE', *, *, #19700, .T. ) ;
#1625 = AXIS2_PLACEMENT_3D ( 'NONE', #33468, #10027, #21825 ) ;
#1626 = VERTEX_POINT ( 'NONE', #11859 ) ;
#1627 = CARTESIAN_POINT ( 'NONE',  ( -65.63757354697304436, -58.72612421542294925, -5.000000000000000000 ) ) ;
#1628 = LINE ( 'NONE', #1077, #31477 ) ;
#1629 = EDGE_CURVE ( 'NONE', #17931, #34610, #34305, .T. ) ;
#1630 =( GEOMETRIC_REPRESENTATION_CONTEXT ( 3 ) GLOBAL_UNCERTAINTY_ASSIGNED_CONTEXT ( ( #8434 ) ) GLOBAL_UNIT_ASSIGNED_CONTEXT ( ( #30742, #18767, #10319 ) ) REPRESENTATION_CONTEXT ( 'NONE', 'WORKASPACE' ) );
#1631 = VECTOR ( 'NONE', #33925, 1000.000000000000000 ) ;
#1632 = EDGE_CURVE ( 'NONE', #26415, #8015, #1965, .T. ) ;
#1633 = DIRECTION ( 'NONE',  ( -0.000000000000000000, -0.000000000000000000, 1.000000000000000000 ) ) ;
#1634 = AXIS2_PLACEMENT_3D ( 'NONE', #15649, #9822, #29692 ) ;
#1635 = ORIENTED_EDGE ( 'NONE', *, *, #29591, .F. ) ;
#1636 = ADVANCED_FACE ( 'NONE', ( #19937 ), #2690, .F. ) ;
#1637 = CARTESIAN_POINT ( 'NONE',  ( 89.42901512340354486, -31.83425564451495404, -5.000000000000011546 ) ) ;
#1638 = DIRECTION ( 'NONE',  ( 0.000000000000000000, 0.000000000000000000, 1.000000000000000000 ) ) ;
#1639 = EDGE_CURVE ( 'NONE', #33094, #3043, #8408, .T. ) ;
#1640 = DIRECTION ( 'NONE',  ( 0.000000000000000000, 0.000000000000000000, 1.000000000000000000 ) ) ;
#1641 = AXIS2_PLACEMENT_3D ( 'NONE', #16254, #4438, #15690 ) ;
#1642 = DIRECTION ( 'NONE',  ( -1.000000000000000000, 0.000000000000000000, 0.000000000000000000 ) ) ;
#1643 = ORIENTED_EDGE ( 'NONE', *, *, #12876, .F. ) ;
#1644 = CIRCLE ( 'NONE', #32165, 2.000000000000001776 ) ;
#1645 = ORIENTED_EDGE ( 'NONE', *, *, #24791, .T. ) ;
#1646 = CARTESIAN_POINT ( 'NONE',  ( -3.374631334790434423E-06, 69.28203230275516944, 17.49999999999999645 ) ) ;
#1647 = AXIS2_PLACEMENT_3D ( 'NONE', #239, #23496, #11502 ) ;
#1648 = DIRECTION ( 'NONE',  ( 1.000000000000000000, 0.000000000000000000, 0.000000000000000000 ) ) ;
#1649 = EDGE_LOOP ( 'NONE', ( #22777, #456 ) ) ;
#1650 = PLANE ( 'NONE',  #21521 ) ;
#1651 = ORIENTED_EDGE ( 'NONE', *, *, #32671, .F. ) ;
#1652 = CIRCLE ( 'NONE', #23814, 3.750000000000001776 ) ;
#1653 = CARTESIAN_POINT ( 'NONE',  ( -87.00000337463093558, -25.98076211353322051, -9.999999999999998224 ) ) ;
#1654 = AXIS2_PLACEMENT_3D ( 'NONE', #21908, #16119, #17845 ) ;
#1655 = AXIS2_PLACEMENT_3D ( 'NONE', #22166, #9973, #21972 ) ;
#1656 = DIRECTION ( 'NONE',  ( 0.000000000000000000, 0.000000000000000000, 1.000000000000000000 ) ) ;
#1657 = ORIENTED_EDGE ( 'NONE', *, *, #3901, .F. ) ;
#1658 = DIRECTION ( 'NONE',  ( 0.000000000000000000, 0.000000000000000000, 1.000000000000000000 ) ) ;
#1659 = VERTEX_POINT ( 'NONE', #19776 ) ;
#1660 = AXIS2_PLACEMENT_3D ( 'NONE', #17232, #31452, #28655 ) ;
#1661 = LINE ( 'NONE', #35609, #19441 ) ;
#1662 = AXIS2_PLACEMENT_3D ( 'NONE', #10916, #2869, #19363 ) ;
#1663 = DIRECTION ( 'NONE',  ( 1.000000000000000000, 0.000000000000000000, 0.000000000000000000 ) ) ;
#1664 = DIRECTION ( 'NONE',  ( 0.000000000000000000, 0.000000000000000000, 1.000000000000000000 ) ) ;
#1665 = ORIENTED_EDGE ( 'NONE', *, *, #11193, .F. ) ;
#1666 = DIRECTION ( 'NONE',  ( 1.000000000000000000, 0.000000000000000000, 0.000000000000000000 ) ) ;
#1667 = CARTESIAN_POINT ( 'NONE',  ( -107.0891125874437506, 43.89216747908891136, 32.49999999999999289 ) ) ;
#1668 = CIRCLE ( 'NONE', #11246, 2.000000000000001776 ) ;
#1669 = CARTESIAN_POINT ( 'NONE',  ( 7.999996625368656744, -86.60254037844400443, -9.999999999999998224 ) ) ;
#1670 = VERTEX_POINT ( 'NONE', #11496 ) ;
#1671 = ORIENTED_EDGE ( 'NONE', *, *, #5157, .F. ) ;
#1672 = ORIENTED_EDGE ( 'NONE', *, *, #4969, .F. ) ;
#1673 = LINE ( 'NONE', #26984, #868 ) ;
#1674 = VECTOR ( 'NONE', #17302, 1000.000000000000000 ) ;
#1675 = DIRECTION ( 'NONE',  ( 0.000000000000000000, 0.000000000000000000, 1.000000000000000000 ) ) ;
#1676 = ORIENTED_EDGE ( 'NONE', *, *, #34306, .F. ) ;
#1677 = AXIS2_PLACEMENT_3D ( 'NONE', #27123, #4086, #26955 ) ;
#1678 = AXIS2_PLACEMENT_3D ( 'NONE', #15413, #32459, #12757 ) ;
#1679 = CARTESIAN_POINT ( 'NONE',  ( -5.000000000000000000, -0.5603747650654237189, -0.5678343202077608121 ) ) ;
#1680 = DIRECTION ( 'NONE',  ( 0.000000000000000000, 0.000000000000000000, 1.000000000000000000 ) ) ;
#1681 = DIRECTION ( 'NONE',  ( 1.000000000000000000, 0.000000000000000000, 0.000000000000000000 ) ) ;
#1682 = AXIS2_PLACEMENT_3D ( 'NONE', #32550, #32944, #19074 ) ;
#1683 = EDGE_CURVE ( 'NONE', #28818, #26555, #34167, .T. ) ;
#1684 = FACE_OUTER_BOUND ( 'NONE', #25442, .T. ) ;
#1685 = AXIS2_PLACEMENT_3D ( 'NONE', #746, #20437, #6574 ) ;
#1686 = ADVANCED_FACE ( 'NONE', ( #13938 ), #31198, .F. ) ;
#1687 = ADVANCED_FACE ( 'NONE', ( #14121 ), #16779, .T. ) ;
#1688 = DIRECTION ( 'NONE',  ( -0.000000000000000000, -0.000000000000000000, 1.000000000000000000 ) ) ;
#1689 = FACE_OUTER_BOUND ( 'NONE', #12212, .T. ) ;
#1690 = LINE ( 'NONE', #32433, #24985 ) ;
#1691 = DIRECTION ( 'NONE',  ( -1.000000000000000000, 0.000000000000000000, -0.000000000000000000 ) ) ;
#1692 = ORIENTED_EDGE ( 'NONE', *, *, #6728, .T. ) ;
#1693 = EDGE_LOOP ( 'NONE', ( #15183, #32670 ) ) ;
#1694 = CIRCLE ( 'NONE', #8856, 33.00000000000001421 ) ;
#1695 = DIRECTION ( 'NONE',  ( 0.5000000000000038858, 0.8660254037844363761, 0.000000000000000000 ) ) ;
#1696 = DIRECTION ( 'NONE',  ( 0.000000000000000000, 0.000000000000000000, -1.000000000000000000 ) ) ;
#1697 = DIRECTION ( 'NONE',  ( 0.000000000000000000, 0.000000000000000000, 1.000000000000000000 ) ) ;
#1698 = CARTESIAN_POINT ( 'NONE',  ( -78.00000337463094979, 34.64101615137757051, 12.50000000000000000 ) ) ;
#1699 = ORIENTED_EDGE ( 'NONE', *, *, #20552, .T. ) ;
#1700 = CIRCLE ( 'NONE', #22657, 3.000000000000003997 ) ;
#1701 = DIRECTION ( 'NONE',  ( 1.000000000000000000, 0.000000000000000000, 0.000000000000000000 ) ) ;
#1702 = DIRECTION ( 'NONE',  ( 0.000000000000000000, 0.000000000000000000, 1.000000000000000000 ) ) ;
#1703 = CARTESIAN_POINT ( 'NONE',  ( 5.000000000000000000, 6.074766241781102566E-16, -0.5080592402122449114 ) ) ;
#1704 = AXIS2_PLACEMENT_3D ( 'NONE', #36443, #2108, #22189 ) ;
#1705 = ORIENTED_EDGE ( 'NONE', *, *, #11357, .F. ) ;
#1706 = AXIS2_PLACEMENT_3D ( 'NONE', #9005, #11439, #32023 ) ;
#1707 = DIRECTION ( 'NONE',  ( 0.000000000000000000, 0.000000000000000000, 1.000000000000000000 ) ) ;
#1708 = ORIENTED_EDGE ( 'NONE', *, *, #31388, .F. ) ;
#1709 = EDGE_CURVE ( 'NONE', #6799, #27465, #31362, .T. ) ;
#1710 = AXIS2_PLACEMENT_3D ( 'NONE', #11524, #12065, #25969 ) ;
#1711 = CARTESIAN_POINT ( 'NONE',  ( -65.00000337463104927, -43.30127018922202353, 12.50000000000000000 ) ) ;
#1712 = CARTESIAN_POINT ( 'NONE',  ( -67.30619744049063513, -84.18124734178186941, 27.50000000000000000 ) ) ;
#1713 = CIRCLE ( 'NONE', #31355, 2.000000000000000000 ) ;
#1714 = CARTESIAN_POINT ( 'NONE',  ( -42.00000337463114164, -69.28203230275519786, -9.999999999999998224 ) ) ;
#1715 = EDGE_LOOP ( 'NONE', ( #15994, #30159, #25758, #23139 ) ) ;
#1716 = ORIENTED_EDGE ( 'NONE', *, *, #3941, .T. ) ;
#1717 = VECTOR ( 'NONE', #5646, 1000.000000000000000 ) ;
#1718 = CYLINDRICAL_SURFACE ( 'NONE', #25165, 2.000000000000001776 ) ;
#1719 = CIRCLE ( 'NONE', #23887, 2.000000000000001776 ) ;
#1720 = ORIENTED_EDGE ( 'NONE', *, *, #15375, .T. ) ;
#1721 = CARTESIAN_POINT ( 'NONE',  ( -3.374631303565411855E-06, -86.60254037844400443, -9.999999999999998224 ) ) ;
#1722 = FACE_BOUND ( 'NONE', #31894, .T. ) ;
#1723 = DIRECTION ( 'NONE',  ( 0.000000000000000000, 0.000000000000000000, 1.000000000000000000 ) ) ;
#1724 = CARTESIAN_POINT ( 'NONE',  ( 84.99999662536832545, 8.660254037844394404, 17.49999999999999645 ) ) ;
#1725 = DIRECTION ( 'NONE',  ( 1.000000000000000000, 0.000000000000000000, 0.000000000000000000 ) ) ;
#1726 = ORIENTED_EDGE ( 'NONE', *, *, #4042, .F. ) ;
#1727 = CARTESIAN_POINT ( 'NONE',  ( 0.000000000000000000, 0.000000000000000000, -25.03750572909317285 ) ) ;
#1728 = CARTESIAN_POINT ( 'NONE',  ( 69.99999662536839651, -17.32050807568879947, 12.50000000000000000 ) ) ;
#1729 = EDGE_CURVE ( 'NONE', #1410, #9726, #21578, .T. ) ;
#1730 = SURFACE_STYLE_USAGE ( .BOTH. , #15979 ) ;
#1731 = ORIENTED_EDGE ( 'NONE', *, *, #30960, .T. ) ;
#1732 = CYLINDRICAL_SURFACE ( 'NONE', #20808, 2.000000000000001776 ) ;
#1733 = AXIS2_PLACEMENT_3D ( 'NONE', #24641, #18643, #30236 ) ;
#1734 = CARTESIAN_POINT ( 'NONE',  ( -14.80603122773057478, 87.83969979969877784, 12.49999999999999645 ) ) ;
#1735 = ORIENTED_EDGE ( 'NONE', *, *, #31425, .F. ) ;
#1736 = ORIENTED_EDGE ( 'NONE', *, *, #27714, .T. ) ;
#1737 = FACE_OUTER_BOUND ( 'NONE', #10885, .T. ) ;
#1738 = DIRECTION ( 'NONE',  ( 0.000000000000000000, 0.000000000000000000, 1.000000000000000000 ) ) ;
#1739 = CARTESIAN_POINT ( 'NONE',  ( -103.1837590831665210, -33.77668192579397299, 32.49999999999999289 ) ) ;
#1740 = ORIENTED_EDGE ( 'NONE', *, *, #24255, .T. ) ;
#1741 = ORIENTED_EDGE ( 'NONE', *, *, #33937, .F. ) ;
#1742 = ORIENTED_EDGE ( 'NONE', *, *, #2060, .T. ) ;
#1743 = CARTESIAN_POINT ( 'NONE',  ( 74.99999662536836809, 8.660254037844394404, 17.49999999999999645 ) ) ;
#1744 = AXIS2_PLACEMENT_3D ( 'NONE', #22096, #25105, #7848 ) ;
#1745 = ORIENTED_EDGE ( 'NONE', *, *, #4190, .T. ) ;
#1746 = EDGE_CURVE ( 'NONE', #22366, #13981, #15602, .T. ) ;
#1747 = AXIS2_PLACEMENT_3D ( 'NONE', #10474, #33910, #8230 ) ;
#1748 = DIRECTION ( 'NONE',  ( -0.000000000000000000, -0.000000000000000000, 1.000000000000000000 ) ) ;
#1749 = ORIENTED_EDGE ( 'NONE', *, *, #32760, .T. ) ;
#1750 = EDGE_CURVE ( 'NONE', #19879, #6148, #24587, .T. ) ;
#1751 = ORIENTED_EDGE ( 'NONE', *, *, #1412, .F. ) ;
#1752 = DIRECTION ( 'NONE',  ( 0.8660254037844344888, -0.5000000000000071054, 0.000000000000000000 ) ) ;
#1753 = AXIS2_PLACEMENT_3D ( 'NONE', #4859, #27890, #2214 ) ;
#1754 = CARTESIAN_POINT ( 'NONE',  ( -32.00000337463118427, 69.28203230275516944, -9.999999999999998224 ) ) ;
#1755 = VERTEX_POINT ( 'NONE', #34763 ) ;
#1756 = ADVANCED_FACE ( 'NONE', ( #31013 ), #5349, .F. ) ;
#1757 = VERTEX_POINT ( 'NONE', #29099 ) ;
#1758 = CARTESIAN_POINT ( 'NONE',  ( 24.99999662536857059, 77.94228634059957983, -9.999999999999998224 ) ) ;
#1759 = AXIS2_PLACEMENT_3D ( 'NONE', #27439, #21803, #33242 ) ;
#1760 = DIRECTION ( 'NONE',  ( -0.000000000000000000, -0.000000000000000000, -1.000000000000000000 ) ) ;
#1761 = CARTESIAN_POINT ( 'NONE',  ( -48.00000337463109190, 69.28203230275518365, -9.999999999999998224 ) ) ;
#1762 = DIRECTION ( 'NONE',  ( 1.000000000000000000, 0.000000000000000000, 0.000000000000000000 ) ) ;
#1763 = ADVANCED_FACE ( 'NONE', ( #15051 ), #6979, .F. ) ;
#1764 = VERTEX_POINT ( 'NONE', #29856 ) ;
#1765 = CARTESIAN_POINT ( 'NONE',  ( 26.99999662536856704, 77.94228634059957983, 12.50000000000000000 ) ) ;
#1766 = CIRCLE ( 'NONE', #27510, 2.000000000000001776 ) ;
#1767 = ORIENTED_EDGE ( 'NONE', *, *, #6528, .F. ) ;
#1768 = CYLINDRICAL_SURFACE ( 'NONE', #23835, 95.00000000000001421 ) ;
#1769 = DIRECTION ( 'NONE',  ( 0.000000000000000000, 0.000000000000000000, 1.000000000000000000 ) ) ;
#1770 = FACE_BOUND ( 'NONE', #14736, .T. ) ;
#1771 = CARTESIAN_POINT ( 'NONE',  ( 0.000000000000000000, 84.16276890242652087, 42.47964607176039209 ) ) ;
#1772 = VECTOR ( 'NONE', #14188, 1000.000000000000000 ) ;
#1773 = CARTESIAN_POINT ( 'NONE',  ( 62.99999662536839651, 60.62177826491078747, -9.999999999999998224 ) ) ;
#1774 = AXIS2_PLACEMENT_3D ( 'NONE', #3510, #28973, #6503 ) ;
#1775 = CARTESIAN_POINT ( 'NONE',  ( 77.99999662536832545, -34.64101615137759183, -9.999999999999998224 ) ) ;
#1776 = EDGE_CURVE ( 'NONE', #36972, #30139, #36572, .T. ) ;
#1777 = FACE_OUTER_BOUND ( 'NONE', #33774, .T. ) ;
#1778 = ORIENTED_EDGE ( 'NONE', *, *, #9161, .F. ) ;
#1779 = LINE ( 'NONE', #24835, #26780 ) ;
#1780 = LINE ( 'NONE', #21267, #16549 ) ;
#1781 = DIRECTION ( 'NONE',  ( -0.000000000000000000, -0.000000000000000000, 1.000000000000000000 ) ) ;
#1782 = EDGE_LOOP ( 'NONE', ( #26880, #23235, #33783, #15243, #18109 ) ) ;
#1783 = ORIENTED_EDGE ( 'NONE', *, *, #10181, .F. ) ;
#1784 = ORIENTED_EDGE ( 'NONE', *, *, #22476, .T. ) ;
#1785 = CIRCLE ( 'NONE', #17947, 33.00000000000001421 ) ;
#1786 = CARTESIAN_POINT ( 'NONE',  ( -145.0000000000000568, 1.518182058997189877E-12, 32.55002500000000509 ) ) ;
#1787 = CARTESIAN_POINT ( 'NONE',  ( 145.0000000000000568, -5.056524707326808249E-13, 32.55002500000000509 ) ) ;
#1788 = CIRCLE ( 'NONE', #22754, 3.000000000000002665 ) ;
#1789 = ORIENTED_EDGE ( 'NONE', *, *, #19867, .T. ) ;
#1790 = EDGE_CURVE ( 'NONE', #17529, #13754, #14396, .T. ) ;
#1791 = DIRECTION ( 'NONE',  ( 0.000000000000000000, 0.000000000000000000, -1.000000000000000000 ) ) ;
#1792 = CARTESIAN_POINT ( 'NONE',  ( -10.00000337463125000, -86.60254037844400443, 12.50000000000000000 ) ) ;
#1793 = ORIENTED_EDGE ( 'NONE', *, *, #33669, .T. ) ;
#1794 = EDGE_CURVE ( 'NONE', #2651, #8103, #20385, .T. ) ;
#1795 = DIRECTION ( 'NONE',  ( 0.000000000000000000, 0.000000000000000000, 1.000000000000000000 ) ) ;
#1796 = EDGE_LOOP ( 'NONE', ( #35672, #5088 ) ) ;
#1797 = DIRECTION ( 'NONE',  ( 0.000000000000000000, 0.000000000000000000, 1.000000000000000000 ) ) ;
#1798 = AXIS2_PLACEMENT_3D ( 'NONE', #12044, #3087, #23504 ) ;
#1799 = CARTESIAN_POINT ( 'NONE',  ( 52.99999662536844625, -60.62177826491080168, -9.999999999999998224 ) ) ;
#1800 = FACE_OUTER_BOUND ( 'NONE', #612, .T. ) ;
#1801 = FACE_OUTER_BOUND ( 'NONE', #32971, .T. ) ;
#1802 = VECTOR ( 'NONE', #24216, 1000.000000000000000 ) ;
#1803 = EDGE_CURVE ( 'NONE', #32300, #36720, #36181, .T. ) ;
#1804 = ORIENTED_EDGE ( 'NONE', *, *, #487, .T. ) ;
#1805 = CARTESIAN_POINT ( 'NONE',  ( 5.000000000000000888, 0.000000000000000000, -6.000000000000000000 ) ) ;
#1806 = AXIS2_PLACEMENT_3D ( 'NONE', #8453, #14806, #25710 ) ;
#1807 = CONTEXT_DEPENDENT_SHAPE_REPRESENTATION ( #33637, #21154 ) ;
#1808 = DIRECTION ( 'NONE',  ( 0.000000000000000000, 0.000000000000000000, -1.000000000000000000 ) ) ;
#1809 = FACE_OUTER_BOUND ( 'NONE', #29343, .T. ) ;
#1810 = EDGE_CURVE ( 'NONE', #21528, #18894, #15223, .T. ) ;
#1811 = AXIS2_PLACEMENT_3D ( 'NONE', #3822, #16162, #6468 ) ;
#1812 = ORIENTED_EDGE ( 'NONE', *, *, #16207, .T. ) ;
#1813 = DIRECTION ( 'NONE',  ( -0.4999999999999980016, 0.8660254037844398178, 0.000000000000000000 ) ) ;
#1814 = CARTESIAN_POINT ( 'NONE',  ( 0.000000000000000000, -55.00000000000000000, -5.000000000000000888 ) ) ;
#1815 = EDGE_LOOP ( 'NONE', ( #19953, #7949 ) ) ;
#1816 = CARTESIAN_POINT ( 'NONE',  ( 34.99999662536855283, 60.62177826491078747, -9.999999999999998224 ) ) ;
#1817 = CARTESIAN_POINT ( 'NONE',  ( -47.63139720814438505, -27.49999999999955591, -15.00000000000000000 ) ) ;
#1818 = CARTESIAN_POINT ( 'NONE',  ( 24.99999662536857059, 77.94228634059957983, -9.999999999999998224 ) ) ;
#1819 = VERTEX_POINT ( 'NONE', #26310 ) ;
#1820 = VERTEX_POINT ( 'NONE', #31898 ) ;
#1821 = AXIS2_PLACEMENT_3D ( 'NONE', #788, #12032, #17866 ) ;
#1822 = DIRECTION ( 'NONE',  ( 0.000000000000000000, 0.000000000000000000, 1.000000000000000000 ) ) ;
#1823 = CARTESIAN_POINT ( 'NONE',  ( 59.99999662536842493, 51.96152422706639129, -9.999999999999998224 ) ) ;
#1824 = DIRECTION ( 'NONE',  ( 1.000000000000000000, 0.000000000000000000, 0.000000000000000000 ) ) ;
#1825 = EDGE_CURVE ( 'NONE', #6458, #10369, #18046, .T. ) ;
#1826 = ORIENTED_EDGE ( 'NONE', *, *, #3894, .T. ) ;
#1827 = AXIS2_PLACEMENT_3D ( 'NONE', #29849, #8087, #1908 ) ;
#1828 = FACE_OUTER_BOUND ( 'NONE', #3973, .T. ) ;
#1829 = CARTESIAN_POINT ( 'NONE',  ( 11.99999662536865763, -86.60254037844400443, -9.999999999999998224 ) ) ;
#1830 = CARTESIAN_POINT ( 'NONE',  ( 0.000000000000000000, -95.00000000000001421, 32.50002500000000083 ) ) ;
#1831 = CARTESIAN_POINT ( 'NONE',  ( -103.1654841881149025, 61.26096253783315859, 32.50000000000000711 ) ) ;
#1832 = EDGE_LOOP ( 'NONE', ( #22224, #2825 ) ) ;
#1833 = EDGE_CURVE ( 'NONE', #34764, #68, #34928, .T. ) ;
#1834 = EDGE_LOOP ( 'NONE', ( #17146, #25800, #28090, #24674 ) ) ;
#1835 = DIRECTION ( 'NONE',  ( 1.000000000000000000, 0.000000000000000000, 0.000000000000000000 ) ) ;
#1836 = FACE_OUTER_BOUND ( 'NONE', #32214, .T. ) ;
#1837 = ORIENTED_EDGE ( 'NONE', *, *, #25740, .T. ) ;
#1838 = ADVANCED_FACE ( 'NONE', ( #6231 ), #35497, .F. ) ;
#1839 = CARTESIAN_POINT ( 'NONE',  ( 65.63757102168601421, 58.72612563608866765, -5.000000000000000000 ) ) ;
#1840 = EDGE_CURVE ( 'NONE', #10511, #28959, #19203, .T. ) ;
#1841 = ORIENTED_EDGE ( 'NONE', *, *, #25449, .F. ) ;
#1842 = CARTESIAN_POINT ( 'NONE',  ( 17.99999662536858125, 86.60254037844397601, 12.50000000000000000 ) ) ;
#1843 = DIRECTION ( 'NONE',  ( 1.000000000000000000, 0.000000000000000000, 0.000000000000000000 ) ) ;
#1844 = EDGE_LOOP ( 'NONE', ( #2809, #20964 ) ) ;
#1845 = CARTESIAN_POINT ( 'NONE',  ( 32.99999662536855283, -60.62177826491080168, -5.000000000000000000 ) ) ;
#1846 = ORIENTED_EDGE ( 'NONE', *, *, #30808, .F. ) ;
#1847 = CARTESIAN_POINT ( 'NONE',  ( 67.99999662536838230, -17.32050807568879947, 17.49999999999999645 ) ) ;
#1848 = EDGE_CURVE ( 'NONE', #9530, #25810, #9620, .T. ) ;
#1849 = CARTESIAN_POINT ( 'NONE',  ( 62.99999662536839651, -43.30127018922199511, 17.49999999999999645 ) ) ;
#1850 = DIRECTION ( 'NONE',  ( 1.000000000000000000, 0.000000000000000000, 0.000000000000000000 ) ) ;
#1851 = AXIS2_PLACEMENT_3D ( 'NONE', #19848, #31269, #22848 ) ;
#1852 = ORIENTED_EDGE ( 'NONE', *, *, #31081, .T. ) ;
#1853 = DIRECTION ( 'NONE',  ( 0.000000000000000000, 0.000000000000000000, 1.000000000000000000 ) ) ;
#1854 = ADVANCED_BREP_SHAPE_REPRESENTATION ( '', ( #32508, #21385 ), #29775 ) ;
#1855 = DIRECTION ( 'NONE',  ( 0.000000000000000000, 0.000000000000000000, 1.000000000000000000 ) ) ;
#1856 = CARTESIAN_POINT ( 'NONE',  ( -85.00000337463092137, 8.660254037844389075, -5.000000000000000000 ) ) ;
#1857 = VERTEX_POINT ( 'NONE', #12403 ) ;
#1858 = ORIENTED_EDGE ( 'NONE', *, *, #25066, .F. ) ;
#1859 = ORIENTED_EDGE ( 'NONE', *, *, #14978, .F. ) ;
#1860 = DIRECTION ( 'NONE',  ( 1.000000000000000000, 0.000000000000000000, 0.000000000000000000 ) ) ;
#1861 = VERTEX_POINT ( 'NONE', #20657 ) ;
#1862 = DIRECTION ( 'NONE',  ( -1.000000000000000000, 0.000000000000000000, 0.000000000000000000 ) ) ;
#1863 = CARTESIAN_POINT ( 'NONE',  ( -3.374631327851540519E-06, 86.60254037844397601, 12.50000000000000000 ) ) ;
#1864 = CARTESIAN_POINT ( 'NONE',  ( 2.068360682592127020, 4.579334095020458406, -0.01465562841807926259 ) ) ;
#1865 = EDGE_CURVE ( 'NONE', #33610, #4180, #32091, .T. ) ;
#1866 = CARTESIAN_POINT ( 'NONE',  ( -65.00000337463102085, 60.62177826491077326, -5.000000000000000000 ) ) ;
#1867 = FACE_OUTER_BOUND ( 'NONE', #31906, .T. ) ;
#1868 = CARTESIAN_POINT ( 'NONE',  ( -2.449999999999998845, 3.000384657911014384E-16, -0.3851141460153411078 ) ) ;
#1869 = EDGE_CURVE ( 'NONE', #14564, #13541, #16791, .T. ) ;
#1870 = DIRECTION ( 'NONE',  ( -0.5000000000000051070, 1.060575238724903217E-16, -0.8660254037844355990 ) ) ;
#1871 = PLANE ( 'NONE',  #17245 ) ;
#1872 = ORIENTED_EDGE ( 'NONE', *, *, #18822, .T. ) ;
#1873 = EDGE_CURVE ( 'NONE', #17871, #18749, #33578, .T. ) ;
#1874 = ORIENTED_EDGE ( 'NONE', *, *, #2305, .F. ) ;
#1875 = DIRECTION ( 'NONE',  ( 0.000000000000000000, 0.000000000000000000, 1.000000000000000000 ) ) ;
#1876 = CARTESIAN_POINT ( 'NONE',  ( -70.00000337463099243, 51.96152422706637708, 12.50000000000000000 ) ) ;
#1877 = DIRECTION ( 'NONE',  ( 1.000000000000000000, 0.000000000000000000, 0.000000000000000000 ) ) ;
#1878 = CARTESIAN_POINT ( 'NONE',  ( -67.00000337463106348, -60.62177826491083010, -5.000000000000000000 ) ) ;
#1879 = EDGE_CURVE ( 'NONE', #29900, #36497, #18429, .T. ) ;
#1880 = ORIENTED_EDGE ( 'NONE', *, *, #6661, .F. ) ;
#1881 = EDGE_CURVE ( 'NONE', #2266, #18182, #29650, .T. ) ;
#1882 = CARTESIAN_POINT ( 'NONE',  ( -20.00000337463122690, 86.60254037844397601, -5.000000000000000000 ) ) ;
#1883 = CARTESIAN_POINT ( 'NONE',  ( 5.000000000000000000, -1.096207231254244352, -0.7463930790433302986 ) ) ;
#1884 = EDGE_LOOP ( 'NONE', ( #8577, #25517, #19032, #6250 ) ) ;
#1885 = FACE_OUTER_BOUND ( 'NONE', #26315, .T. ) ;
#1886 = ORIENTED_EDGE ( 'NONE', *, *, #1790, .F. ) ;
#1887 = EDGE_CURVE ( 'NONE', #36225, #13221, #24051, .T. ) ;
#1888 = FILL_AREA_STYLE ('',( #4896 ) ) ;
#1889 = DIRECTION ( 'NONE',  ( -1.051347561198064495E-14, -1.000000000000000000, 0.000000000000000000 ) ) ;
#1890 = ADVANCED_FACE ( 'NONE', ( #17026, #2040 ), #27915, .T. ) ;
#1891 = LINE ( 'NONE', #13317, #14018 ) ;
#1892 = EDGE_CURVE ( 'NONE', #20137, #32311, #13852, .T. ) ;
#1893 = AXIS2_PLACEMENT_3D ( 'NONE', #34009, #27796, #1934 ) ;
#1894 = LINE ( 'NONE', #1714, #7701 ) ;
#1895 = ADVANCED_FACE ( 'NONE', ( #7875 ), #13471, .F. ) ;
#1896 = EDGE_LOOP ( 'NONE', ( #31675, #26615, #30467, #15596, #25576, #31376 ) ) ;
#1897 = EDGE_LOOP ( 'NONE', ( #34890, #7758 ) ) ;
#1898 = AXIS2_PLACEMENT_3D ( 'NONE', #15578, #12732, #35077 ) ;
#1899 = CARTESIAN_POINT ( 'NONE',  ( -70.00000337463100664, -17.32050807568882078, -9.999999999999998224 ) ) ;
#1900 = ORIENTED_EDGE ( 'NONE', *, *, #22499, .F. ) ;
#1901 = CARTESIAN_POINT ( 'NONE',  ( 0.3000000000000016542, 0.000000000000000000, 5.000000000000000000 ) ) ;
#1902 = CYLINDRICAL_SURFACE ( 'NONE', #14361, 33.00000000000001421 ) ;
#1903 = CARTESIAN_POINT ( 'NONE',  ( -7.000003374631307729, 77.94228634059957983, -9.999999999999998224 ) ) ;
#1904 = CARTESIAN_POINT ( 'NONE',  ( -31.74999999999995737, 3.673940397442060854E-16, -3.000000000000000888 ) ) ;
#1905 = CARTESIAN_POINT ( 'NONE',  ( -29.97040610772328861, 71.28181329121154874, -5.000000000000000000 ) ) ;
#1906 = ORIENTED_EDGE ( 'NONE', *, *, #11864, .T. ) ;
#1907 = FACE_BOUND ( 'NONE', #19435, .T. ) ;
#1908 = DIRECTION ( 'NONE',  ( 1.000000000000000000, 0.000000000000000000, 0.000000000000000000 ) ) ;
#1909 = DIRECTION ( 'NONE',  ( -0.000000000000000000, -0.000000000000000000, 1.000000000000000000 ) ) ;
#1910 = ORIENTED_EDGE ( 'NONE', *, *, #925, .T. ) ;
#1911 = CARTESIAN_POINT ( 'NONE',  ( 0.000000000000000000, 81.28776890242656350, 37.49999999999985079 ) ) ;
#1912 = CARTESIAN_POINT ( 'NONE',  ( -5.000003374631269537, -77.94228634059960825, -9.999999999999998224 ) ) ;
#1913 = EDGE_CURVE ( 'NONE', #33336, #3159, #606, .T. ) ;
#1914 = ORIENTED_EDGE ( 'NONE', *, *, #21623, .F. ) ;
#1915 = ORIENTED_EDGE ( 'NONE', *, *, #4297, .T. ) ;
#1916 = CARTESIAN_POINT ( 'NONE',  ( -5.000000000000000000, 2.886751345948126879, -6.000000000000000000 ) ) ;
#1917 = CARTESIAN_POINT ( 'NONE',  ( 5.170224855064530445, -2.788471980053870869, -4.289066185948684939 ) ) ;
#1918 = CARTESIAN_POINT ( 'NONE',  ( -107.2777853369584591, -46.05195005975305378, 32.50000000000000000 ) ) ;
#1919 = VERTEX_POINT ( 'NONE', #33740 ) ;
#1920 = EDGE_LOOP ( 'NONE', ( #8732, #36744, #26794, #12307, #11729, #24164, #19809, #10074, #25151, #33826, #24025, #21911, #12744, #33055, #6237, #10358, #21105, #28122, #28960, #16884, #3124, #8179, #36525, #19792, #28859, #18087, #7295, #250, #22492, #26605, #15987, #18220, #231, #15241, #9497 ) ) ;
#1921 = EDGE_LOOP ( 'NONE', ( #6368, #1910 ) ) ;
#1922 = DIRECTION ( 'NONE',  ( 0.000000000000000000, 0.000000000000000000, -1.000000000000000000 ) ) ;
#1923 = ORIENTED_EDGE ( 'NONE', *, *, #30008, .F. ) ;
#1924 = FACE_OUTER_BOUND ( 'NONE', #9242, .T. ) ;
#1925 = EDGE_LOOP ( 'NONE', ( #10034, #14549, #26368, #1432 ) ) ;
#1926 = VERTEX_POINT ( 'NONE', #24935 ) ;
#1927 = CARTESIAN_POINT ( 'NONE',  ( -85.00000337463092137, 8.660254037844389075, -9.999999999999998224 ) ) ;
#1928 = CARTESIAN_POINT ( 'NONE',  ( 19.31922176934805435, 76.99660315353983719, 18.49999999999999645 ) ) ;
#1929 = ADVANCED_FACE ( 'NONE', ( #19138 ), #14221, .T. ) ;
#1930 = ORIENTED_EDGE ( 'NONE', *, *, #25063, .F. ) ;
#1931 = ORIENTED_EDGE ( 'NONE', *, *, #19432, .F. ) ;
#1932 = DIRECTION ( 'NONE',  ( -0.000000000000000000, -0.000000000000000000, -1.000000000000000000 ) ) ;
#1933 = CARTESIAN_POINT ( 'NONE',  ( -8.000003374631281972, 86.60254037844397601, -9.999999999999998224 ) ) ;
#1934 = DIRECTION ( 'NONE',  ( 1.000000000000000000, 0.000000000000000000, 0.000000000000000000 ) ) ;
#1935 = LINE ( 'NONE', #21637, #12460 ) ;
#1936 = ORIENTED_EDGE ( 'NONE', *, *, #27644, .F. ) ;
#1937 = DIRECTION ( 'NONE',  ( 0.000000000000000000, 0.000000000000000000, 1.000000000000000000 ) ) ;
#1938 = AXIS2_PLACEMENT_3D ( 'NONE', #13117, #19130, #30160 ) ;
#1939 = FACE_BOUND ( 'NONE', #20725, .T. ) ;
#1940 = DIRECTION ( 'NONE',  ( 1.000000000000000000, 0.000000000000000000, 0.000000000000000000 ) ) ;
#1941 = CARTESIAN_POINT ( 'NONE',  ( -43.19957991610399972, -47.04203867989563292, 12.49999999999999822 ) ) ;
#1942 = DIRECTION ( 'NONE',  ( -0.000000000000000000, -0.000000000000000000, 1.000000000000000000 ) ) ;
#1943 = DIRECTION ( 'NONE',  ( 0.000000000000000000, 0.000000000000000000, 1.000000000000000000 ) ) ;
#1944 = CARTESIAN_POINT ( 'NONE',  ( 4.999999999999999112, 2.886751345948125991, -5.700000000000000178 ) ) ;
#1945 = CARTESIAN_POINT ( 'NONE',  ( 35.99999999999999289, 2.994873747314852478E-16, -2.445500000000000007 ) ) ;
#1946 = VERTEX_POINT ( 'NONE', #36374 ) ;
#1947 = LINE ( 'NONE', #30460, #25008 ) ;
#1948 = PLANE ( 'NONE',  #15930 ) ;
#1949 = CARTESIAN_POINT ( 'NONE',  ( -78.00000337463096400, -34.64101615137762025, -9.999999999999998224 ) ) ;
#1950 = EDGE_CURVE ( 'NONE', #13345, #8665, #9606, .T. ) ;
#1951 = EDGE_CURVE ( 'NONE', #1659, #19499, #14122, .T. ) ;
#1952 = VERTEX_POINT ( 'NONE', #25297 ) ;
#1953 = AXIS2_PLACEMENT_3D ( 'NONE', #1354, #33045, #1184 ) ;
#1954 = ORIENTED_EDGE ( 'NONE', *, *, #10337, .T. ) ;
#1955 = VERTEX_POINT ( 'NONE', #11031 ) ;
#1956 = DIRECTION ( 'NONE',  ( 0.000000000000000000, 0.000000000000000000, 1.000000000000000000 ) ) ;
#1957 = CARTESIAN_POINT ( 'NONE',  ( 0.000000000000000000, 0.000000000000000000, -6.000000000000000000 ) ) ;
#1958 = ADVANCED_FACE ( 'NONE', ( #10682 ), #30722, .F. ) ;
#1959 = VERTEX_POINT ( 'NONE', #36563 ) ;
#1960 = CARTESIAN_POINT ( 'NONE',  ( 67.99999662536839651, 51.96152422706640550, 12.50000000000000000 ) ) ;
#1961 = EDGE_CURVE ( 'NONE', #22389, #3923, #34473, .T. ) ;
#1962 = AXIS2_PLACEMENT_3D ( 'NONE', #32236, #34705, #9006 ) ;
#1963 = DIRECTION ( 'NONE',  ( 0.000000000000000000, 0.000000000000000000, 1.000000000000000000 ) ) ;
#1964 = ORIENTED_EDGE ( 'NONE', *, *, #11063, .T. ) ;
#1965 = CIRCLE ( 'NONE', #30706, 2.000000000000001776 ) ;
#1966 = CYLINDRICAL_SURFACE ( 'NONE', #19181, 2.000000000000001776 ) ;
#1967 = EDGE_LOOP ( 'NONE', ( #24734, #28848 ) ) ;
#1968 = DIRECTION ( 'NONE',  ( 0.000000000000000000, 0.000000000000000000, 1.000000000000000000 ) ) ;
#1969 = DIRECTION ( 'NONE',  ( 1.000000000000000000, 0.000000000000000000, 0.000000000000000000 ) ) ;
#1970 = CARTESIAN_POINT ( 'NONE',  ( 3.060208875726632805, -4.280211771583998903, -4.057749648769106265 ) ) ;
#1971 = CARTESIAN_POINT ( 'NONE',  ( -95.00000000000000000, 0.000000000000000000, 12.49999999999999822 ) ) ;
#1972 = ADVANCED_FACE ( 'NONE', ( #8779 ), #526, .F. ) ;
#1973 = ORIENTED_EDGE ( 'NONE', *, *, #6672, .F. ) ;
#1974 = CARTESIAN_POINT ( 'NONE',  ( 0.000000000000000000, 0.000000000000000000, 0.000000000000000000 ) ) ;
#1975 = ITEM_DEFINED_TRANSFORMATION ( 'NONE', 'NONE', #23743,  #21385 ) ;
#1976 = CYLINDRICAL_SURFACE ( 'NONE', #2114, 2.000000000000001776 ) ;
#1977 = LINE ( 'NONE', #2167, #12153 ) ;
#1978 = AXIS2_PLACEMENT_3D ( 'NONE', #31503, #11620, #5845 ) ;
#1979 = ORIENTED_EDGE ( 'NONE', *, *, #12058, .F. ) ;
#1980 = LINE ( 'NONE', #13054, #7198 ) ;
#1981 = DIRECTION ( 'NONE',  ( 0.000000000000000000, 0.000000000000000000, 1.000000000000000000 ) ) ;
#1982 = ORIENTED_EDGE ( 'NONE', *, *, #20359, .F. ) ;
#1983 = DIRECTION ( 'NONE',  ( 0.8191520442889890230, 1.003171929053521295E-16, -0.5735764363510501562 ) ) ;
#1984 = PLANE ( 'NONE',  #28039 ) ;
#1985 = CARTESIAN_POINT ( 'NONE',  ( -27.00000337463120914, 77.94228634059957983, -9.999999999999998224 ) ) ;
#1986 = EDGE_LOOP ( 'NONE', ( #6166, #34350 ) ) ;
#1987 = AXIS2_PLACEMENT_3D ( 'NONE', #4028, #35719, #9658 ) ;
#1988 = EDGE_CURVE ( 'NONE', #32887, #4892, #14714, .T. ) ;
#1989 = ORIENTED_EDGE ( 'NONE', *, *, #35364, .F. ) ;
#1990 = DIRECTION ( 'NONE',  ( -1.000000000000000000, 0.000000000000000000, -0.000000000000000000 ) ) ;
#1991 = CARTESIAN_POINT ( 'NONE',  ( -75.00000337463100664, -43.30127018922202353, 17.49999999999999645 ) ) ;
#1992 = CARTESIAN_POINT ( 'NONE',  ( -111.8061974404900241, -19.22934205794863516, 27.50000000000000000 ) ) ;
#1993 = EDGE_LOOP ( 'NONE', ( #30566, #3036, #34482, #12581 ) ) ;
#1994 = EDGE_LOOP ( 'NONE', ( #28535, #32707 ) ) ;
#1995 = PRODUCT_DEFINITION ( 'UNKNOWN', '', #20147, #30919 ) ;
#1996 = DIRECTION ( 'NONE',  ( -1.000000000000000000, 0.000000000000000000, 0.000000000000000000 ) ) ;
#1997 = CARTESIAN_POINT ( 'NONE',  ( -1.552113441248129000, 4.877389578778817736, -0.7348938709837885552 ) ) ;
#1998 = EDGE_CURVE ( 'NONE', #114, #35512, #32055, .T. ) ;
#1999 = CARTESIAN_POINT ( 'NONE',  ( 5.750000000000000000, 89.94802294027094547, -24.99999999999999645 ) ) ;
#2000 = AXIS2_PLACEMENT_3D ( 'NONE', #11669, #31369, #22945 ) ;
#2001 = DIRECTION ( 'NONE',  ( 0.000000000000000000, 0.000000000000000000, 1.000000000000000000 ) ) ;
#2002 = VERTEX_POINT ( 'NONE', #23408 ) ;
#2003 = ORIENTED_EDGE ( 'NONE', *, *, #17646, .T. ) ;
#2004 = AXIS2_PLACEMENT_3D ( 'NONE', #18333, #33131, #12878 ) ;
#2005 = DIRECTION ( 'NONE',  ( -1.000000000000000000, 0.000000000000000000, 0.000000000000000000 ) ) ;
#2006 = EDGE_CURVE ( 'NONE', #23321, #6715, #20562, .T. ) ;
#2007 = DIRECTION ( 'NONE',  ( 1.000000000000000000, 0.000000000000000000, 0.000000000000000000 ) ) ;
#2008 = ORIENTED_EDGE ( 'NONE', *, *, #30972, .F. ) ;
#2009 = DIRECTION ( 'NONE',  ( 1.000000000000000000, 0.000000000000000000, -0.000000000000000000 ) ) ;
#2010 = EDGE_LOOP ( 'NONE', ( #24036, #35965 ) ) ;
#2011 = CARTESIAN_POINT ( 'NONE',  ( 3.000000000000000000, -1.467624384280027172, 2.542000000000001592 ) ) ;
#2012 = AXIS2_PLACEMENT_3D ( 'NONE', #30484, #2659, #25747 ) ;
#2013 = PLANE ( 'NONE',  #17910 ) ;
#2014 = DIRECTION ( 'NONE',  ( 1.000000000000000000, 0.000000000000000000, 0.000000000000000000 ) ) ;
#2015 = ORIENTED_EDGE ( 'NONE', *, *, #33020, .T. ) ;
#2016 = AXIS2_PLACEMENT_3D ( 'NONE', #14169, #25627, #34622 ) ;
#2017 = PRODUCT_DEFINITION_SHAPE ( 'NONE', 'NONE',  #37133 ) ;
#2018 = DIRECTION ( 'NONE',  ( 0.000000000000000000, -0.8660254037844420383, -0.4999999999999945599 ) ) ;
#2019 = EDGE_CURVE ( 'NONE', #12329, #33284, #26215, .T. ) ;
#2020 = CARTESIAN_POINT ( 'NONE',  ( -52.39915983220772233, -35.19434990244957362, -4.999999999999997335 ) ) ;
#2021 = CARTESIAN_POINT ( 'NONE',  ( 3.000000000000000000, -1.467624384280027172, 2.542000000000001592 ) ) ;
#2022 = EDGE_LOOP ( 'NONE', ( #21195, #20127, #11544, #36205 ) ) ;
#2023 = DIRECTION ( 'NONE',  ( 0.000000000000000000, 0.000000000000000000, -1.000000000000000000 ) ) ;
#2024 = DIRECTION ( 'NONE',  ( 0.000000000000000000, 0.000000000000000000, 1.000000000000000000 ) ) ;
#2025 = CARTESIAN_POINT ( 'NONE',  ( 72.72667006429044534, -101.6652913307183610, 32.50000000000000000 ) ) ;
#2026 = VERTEX_POINT ( 'NONE', #15136 ) ;
#2027 = EDGE_CURVE ( 'NONE', #25889, #26458, #28653, .T. ) ;
#2028 = VERTEX_POINT ( 'NONE', #11954 ) ;
#2029 = CIRCLE ( 'NONE', #11590, 2.000000000000001776 ) ;
#2030 = ORIENTED_EDGE ( 'NONE', *, *, #27739, .F. ) ;
#2031 = ADVANCED_FACE ( 'NONE', ( #34470 ), #14967, .F. ) ;
#2032 = DIRECTION ( 'NONE',  ( 1.000000000000000000, 0.000000000000000000, 0.000000000000000000 ) ) ;
#2033 = EDGE_LOOP ( 'NONE', ( #19508, #14993, #29571, #36394 ) ) ;
#2034 = FACE_OUTER_BOUND ( 'NONE', #21873, .T. ) ;
#2035 = CARTESIAN_POINT ( 'NONE',  ( 51.99999662536847467, -69.28203230275519786, -9.999999999999998224 ) ) ;
#2036 = CYLINDRICAL_SURFACE ( 'NONE', #2448, 2.000000000000001776 ) ;
#2037 = AXIS2_PLACEMENT_3D ( 'NONE', #21970, #35864, #33606 ) ;
#2038 = CARTESIAN_POINT ( 'NONE',  ( -35.00000337463116296, 60.62177826491077326, -9.999999999999998224 ) ) ;
#2039 = LINE ( 'NONE', #15744, #1116 ) ;
#2040 = FACE_OUTER_BOUND ( 'NONE', #9470, .T. ) ;
#2041 = DIRECTION ( 'NONE',  ( 0.000000000000000000, 0.000000000000000000, 1.000000000000000000 ) ) ;
#2042 = DIRECTION ( 'NONE',  ( 0.000000000000000000, 0.000000000000000000, 1.000000000000000000 ) ) ;
#2043 = ORIENTED_EDGE ( 'NONE', *, *, #25784, .F. ) ;
#2044 = ORIENTED_EDGE ( 'NONE', *, *, #19742, .F. ) ;
#2045 = EDGE_CURVE ( 'NONE', #9593, #30829, #2134, .T. ) ;
#2046 = CARTESIAN_POINT ( 'NONE',  ( 71.99999662536838230, -34.64101615137759183, -9.999999999999998224 ) ) ;
#2047 = CARTESIAN_POINT ( 'NONE',  ( -35.00000337463116296, 77.94228634059957983, -9.999999999999998224 ) ) ;
#2048 = CARTESIAN_POINT ( 'NONE',  ( 44.99999662536849598, -77.94228634059960825, 17.49999999999999645 ) ) ;
#2049 = VERTEX_POINT ( 'NONE', #139 ) ;
#2050 = DIRECTION ( 'NONE',  ( 0.000000000000000000, 0.000000000000000000, 1.000000000000000000 ) ) ;
#2051 = CIRCLE ( 'NONE', #23596, 45.00000000000000000 ) ;
#2052 = DIRECTION ( 'NONE',  ( 1.000000000000000000, 0.000000000000000000, 0.000000000000000000 ) ) ;
#2053 = VERTEX_POINT ( 'NONE', #29200 ) ;
#2054 = DIRECTION ( 'NONE',  ( 0.000000000000000000, 0.000000000000000000, 1.000000000000000000 ) ) ;
#2055 = VERTEX_POINT ( 'NONE', #26402 ) ;
#2056 = DIRECTION ( 'NONE',  ( 1.000000000000000000, 0.000000000000000000, 0.000000000000000000 ) ) ;
#2057 = AXIS2_PLACEMENT_3D ( 'NONE', #4110, #12703, #4471 ) ;
#2058 = AXIS2_PLACEMENT_3D ( 'NONE', #23236, #20239, #31827 ) ;
#2059 = CARTESIAN_POINT ( 'NONE',  ( 72.99999662536835388, -43.30127018922199511, -5.000000000000000000 ) ) ;
#2060 = EDGE_CURVE ( 'NONE', #30710, #7161, #18298, .T. ) ;
#2061 = AXIS2_PLACEMENT_3D ( 'NONE', #29994, #36007, #10300 ) ;
#2062 = DIRECTION ( 'NONE',  ( 0.000000000000000000, 0.000000000000000000, -1.000000000000000000 ) ) ;
#2063 = ORIENTED_EDGE ( 'NONE', *, *, #18585, .F. ) ;
#2064 = EDGE_CURVE ( 'NONE', #20328, #26329, #9919, .T. ) ;
#2065 = ORIENTED_EDGE ( 'NONE', *, *, #4297, .F. ) ;
#2066 = ADVANCED_FACE ( 'NONE', ( #20396 ), #20024, .T. ) ;
#2067 = EDGE_LOOP ( 'NONE', ( #25119, #14983, #24161 ) ) ;
#2069 = DIRECTION ( 'NONE',  ( 1.000000000000000000, 0.000000000000000000, 0.000000000000000000 ) ) ;
#2068 = AXIS2_PLACEMENT_3D ( 'NONE', #32426, #29601, #1681 ) ;
#2070 = CARTESIAN_POINT ( 'NONE',  ( 23.49154088336464952, -103.5526315789473699, 32.50002500000000083 ) ) ;
#2071 = AXIS2_PLACEMENT_3D ( 'NONE', #35052, #22883, #6173 ) ;
#2072 = EDGE_CURVE ( 'NONE', #23588, #15633, #12303, .T. ) ;
#2073 = CARTESIAN_POINT ( 'NONE',  ( -10.00000337463125000, -86.60254037844400443, -9.999999999999998224 ) ) ;
#2074 = DIRECTION ( 'NONE',  ( -0.000000000000000000, -0.000000000000000000, 1.000000000000000000 ) ) ;
#2075 = FACE_OUTER_BOUND ( 'NONE', #18889, .T. ) ;
#2076 = ADVANCED_FACE ( 'NONE', ( #17574 ), #5793, .F. ) ;
#2077 = ORIENTED_EDGE ( 'NONE', *, *, #14938, .T. ) ;
#2078 = DIRECTION ( 'NONE',  ( 1.000000000000000000, 0.000000000000000000, 0.000000000000000000 ) ) ;
#2079 = CIRCLE ( 'NONE', #21836, 2.000000000000001776 ) ;
#2080 = FACE_OUTER_BOUND ( 'NONE', #27709, .T. ) ;
#2081 = DIRECTION ( 'NONE',  ( 0.000000000000000000, 0.000000000000000000, 1.000000000000000000 ) ) ;
#2082 = ORIENTED_EDGE ( 'NONE', *, *, #25421, .T. ) ;
#2083 = LINE ( 'NONE', #27414, #13053 ) ;
#2084 = DIRECTION ( 'NONE',  ( -0.000000000000000000, -0.000000000000000000, 1.000000000000000000 ) ) ;
#2085 = EDGE_CURVE ( 'NONE', #19856, #15010, #11705, .T. ) ;
#2086 = AXIS2_PLACEMENT_3D ( 'NONE', #11199, #10843, #19459 ) ;
#2087 = ORIENTED_EDGE ( 'NONE', *, *, #21136, .T. ) ;
#2088 = EDGE_CURVE ( 'NONE', #26833, #15434, #35682, .T. ) ;
#2089 = VERTEX_POINT ( 'NONE', #26018 ) ;
#2090 = DIRECTION ( 'NONE',  ( 1.000000000000000000, 0.000000000000000000, 0.000000000000000000 ) ) ;
#2091 = EDGE_CURVE ( 'NONE', #33082, #32864, #33294, .T. ) ;
#2092 = ADVANCED_FACE ( 'NONE', ( #33123 ), #7443, .F. ) ;
#2093 = CARTESIAN_POINT ( 'NONE',  ( -82.27241335952211898, -47.49999999999924682, 27.50000000000000000 ) ) ;
#2094 = EDGE_CURVE ( 'NONE', #27785, #30348, #7546, .T. ) ;
#2095 = CARTESIAN_POINT ( 'NONE',  ( 69.99999662536839651, 17.32050807568879236, 17.49999999999999645 ) ) ;
#2096 = EDGE_LOOP ( 'NONE', ( #27715, #24224, #28476, #9643 ) ) ;
#2097 = ORIENTED_EDGE ( 'NONE', *, *, #13664, .F. ) ;
#2098 = DIRECTION ( 'NONE',  ( 0.000000000000000000, 0.000000000000000000, -1.000000000000000000 ) ) ;
#2099 = CIRCLE ( 'NONE', #31993, 2.000000000000000000 ) ;
#2100 = VERTEX_POINT ( 'NONE', #886 ) ;
#2101 = CONICAL_SURFACE ( 'NONE', #24235, 2.445500000000000007, 0.7853981633974749244 ) ;
#2102 = FACE_BOUND ( 'NONE', #27319, .T. ) ;
#2103 = ORIENTED_EDGE ( 'NONE', *, *, #20963, .T. ) ;
#2104 = AXIS2_PLACEMENT_3D ( 'NONE', #2399, #16446, #36696 ) ;
#2105 = ORIENTED_EDGE ( 'NONE', *, *, #29918, .T. ) ;
#2106 = CIRCLE ( 'NONE', #5114, 2.000000000000001776 ) ;
#2107 = CYLINDRICAL_SURFACE ( 'NONE', #27997, 27.00000000000001421 ) ;
#2108 = DIRECTION ( 'NONE',  ( 0.000000000000000000, 0.000000000000000000, 1.000000000000000000 ) ) ;
#2109 = ORIENTED_EDGE ( 'NONE', *, *, #26290, .T. ) ;
#2110 = ORIENTED_EDGE ( 'NONE', *, *, #799, .F. ) ;
#2111 = FACE_OUTER_BOUND ( 'NONE', #35952, .T. ) ;
#2112 = CIRCLE ( 'NONE', #14688, 1.999999999999998224 ) ;
#2113 = LINE ( 'NONE', #10758, #18957 ) ;
#2114 = AXIS2_PLACEMENT_3D ( 'NONE', #13605, #30833, #5539 ) ;
#2115 = CARTESIAN_POINT ( 'NONE',  ( -47.00000337463112743, -60.62177826491080168, -9.999999999999998224 ) ) ;
#2116 = AXIS2_PLACEMENT_3D ( 'NONE', #1276, #15536, #34179 ) ;
#2117 = DIRECTION ( 'NONE',  ( -1.000000000000000000, 0.000000000000000000, 0.000000000000000000 ) ) ;
#2118 = EDGE_LOOP ( 'NONE', ( #28713, #23285, #17247, #29365 ) ) ;
#2119 = CARTESIAN_POINT ( 'NONE',  ( 0.000000000000000000, 0.000000000000000000, 27.50000000000000000 ) ) ;
#2120 = FACE_BOUND ( 'NONE', #34435, .T. ) ;
#2121 = CARTESIAN_POINT ( 'NONE',  ( 6.249999999999998224, 0.000000000000000000, 0.000000000000000000 ) ) ;
#2122 = CARTESIAN_POINT ( 'NONE',  ( 47.04203867989577503, -43.19957991610382919, 12.49999999999999822 ) ) ;
#2123 = FACE_OUTER_BOUND ( 'NONE', #19915, .T. ) ;
#2124 = CARTESIAN_POINT ( 'NONE',  ( -70.00000337463099243, 34.64101615137758472, -9.999999999999998224 ) ) ;
#2125 = CARTESIAN_POINT ( 'NONE',  ( 29.99999662536857770, -69.28203230275519786, 12.50000000000000000 ) ) ;
#2126 = CIRCLE ( 'NONE', #33260, 30.00000000000001421 ) ;
#2127 = LINE ( 'NONE', #13767, #11576 ) ;
#2128 = EDGE_CURVE ( 'NONE', #8511, #6351, #19510, .T. ) ;
#2129 = ORIENTED_EDGE ( 'NONE', *, *, #31840, .F. ) ;
#2131 = AXIS2_PLACEMENT_3D ( 'NONE', #33816, #5677, #19380 ) ;
#2130 = FACE_OUTER_BOUND ( 'NONE', #32941, .T. ) ;
#2132 = DIRECTION ( 'NONE',  ( 0.000000000000000000, 0.000000000000000000, 1.000000000000000000 ) ) ;
#2133 = CARTESIAN_POINT ( 'NONE',  ( 0.000000000000000000, 0.000000000000000000, 27.50000000000000000 ) ) ;
#2134 = CIRCLE ( 'NONE', #29070, 27.00000000000001421 ) ;
#2135 = AXIS2_PLACEMENT_3D ( 'NONE', #29869, #17883, #35337 ) ;
#2136 = CIRCLE ( 'NONE', #31455, 2.000000000000000000 ) ;
#2137 = ORIENTED_EDGE ( 'NONE', *, *, #34736, .T. ) ;
#2138 = CIRCLE ( 'NONE', #33893, 2.000000000000001776 ) ;
#2139 = EDGE_CURVE ( 'NONE', #28708, #13783, #17130, .T. ) ;
#2140 = ORIENTED_EDGE ( 'NONE', *, *, #5981, .F. ) ;
#2141 = EDGE_LOOP ( 'NONE', ( #82, #30005, #22727, #24066 ) ) ;
#2142 = EDGE_CURVE ( 'NONE', #5127, #11641, #23776, .T. ) ;
#2143 = DIRECTION ( 'NONE',  ( -1.000000000000000000, -0.000000000000000000, -0.000000000000000000 ) ) ;
#2144 = CARTESIAN_POINT ( 'NONE',  ( 34.99999662536853862, 77.94228634059959404, -9.999999999999998224 ) ) ;
#2145 = ORIENTED_EDGE ( 'NONE', *, *, #1881, .T. ) ;
#2146 = CIRCLE ( 'NONE', #23099, 2.000000000000001776 ) ;
#2147 = CARTESIAN_POINT ( 'NONE',  ( 77.99999662536833966, -3.224517592124143893E-15, -5.000000000000000000 ) ) ;
#2148 = DIRECTION ( 'NONE',  ( 0.000000000000000000, 0.000000000000000000, 1.000000000000000000 ) ) ;
#2149 = ORIENTED_EDGE ( 'NONE', *, *, #3807, .F. ) ;
#2150 = DIRECTION ( 'NONE',  ( 1.000000000000000000, 0.000000000000000000, 0.000000000000000000 ) ) ;
#2151 = ORIENTED_EDGE ( 'NONE', *, *, #16537, .T. ) ;
#2152 = CARTESIAN_POINT ( 'NONE',  ( 89.99999662536828282, 0.000000000000000000, 12.50000000000000000 ) ) ;
#2153 = AXIS2_PLACEMENT_3D ( 'NONE', #23156, #6817, #9259 ) ;
#2154 = CYLINDRICAL_SURFACE ( 'NONE', #9416, 2.000000000000001776 ) ;
#2155 = DIRECTION ( 'NONE',  ( 0.000000000000000000, 0.000000000000000000, 1.000000000000000000 ) ) ;
#2156 = AXIS2_PLACEMENT_3D ( 'NONE', #16768, #14489, #13760 ) ;
#2157 = CIRCLE ( 'NONE', #15323, 2.000000000000001776 ) ;
#2158 = ORIENTED_EDGE ( 'NONE', *, *, #27351, .F. ) ;
#2159 =( GEOMETRIC_REPRESENTATION_CONTEXT ( 3 ) GLOBAL_UNCERTAINTY_ASSIGNED_CONTEXT ( ( #24947 ) ) GLOBAL_UNIT_ASSIGNED_CONTEXT ( ( #19503, #33946, #720 ) ) REPRESENTATION_CONTEXT ( 'NONE', 'WORKASPACE' ) );
#2160 = FACE_OUTER_BOUND ( 'NONE', #24834, .T. ) ;
#2161 = AXIS2_PLACEMENT_3D ( 'NONE', #15520, #17959, #12680 ) ;
#2162 = ITEM_DEFINED_TRANSFORMATION ( 'NONE', 'NONE', #16569,  #21385 ) ;
#2163 = AXIS2_PLACEMENT_3D ( 'NONE', #18128, #17759, #29196 ) ;
#2164 = EDGE_CURVE ( 'NONE', #32910, #5560, #32664, .T. ) ;
#2165 = CIRCLE ( 'NONE', #18926, 2.000000000000001776 ) ;
#2166 = CARTESIAN_POINT ( 'NONE',  ( 66.00000000000000000, 0.000000000000000000, 2.445500000000000007 ) ) ;
#2167 = CARTESIAN_POINT ( 'NONE',  ( -67.00000337463104927, -25.98076211353322051, -9.999999999999998224 ) ) ;
#2168 = AXIS2_PLACEMENT_3D ( 'NONE', #17752, #23565, #8412 ) ;
#2169 = ORIENTED_EDGE ( 'NONE', *, *, #8510, .T. ) ;
#2170 = DIRECTION ( 'NONE',  ( 0.000000000000000000, 1.000000000000000000, -1.625241993126352989E-15 ) ) ;
#2171 = CARTESIAN_POINT ( 'NONE',  ( 3.000000000000000000, -1.467624384280027172, 2.542000000000001592 ) ) ;
#2172 = VERTEX_POINT ( 'NONE', #35969 ) ;
#2173 = DIRECTION ( 'NONE',  ( 0.000000000000000000, 0.000000000000000000, 1.000000000000000000 ) ) ;
#2174 = DIRECTION ( 'NONE',  ( 0.000000000000000000, 0.000000000000000000, -1.000000000000000000 ) ) ;
#2175 = DIRECTION ( 'NONE',  ( 1.000000000000000000, 0.000000000000000000, 0.000000000000000000 ) ) ;
#2176 = EDGE_CURVE ( 'NONE', #9542, #29900, #16510, .T. ) ;
#2177 = VERTEX_POINT ( 'NONE', #4646 ) ;
#2178 = ORIENTED_EDGE ( 'NONE', *, *, #29139, .T. ) ;
#2179 = LINE ( 'NONE', #36861, #9385 ) ;
#2180 = CARTESIAN_POINT ( 'NONE',  ( -2.775557561562891351E-14, 19.94802294027085310, 27.49999999999999645 ) ) ;
#2181 = AXIS2_PLACEMENT_3D ( 'NONE', #2673, #2879, #25023 ) ;
#2182 = FACE_OUTER_BOUND ( 'NONE', #27550, .T. ) ;
#2183 = EDGE_LOOP ( 'NONE', ( #36867, #15554, #36057, #31956 ) ) ;
#2184 = ORIENTED_EDGE ( 'NONE', *, *, #13444, .F. ) ;
#2185 = CIRCLE ( 'NONE', #27310, 5.000000000000000000 ) ;
#2186 = EDGE_CURVE ( 'NONE', #14320, #21597, #15885, .T. ) ;
#2187 = DIRECTION ( 'NONE',  ( -1.000000000000000000, 0.000000000000000000, 0.000000000000000000 ) ) ;
#2188 = CARTESIAN_POINT ( 'NONE',  ( -38.00000337463113453, -69.28203230275519786, -9.999999999999998224 ) ) ;
#2189 = PRODUCT_DEFINITION_FORMATION_WITH_SPECIFIED_SOURCE ( 'ANY', '', #36694, .NOT_KNOWN. ) ;
#2190 = DIRECTION ( 'NONE',  ( -0.000000000000000000, -0.000000000000000000, 1.000000000000000000 ) ) ;
#2191 = AXIS2_PLACEMENT_3D ( 'NONE', #6241, #3249, #23880 ) ;
#2192 = AXIS2_PLACEMENT_3D ( 'NONE', #9463, #20894, #16562 ) ;
#2193 = CARTESIAN_POINT ( 'NONE',  ( -3.368272016354703968, 101.4480229402710592, 32.49999999999999289 ) ) ;
#2194 = VECTOR ( 'NONE', #12838, 1000.000000000000000 ) ;
#2195 = EDGE_LOOP ( 'NONE', ( #5622, #36339, #21023, #6317 ) ) ;
#2196 = CIRCLE ( 'NONE', #26147, 2.000000000000001776 ) ;
#2197 = ORIENTED_EDGE ( 'NONE', *, *, #18735, .T. ) ;
#2198 = FACE_OUTER_BOUND ( 'NONE', #28753, .T. ) ;
#2199 = AXIS2_PLACEMENT_3D ( 'NONE', #36677, #16425, #22244 ) ;
#2200 = CARTESIAN_POINT ( 'NONE',  ( -20.39230267490738768, 84.64139243425341874, -5.000000000000000000 ) ) ;
#2201 = VERTEX_POINT ( 'NONE', #24139 ) ;
#2202 = DIRECTION ( 'NONE',  ( 0.000000000000000000, 0.000000000000000000, 1.000000000000000000 ) ) ;
#2203 = ORIENTED_EDGE ( 'NONE', *, *, #22583, .F. ) ;
#2204 = FACE_BOUND ( 'NONE', #6962, .T. ) ;
#2205 = CIRCLE ( 'NONE', #23754, 2.000000000000001776 ) ;
#2206 = CARTESIAN_POINT ( 'NONE',  ( -50.00000337463109190, 69.28203230275518365, -9.999999999999998224 ) ) ;
#2207 = ADVANCED_FACE ( 'NONE', ( #24326 ), #10261, .F. ) ;
#2208 = DIRECTION ( 'NONE',  ( -1.000000000000000000, 0.000000000000000000, 0.000000000000000000 ) ) ;
#2209 = ORIENTED_EDGE ( 'NONE', *, *, #20485, .T. ) ;
#2210 = EDGE_CURVE ( 'NONE', #8614, #18736, #24297, .T. ) ;
#2211 = CARTESIAN_POINT ( 'NONE',  ( 67.99999662536838230, -17.32050807568879947, 12.50000000000000000 ) ) ;
#2212 = VECTOR ( 'NONE', #29599, 1000.000000000000000 ) ;
#2213 = CARTESIAN_POINT ( 'NONE',  ( -2.000003374631327713, 86.60254037844397601, -9.999999999999998224 ) ) ;
#2214 = DIRECTION ( 'NONE',  ( 1.000000000000000000, 0.000000000000000000, 0.000000000000000000 ) ) ;
#2215 = CIRCLE ( 'NONE', #13591, 30.00000000000000000 ) ;
#2216 = ORIENTED_EDGE ( 'NONE', *, *, #36204, .T. ) ;
#2217 = CARTESIAN_POINT ( 'NONE',  ( 44.99999662536849598, 60.62177826491077326, 12.50000000000000000 ) ) ;
#2218 = EDGE_CURVE ( 'NONE', #13427, #1092, #31010, .T. ) ;
#2219 = ADVANCED_FACE ( 'NONE', ( #84 ), #813, .T. ) ;
#2220 = CYLINDRICAL_SURFACE ( 'NONE', #20250, 2.000000000000001776 ) ;
#2221 = FACE_OUTER_BOUND ( 'NONE', #3395, .T. ) ;
#2222 = AXIS2_PLACEMENT_3D ( 'NONE', #29319, #32113, #20494 ) ;
#2223 = CIRCLE ( 'NONE', #4616, 2.000000000000001776 ) ;
#2224 = EDGE_LOOP ( 'NONE', ( #6573, #23462 ) ) ;
#2225 = AXIS2_PLACEMENT_3D ( 'NONE', #19870, #5267, #34141 ) ;
#2226 = AXIS2_PLACEMENT_3D ( 'NONE', #13009, #30247, #28002 ) ;
#2227 = ADVANCED_FACE ( 'NONE', ( #29556 ), #18704, .F. ) ;
#2228 = ORIENTED_EDGE ( 'NONE', *, *, #950, .T. ) ;
#2229 = CARTESIAN_POINT ( 'NONE',  ( 39.27785635698568711, -86.50000000000001421, 27.50000000000000000 ) ) ;
#2230 = ORIENTED_EDGE ( 'NONE', *, *, #23922, .T. ) ;
#2231 = CARTESIAN_POINT ( 'NONE',  ( -70.00000337463102085, -51.96152422706641971, -5.000000000000000000 ) ) ;
#2232 = AXIS2_PLACEMENT_3D ( 'NONE', #31970, #17750, #3522 ) ;
#2233 = DIRECTION ( 'NONE',  ( 0.000000000000000000, 0.000000000000000000, 1.000000000000000000 ) ) ;
#2234 = AXIS2_PLACEMENT_3D ( 'NONE', #6999, #18448, #27229 ) ;
#2235 = DIRECTION ( 'NONE',  ( -0.000000000000000000, -0.000000000000000000, -1.000000000000000000 ) ) ;
#2236 = DIRECTION ( 'NONE',  ( 0.000000000000000000, 0.000000000000000000, -1.000000000000000000 ) ) ;
#2237 = DIRECTION ( 'NONE',  ( 0.000000000000000000, 0.000000000000000000, 1.000000000000000000 ) ) ;
#2238 = CARTESIAN_POINT ( 'NONE',  ( 70.80619744048946984, -84.18124734178287838, 32.50000000000000000 ) ) ;
#2239 = CARTESIAN_POINT ( 'NONE',  ( -6.069707180676227632E-15, 5.773502691896268857, -3.984345921091771547 ) ) ;
#2240 = CIRCLE ( 'NONE', #29180, 3.499999999999989342 ) ;
#2241 = CARTESIAN_POINT ( 'NONE',  ( -55.00000337463107059, 43.30127018922197379, -9.999999999999998224 ) ) ;
#2242 = ORIENTED_EDGE ( 'NONE', *, *, #33594, .T. ) ;
#2243 = TOROIDAL_SURFACE ( 'NONE', #11230, 4.700000000000000178, 0.2999999999999999889 ) ;
#2244 = ORIENTED_EDGE ( 'NONE', *, *, #12311, .T. ) ;
#2245 = EDGE_CURVE ( 'NONE', #5952, #8794, #36404, .T. ) ;
#2246 = CARTESIAN_POINT ( 'NONE',  ( -5.000000000000000000, -2.886751345948137981, -5.553418012614792509 ) ) ;
#2247 = DIRECTION ( 'NONE',  ( -1.000000000000000000, 0.000000000000000000, 0.000000000000000000 ) ) ;
#2248 = DIRECTION ( 'NONE',  ( 0.000000000000000000, 0.000000000000000000, 1.000000000000000000 ) ) ;
#2249 = DIRECTION ( 'NONE',  ( 1.000000000000000000, 0.000000000000000000, 0.000000000000000000 ) ) ;
#2250 = ORIENTED_EDGE ( 'NONE', *, *, #306, .T. ) ;
#2251 =( GEOMETRIC_REPRESENTATION_CONTEXT ( 3 ) GLOBAL_UNCERTAINTY_ASSIGNED_CONTEXT ( ( #7697 ) ) GLOBAL_UNIT_ASSIGNED_CONTEXT ( ( #35038, #9343, #35432 ) ) REPRESENTATION_CONTEXT ( 'NONE', 'WORKASPACE' ) );
#2252 = EDGE_CURVE ( 'NONE', #24938, #36272, #5855, .T. ) ;
#2253 = AXIS2_PLACEMENT_3D ( 'NONE', #34288, #17766, #2795 ) ;
#2254 = AXIS2_PLACEMENT_3D ( 'NONE', #33238, #4930, #18452 ) ;
#2255 = CYLINDRICAL_SURFACE ( 'NONE', #8989, 2.000000000000001776 ) ;
#2256 = ORIENTED_EDGE ( 'NONE', *, *, #35923, .T. ) ;
#2257 = EDGE_LOOP ( 'NONE', ( #14402, #32970 ) ) ;
#2258 = EDGE_CURVE ( 'NONE', #20554, #12415, #35201, .T. ) ;
#2259 = CARTESIAN_POINT ( 'NONE',  ( 61.99999662536845335, 34.64101615137759893, -5.000000000000000000 ) ) ;
#2260 = VERTEX_POINT ( 'NONE', #9706 ) ;
#2261 = CARTESIAN_POINT ( 'NONE',  ( 62.99999662536841072, 25.98076211353318854, -9.999999999999998224 ) ) ;
#2262 = DIRECTION ( 'NONE',  ( -1.000000000000000000, 0.000000000000000000, 0.000000000000000000 ) ) ;
#2263 = AXIS2_PLACEMENT_3D ( 'NONE', #11868, #6071, #29112 ) ;
#2264 = DIRECTION ( 'NONE',  ( 0.000000000000000000, 0.000000000000000000, 1.000000000000000000 ) ) ;
#2265 = ORIENTED_EDGE ( 'NONE', *, *, #13282, .T. ) ;
#2266 = VERTEX_POINT ( 'NONE', #30121 ) ;
#2267 = AXIS2_PLACEMENT_3D ( 'NONE', #28414, #22991, #34430 ) ;
#2268 = AXIS2_PLACEMENT_3D ( 'NONE', #6413, #29284, #22929 ) ;
#2269 = ORIENTED_EDGE ( 'NONE', *, *, #12176, .F. ) ;
#2270 = AXIS2_PLACEMENT_3D ( 'NONE', #29545, #11559, #20743 ) ;
#2271 = ADVANCED_FACE ( 'NONE', ( #29754 ), #12868, .F. ) ;
#2272 = AXIS2_PLACEMENT_3D ( 'NONE', #6781, #6424, #17863 ) ;
#2273 = VERTEX_POINT ( 'NONE', #24887 ) ;
#2274 = CARTESIAN_POINT ( 'NONE',  ( 52.99999662536844625, 43.30127018922198801, -9.999999999999998224 ) ) ;
#2275 = CARTESIAN_POINT ( 'NONE',  ( -51.67317684408315870, -68.18636331025710717, 12.50000000000000000 ) ) ;
#2276 = CARTESIAN_POINT ( 'NONE',  ( 2.500000000000002220, -4.330127018922225623, -3.620524600599886345 ) ) ;
#2277 = CARTESIAN_POINT ( 'NONE',  ( -70.00000337463102085, -34.64101615137762025, 12.50000000000000000 ) ) ;
#2278 = CARTESIAN_POINT ( 'NONE',  ( 5.236973622080098423, -1.063218227091886625, -4.059287483237865146 ) ) ;
#2279 = ORIENTED_EDGE ( 'NONE', *, *, #2915, .F. ) ;
#2280 = DIRECTION ( 'NONE',  ( 0.000000000000000000, 0.000000000000000000, 1.000000000000000000 ) ) ;
#2281 = AXIS2_PLACEMENT_3D ( 'NONE', #36376, #7313, #10685 ) ;
#2282 = DIRECTION ( 'NONE',  ( 0.000000000000000000, 0.000000000000000000, 1.000000000000000000 ) ) ;
#2283 = LINE ( 'NONE', #13718, #34971 ) ;
#2284 = VERTEX_POINT ( 'NONE', #25089 ) ;
#2285 = CARTESIAN_POINT ( 'NONE',  ( 51.99999662536847467, 51.96152422706637708, -9.999999999999998224 ) ) ;
#2286 = DIRECTION ( 'NONE',  ( -1.000000000000000000, -0.000000000000000000, -0.000000000000000000 ) ) ;
#2287 = AXIS2_PLACEMENT_3D ( 'NONE', #11204, #36548, #17213 ) ;
#2288 = ORIENTED_EDGE ( 'NONE', *, *, #12048, .F. ) ;
#2289 = EDGE_LOOP ( 'NONE', ( #27948, #25590, #25487, #24034, #12444 ) ) ;
#2290 = EDGE_CURVE ( 'NONE', #36088, #1094, #22627, .T. ) ;
#2291 = CARTESIAN_POINT ( 'NONE',  ( -56.67878100130369035, 27.78182860042797131, 12.49999999999999822 ) ) ;
#2292 = CARTESIAN_POINT ( 'NONE',  ( 35.19434990244975126, -52.39915983220758022, 12.49999999999999822 ) ) ;
#2293 = CARTESIAN_POINT ( 'NONE',  ( -0.1702248550645306668, -5.871782057790580822, -4.289066185948700038 ) ) ;
#2294 = EDGE_CURVE ( 'NONE', #12700, #36472, #17833, .T. ) ;
#2295 = LINE ( 'NONE', #24801, #13171 ) ;
#2296 = ORIENTED_EDGE ( 'NONE', *, *, #19769, .T. ) ;
#2297 = ORIENTED_EDGE ( 'NONE', *, *, #13007, .F. ) ;
#2298 = AXIS2_PLACEMENT_3D ( 'NONE', #15101, #9838, #6839 ) ;
#2299 = VECTOR ( 'NONE', #14443, 1000.000000000000114 ) ;
#2300 = CIRCLE ( 'NONE', #30426, 2.000000000000001776 ) ;
#2301 = EDGE_CURVE ( 'NONE', #19227, #13708, #19035, .T. ) ;
#2302 = CARTESIAN_POINT ( 'NONE',  ( 82.99999662536831124, -8.660254037844397956, 17.49999999999999645 ) ) ;
#2303 = AXIS2_PLACEMENT_3D ( 'NONE', #10897, #19891, #36773 ) ;
#2304 = EDGE_LOOP ( 'NONE', ( #36745, #23293, #34724, #3964 ) ) ;
#2305 = EDGE_CURVE ( 'NONE', #8160, #3797, #2863, .T. ) ;
#2306 = EDGE_CURVE ( 'NONE', #18101, #36107, #1056, .T. ) ;
#2307 = DIRECTION ( 'NONE',  ( 0.000000000000000000, 0.000000000000000000, -1.000000000000000000 ) ) ;
#2308 = ORIENTED_EDGE ( 'NONE', *, *, #5946, .T. ) ;
#2309 = CIRCLE ( 'NONE', #32845, 2.000000000000001776 ) ;
#2310 = VERTEX_POINT ( 'NONE', #10437 ) ;
#2311 = AXIS2_PLACEMENT_3D ( 'NONE', #30995, #16924, #8121 ) ;
#2312 = CARTESIAN_POINT ( 'NONE',  ( -70.00000337463099243, 17.32050807568877460, 12.50000000000000000 ) ) ;
#2313 = FACE_OUTER_BOUND ( 'NONE', #36206, .T. ) ;
#2314 = VERTEX_POINT ( 'NONE', #19819 ) ;
#2315 = ORIENTED_EDGE ( 'NONE', *, *, #25346, .T. ) ;
#2316 = FACE_OUTER_BOUND ( 'NONE', #27302, .T. ) ;
#2317 = CIRCLE ( 'NONE', #18458, 2.000000000000001776 ) ;
#2318 = CARTESIAN_POINT ( 'NONE',  ( -48.00000337463109190, 51.96152422706637708, 12.50000000000000000 ) ) ;
#2319 = EDGE_CURVE ( 'NONE', #34031, #34954, #15436, .T. ) ;
#2320 = DIRECTION ( 'NONE',  ( 1.000000000000000000, 0.000000000000000000, 0.000000000000000000 ) ) ;
#2321 = EDGE_CURVE ( 'NONE', #35319, #3063, #13048, .T. ) ;
#2322 = LINE ( 'NONE', #2670, #35852 ) ;
#2323 = EDGE_CURVE ( 'NONE', #17546, #20171, #32198, .T. ) ;
#2324 = VERTEX_POINT ( 'NONE', #19090 ) ;
#2325 = CARTESIAN_POINT ( 'NONE',  ( -30.00000337463118427, 69.28203230275516944, -9.999999999999998224 ) ) ;
#2326 = AXIS2_PLACEMENT_3D ( 'NONE', #24768, #9598, #21022 ) ;
#2327 = FACE_BOUND ( 'NONE', #35983, .T. ) ;
#2328 = CIRCLE ( 'NONE', #7113, 2.000000000000001776 ) ;
#2329 = FACE_OUTER_BOUND ( 'NONE', #1335, .T. ) ;
#2330 = FACE_BOUND ( 'NONE', #30307, .T. ) ;
#2331 = CARTESIAN_POINT ( 'NONE',  ( 4.279621169095998212, -62.97617850287780072, 12.49999999999999822 ) ) ;
#2332 = CARTESIAN_POINT ( 'NONE',  ( 95.00000000000001421, 0.000000000000000000, -10.00000000000000000 ) ) ;
#2333 = DIRECTION ( 'NONE',  ( 0.000000000000000000, 0.000000000000000000, 1.000000000000000000 ) ) ;
#2334 = CIRCLE ( 'NONE', #16098, 0.2500000000000002220 ) ;
#2335 = AXIS2_PLACEMENT_3D ( 'NONE', #1191, #15236, #29478 ) ;
#2336 = FACE_OUTER_BOUND ( 'NONE', #9314, .T. ) ;
#2337 = ORIENTED_EDGE ( 'NONE', *, *, #17534, .F. ) ;
#2338 = DIRECTION ( 'NONE',  ( 0.000000000000000000, 0.000000000000000000, -1.000000000000000000 ) ) ;
#2339 = DIRECTION ( 'NONE',  ( 0.000000000000000000, 0.000000000000000000, -1.000000000000000000 ) ) ;
#2340 = DIRECTION ( 'NONE',  ( 1.000000000000000000, 0.000000000000000000, 0.000000000000000000 ) ) ;
#2341 = AXIS2_PLACEMENT_3D ( 'NONE', #34131, #36741, #8788 ) ;
#2342 = ORIENTED_EDGE ( 'NONE', *, *, #14576, .F. ) ;
#2343 = CIRCLE ( 'NONE', #34680, 2.000000000000001776 ) ;
#2344 = VERTEX_POINT ( 'NONE', #13256 ) ;
#2345 = ADVANCED_FACE ( 'NONE', ( #30859 ), #13424, .F. ) ;
#2346 = VERTEX_POINT ( 'NONE', #8191 ) ;
#2347 = CARTESIAN_POINT ( 'NONE',  ( -75.00000337463097821, -8.660254037844422825, -5.000000000000000000 ) ) ;
#2348 = DIRECTION ( 'NONE',  ( 1.000000000000000000, 0.000000000000000000, 0.000000000000000000 ) ) ;
#2349 = EDGE_CURVE ( 'NONE', #5579, #28337, #19633, .T. ) ;
#2350 = ORIENTED_EDGE ( 'NONE', *, *, #36591, .F. ) ;
#2351 = CARTESIAN_POINT ( 'NONE',  ( -70.80619744049063513, -84.18124734178186941, 32.50000000000000000 ) ) ;
#2352 = AXIS2_PLACEMENT_3D ( 'NONE', #2770, #20383, #34652 ) ;
#2353 = CARTESIAN_POINT ( 'NONE',  ( 24.99999662536857059, 77.94228634059957983, -9.999999999999998224 ) ) ;
#2354 = VERTEX_POINT ( 'NONE', #2188 ) ;
#2355 = CARTESIAN_POINT ( 'NONE',  ( 37.27962116909601065, -62.97617850287780072, 12.49999999999999822 ) ) ;
#2357 = EDGE_CURVE ( 'NONE', #7889, #2089, #16435, .T. ) ;
#2356 = ORIENTED_EDGE ( 'NONE', *, *, #23989, .T. ) ;
#2358 = VECTOR ( 'NONE', #23598, 1000.000000000000000 ) ;
#2359 = CARTESIAN_POINT ( 'NONE',  ( 15.97563234535730814, -90.60231327712320137, -49.86561046011506448 ) ) ;
#2360 = CARTESIAN_POINT ( 'NONE',  ( 74.30619744049005249, 84.18124734178236679, 32.50000000000000000 ) ) ;
#2361 = DIRECTION ( 'NONE',  ( 0.000000000000000000, 0.000000000000000000, 1.000000000000000000 ) ) ;
#2362 = VECTOR ( 'NONE', #35553, 1000.000000000000000 ) ;
#2363 = VERTEX_POINT ( 'NONE', #7836 ) ;
#2364 = CARTESIAN_POINT ( 'NONE',  ( 124.4080600076931375, 12.15049814296589226, 27.50000000000000000 ) ) ;
#2365 = VECTOR ( 'NONE', #28251, 1000.000000000000000 ) ;
#2366 = EDGE_CURVE ( 'NONE', #3923, #5373, #33322, .T. ) ;
#2367 = DIRECTION ( 'NONE',  ( 0.000000000000000000, 0.000000000000000000, 1.000000000000000000 ) ) ;
#2368 = EDGE_CURVE ( 'NONE', #24370, #17590, #4662, .T. ) ;
#2369 = CARTESIAN_POINT ( 'NONE',  ( 74.99999662536835388, -25.98076211353319565, -9.999999999999998224 ) ) ;
#2370 = CIRCLE ( 'NONE', #36502, 2.000000000000001776 ) ;
#2371 = ADVANCED_FACE ( 'NONE', ( #17540 ), #28613, .F. ) ;
#2372 = VERTEX_POINT ( 'NONE', #14928 ) ;
#2373 = DIRECTION ( 'NONE',  ( 0.000000000000000000, 0.000000000000000000, 1.000000000000000000 ) ) ;
#2374 = DIRECTION ( 'NONE',  ( 1.000000000000000000, 0.000000000000000000, 0.000000000000000000 ) ) ;
#2375 = EDGE_CURVE ( 'NONE', #2372, #1820, #22821, .T. ) ;
#2376 = ORIENTED_EDGE ( 'NONE', *, *, #15078, .F. ) ;
#2377 = AXIS2_PLACEMENT_3D ( 'NONE', #18920, #27554, #1860 ) ;
#2378 = CARTESIAN_POINT ( 'NONE',  ( 69.99999662536838230, -34.64101615137759183, -9.999999999999998224 ) ) ;
#2379 = DIRECTION ( 'NONE',  ( -1.000000000000000000, 0.000000000000000000, 0.000000000000000000 ) ) ;
#2380 = CARTESIAN_POINT ( 'NONE',  ( 4.999996625368676284, -77.94228634059960825, 17.49999999999999645 ) ) ;
#2381 = CARTESIAN_POINT ( 'NONE',  ( -50.00000337463110611, -69.28203230275519786, -9.999999999999998224 ) ) ;
#2382 = AXIS2_PLACEMENT_3D ( 'NONE', #1711, #32836, #7157 ) ;
#2383 = ORIENTED_EDGE ( 'NONE', *, *, #14978, .T. ) ;
#2384 = VECTOR ( 'NONE', #13407, 1000.000000000000000 ) ;
#2385 = ORIENTED_EDGE ( 'NONE', *, *, #9349, .F. ) ;
#2386 = CIRCLE ( 'NONE', #13157, 2.500000000000000444 ) ;
#2387 = CARTESIAN_POINT ( 'NONE',  ( 2.069940739436594068, -4.578421848776002889, -2.348737659441448779E-14 ) ) ;
#2388 = CARTESIAN_POINT ( 'NONE',  ( -13.00000337463126066, 77.94228634059957983, -9.999999999999998224 ) ) ;
#2389 = ORIENTED_EDGE ( 'NONE', *, *, #22724, .F. ) ;
#2390 = ORIENTED_EDGE ( 'NONE', *, *, #26400, .T. ) ;
#2391 = CARTESIAN_POINT ( 'NONE',  ( -70.00000337463102085, -51.96152422706641971, -9.999999999999998224 ) ) ;
#2392 = DIRECTION ( 'NONE',  ( 1.000000000000000000, 0.000000000000000000, 0.000000000000000000 ) ) ;
#2393 = CARTESIAN_POINT ( 'NONE',  ( 52.99999662536844625, 43.30127018922198801, 12.50000000000000000 ) ) ;
#2394 = CIRCLE ( 'NONE', #7180, 2.000000000000001776 ) ;
#2395 = EDGE_CURVE ( 'NONE', #24063, #34902, #11255, .T. ) ;
#2396 = ORIENTED_EDGE ( 'NONE', *, *, #7192, .T. ) ;
#2397 = EDGE_LOOP ( 'NONE', ( #7938, #25080, #6315, #13329 ) ) ;
#2398 = AXIS2_PLACEMENT_3D ( 'NONE', #17153, #19603, #14518 ) ;
#2399 = CARTESIAN_POINT ( 'NONE',  ( 0.000000000000000000, 0.000000000000000000, 15.00000000000000000 ) ) ;
#2400 = VERTEX_POINT ( 'NONE', #109 ) ;
#2401 = AXIS2_PLACEMENT_3D ( 'NONE', #5882, #34567, #28907 ) ;
#2402 = CARTESIAN_POINT ( 'NONE',  ( 54.99999662536844625, 60.62177826491077326, -5.000000000000000000 ) ) ;
#2403 = VERTEX_POINT ( 'NONE', #3120 ) ;
#2405 = AXIS2_PLACEMENT_3D ( 'NONE', #24464, #16022, #21641 ) ;
#2404 = FACE_BOUND ( 'NONE', #33236, .T. ) ;
#2406 = DIRECTION ( 'NONE',  ( 0.000000000000000000, 0.000000000000000000, 1.000000000000000000 ) ) ;
#2407 = VECTOR ( 'NONE', #30394, 1000.000000000000000 ) ;
#2408 = CIRCLE ( 'NONE', #22784, 2.000000000000001776 ) ;
#2409 = ORIENTED_EDGE ( 'NONE', *, *, #19176, .T. ) ;
#2410 = DIRECTION ( 'NONE',  ( 0.000000000000000000, 0.000000000000000000, 1.000000000000000000 ) ) ;
#2411 = CARTESIAN_POINT ( 'NONE',  ( -75.00000337463097821, -8.660254037844422825, -9.999999999999998224 ) ) ;
#2412 = CARTESIAN_POINT ( 'NONE',  ( 56.67878100130369035, -27.78182860042797131, 12.49999999999999822 ) ) ;
#2413 = CARTESIAN_POINT ( 'NONE',  ( -3.374631303565411855E-06, -86.60254037844400443, -9.999999999999998224 ) ) ;
#2414 = EDGE_CURVE ( 'NONE', #2314, #31389, #9440, .T. ) ;
#2415 = ORIENTED_EDGE ( 'NONE', *, *, #25215, .F. ) ;
#2416 = CYLINDRICAL_SURFACE ( 'NONE', #11876, 2.000000000000001776 ) ;
#2417 = DIRECTION ( 'NONE',  ( -1.000000000000000000, 0.000000000000000000, 0.000000000000000000 ) ) ;
#2418 = CARTESIAN_POINT ( 'NONE',  ( 39.99999662536853151, -69.28203230275519786, -9.999999999999998224 ) ) ;
#2419 = AXIS2_PLACEMENT_3D ( 'NONE', #5260, #22139, #15949 ) ;
#2420 = VERTEX_POINT ( 'NONE', #11720 ) ;
#2421 = ORIENTED_EDGE ( 'NONE', *, *, #16207, .F. ) ;
#2422 = VECTOR ( 'NONE', #3576, 1000.000000000000000 ) ;
#2423 = CARTESIAN_POINT ( 'NONE',  ( -89.27079897466126113, 32.49191361593859284, 12.49999999999999822 ) ) ;
#2424 = ORIENTED_EDGE ( 'NONE', *, *, #9001, .T. ) ;
#2425 = CYLINDRICAL_SURFACE ( 'NONE', #4963, 5.999999999999999112 ) ;
#2426 = CIRCLE ( 'NONE', #7217, 2.000000000000001776 ) ;
#2427 = DIRECTION ( 'NONE',  ( 1.000000000000000000, 0.000000000000000000, 0.000000000000000000 ) ) ;
#2428 = DIRECTION ( 'NONE',  ( -0.000000000000000000, 0.000000000000000000, -1.000000000000000000 ) ) ;
#2429 = LINE ( 'NONE', #34119, #26633 ) ;
#2430 = CARTESIAN_POINT ( 'NONE',  ( 95.09707527045419795, -69.00156695264264783, 32.50000000000000000 ) ) ;
#2431 = CARTESIAN_POINT ( 'NONE',  ( 84.99999662536831124, -8.660254037844397956, -9.999999999999998224 ) ) ;
#2432 = DIRECTION ( 'NONE',  ( 0.000000000000000000, 0.000000000000000000, 1.000000000000000000 ) ) ;
#2433 = EDGE_CURVE ( 'NONE', #666, #5093, #11536, .T. ) ;
#2434 = DIRECTION ( 'NONE',  ( 0.000000000000000000, 0.000000000000000000, 1.000000000000000000 ) ) ;
#2435 = EDGE_LOOP ( 'NONE', ( #16819, #36767, #30220, #22143 ) ) ;
#2436 = EDGE_LOOP ( 'NONE', ( #3625, #23425, #29411, #17365 ) ) ;
#2437 = FACE_BOUND ( 'NONE', #33052, .T. ) ;
#2438 = DIRECTION ( 'NONE',  ( -1.000000000000000000, 1.516276816038986019E-14, 0.000000000000000000 ) ) ;
#2439 = CYLINDRICAL_SURFACE ( 'NONE', #3558, 5.750000000000002665 ) ;
#2440 = DIRECTION ( 'NONE',  ( 0.000000000000000000, 0.000000000000000000, 1.000000000000000000 ) ) ;
#2441 = PRODUCT_RELATED_PRODUCT_CATEGORY ( 'part', '', ( #36694 ) ) ;
#2442 = ORIENTED_EDGE ( 'NONE', *, *, #35938, .T. ) ;
#2443 = PRODUCT_DEFINITION_CONTEXT ( 'detailed design', #24048, 'design' ) ;
#2444 = EDGE_CURVE ( 'NONE', #17808, #17256, #28598, .T. ) ;
#2445 = CARTESIAN_POINT ( 'NONE',  ( 71.99999662536839651, -17.32050807568879947, -5.000000000000000000 ) ) ;
#2446 = ORIENTED_EDGE ( 'NONE', *, *, #26140, .F. ) ;
#2447 = VERTEX_POINT ( 'NONE', #20363 ) ;
#2448 = AXIS2_PLACEMENT_3D ( 'NONE', #13467, #24931, #36371 ) ;
#2449 = FACE_OUTER_BOUND ( 'NONE', #11683, .T. ) ;
#2450 = ORIENTED_EDGE ( 'NONE', *, *, #25367, .F. ) ;
#2451 = SHAPE_REPRESENTATION_RELATIONSHIP ( 'NONE' , 'NONE' ,  #6396, #29583 ) ;
#2452 = CARTESIAN_POINT ( 'NONE',  ( 54.99999662536846046, -43.30127018922200222, 17.49999999999999645 ) ) ;
#2453 = DIRECTION ( 'NONE',  ( 0.000000000000000000, 0.000000000000000000, 1.000000000000000000 ) ) ;
#2454 = CARTESIAN_POINT ( 'NONE',  ( -7.041719095097282852E-16, 87.07302294027100231, 27.52035392823936633 ) ) ;
#2455 = EDGE_CURVE ( 'NONE', #27413, #25343, #26217, .T. ) ;
#2456 = ORIENTED_EDGE ( 'NONE', *, *, #19213, .T. ) ;
#2457 = ORIENTED_EDGE ( 'NONE', *, *, #32987, .T. ) ;
#2458 = ORIENTED_EDGE ( 'NONE', *, *, #19080, .T. ) ;
#2459 = ORIENTED_EDGE ( 'NONE', *, *, #28810, .T. ) ;
#2460 = ORIENTED_EDGE ( 'NONE', *, *, #20527, .F. ) ;
#2461 = DIRECTION ( 'NONE',  ( 0.000000000000000000, 0.000000000000000000, 1.000000000000000000 ) ) ;
#2462 = CARTESIAN_POINT ( 'NONE',  ( 17.99999662536858835, 69.28203230275516944, 17.49999999999999645 ) ) ;
#2463 = CARTESIAN_POINT ( 'NONE',  ( -80.00000337463096400, -34.64101615137762025, 12.50000000000000000 ) ) ;
#2464 = CARTESIAN_POINT ( 'NONE',  ( -5.000000000000000888, 2.886751345948107783, -3.984345921091764886 ) ) ;
#2465 = CARTESIAN_POINT ( 'NONE',  ( 5.244723176341855364, 2.047152853917212134, -4.175731492522787747 ) ) ;
#2466 = ORIENTED_EDGE ( 'NONE', *, *, #20204, .T. ) ;
#2467 = CARTESIAN_POINT ( 'NONE',  ( -62.00000337463104927, 51.96152422706639129, -9.999999999999998224 ) ) ;
#2468 = EDGE_CURVE ( 'NONE', #12792, #26170, #32196, .T. ) ;
#2469 = CARTESIAN_POINT ( 'NONE',  ( 59.99999662536845335, 34.64101615137759893, -9.999999999999998224 ) ) ;
#2470 = EDGE_CURVE ( 'NONE', #19796, #2978, #10651, .T. ) ;
#2471 = AXIS2_PLACEMENT_3D ( 'NONE', #8965, #28996, #3328 ) ;
#2472 = CARTESIAN_POINT ( 'NONE',  ( 19.99999662536861678, -69.28203230275519786, -9.999999999999998224 ) ) ;
#2473 = ORIENTED_EDGE ( 'NONE', *, *, #24422, .T. ) ;
#2474 = FACE_OUTER_BOUND ( 'NONE', #32412, .T. ) ;
#2475 = CYLINDRICAL_SURFACE ( 'NONE', #28523, 2.000000000000001776 ) ;
#2476 = ORIENTED_EDGE ( 'NONE', *, *, #20416, .T. ) ;
#2477 = EDGE_LOOP ( 'NONE', ( #15614, #4466 ) ) ;
#2478 = DIRECTION ( 'NONE',  ( -0.000000000000000000, -0.000000000000000000, 1.000000000000000000 ) ) ;
#2479 = CARTESIAN_POINT ( 'NONE',  ( -4.319324222803803792, 3.279739689143194248, -3.838711833383783745 ) ) ;
#2480 = FACE_BOUND ( 'NONE', #36377, .T. ) ;
#2481 = CARTESIAN_POINT ( 'NONE',  ( -107.2742747693529566, -47.50000423952285900, 32.50001250000000397 ) ) ;
#2482 = EDGE_CURVE ( 'NONE', #30643, #32298, #37016, .T. ) ;
#2483 = VERTEX_POINT ( 'NONE', #12079 ) ;
#2484 = EDGE_LOOP ( 'NONE', ( #18047, #14457, #8542, #28271, #14081, #24475, #26306, #6737, #29059, #9151, #32316, #1437, #12204, #12891, #28177, #23491 ) ) ;
#2485 = DIRECTION ( 'NONE',  ( -1.000000000000000000, 0.000000000000000000, 0.000000000000000000 ) ) ;
#2486 = ADVANCED_FACE ( 'NONE', ( #3495 ), #26172, .F. ) ;
#2487 = EDGE_LOOP ( 'NONE', ( #32209, #3344, #1157, #21393 ) ) ;
#2488 = CIRCLE ( 'NONE', #34245, 2.000000000000001776 ) ;
#2489 = CARTESIAN_POINT ( 'NONE',  ( -86.45172111230354517, 31.46585318596159553, 12.49999999999999822 ) ) ;
#2490 = ORIENTED_EDGE ( 'NONE', *, *, #30442, .F. ) ;
#2491 = VERTEX_POINT ( 'NONE', #483 ) ;
#2492 = DIRECTION ( 'NONE',  ( -0.000000000000000000, 0.8660254037844420383, -0.4999999999999945599 ) ) ;
#2493 = CARTESIAN_POINT ( 'NONE',  ( -12.00000337463125000, -86.60254037844400443, -9.999999999999998224 ) ) ;
#2494 = ORIENTED_EDGE ( 'NONE', *, *, #4463, .T. ) ;
#2495 = ORIENTED_EDGE ( 'NONE', *, *, #29664, .F. ) ;
#2496 = CARTESIAN_POINT ( 'NONE',  ( 52.39915983220795681, 35.19434990244919703, -49.22241343995293761 ) ) ;
#2497 = LINE ( 'NONE', #7564, #32093 ) ;
#2498 = DIRECTION ( 'NONE',  ( 0.000000000000000000, 0.000000000000000000, 1.000000000000000000 ) ) ;
#2499 = CARTESIAN_POINT ( 'NONE',  ( 62.99999662536839651, -43.30127018922199511, -9.999999999999998224 ) ) ;
#2500 = ADVANCED_FACE ( 'NONE', ( #26363 ), #5557, .F. ) ;
#2501 = ORIENTED_EDGE ( 'NONE', *, *, #19297, .F. ) ;
#2502 = DIRECTION ( 'NONE',  ( 0.000000000000000000, 0.000000000000000000, 1.000000000000000000 ) ) ;
#2503 = FACE_BOUND ( 'NONE', #7547, .T. ) ;
#2504 = CARTESIAN_POINT ( 'NONE',  ( -72.28378166042018904, -61.53067111003240797, 12.49999999999999822 ) ) ;
#2505 = DIRECTION ( 'NONE',  ( -1.000000000000000000, 0.000000000000000000, 0.000000000000000000 ) ) ;
#2506 = DIRECTION ( 'NONE',  ( -1.000000000000000000, 0.000000000000000000, 0.000000000000000000 ) ) ;
#2507 = CYLINDRICAL_SURFACE ( 'NONE', #11702, 3.000000000000002665 ) ;
#2508 = EDGE_CURVE ( 'NONE', #6746, #22301, #29793, .T. ) ;
#2509 = FACE_OUTER_BOUND ( 'NONE', #29914, .T. ) ;
#2510 = VECTOR ( 'NONE', #7380, 1000.000000000000000 ) ;
#2511 = EDGE_CURVE ( 'NONE', #15438, #20259, #18440, .T. ) ;
#2512 = LINE ( 'NONE', #7579, #2605 ) ;
#2513 = ORIENTED_EDGE ( 'NONE', *, *, #6238, .F. ) ;
#2514 = CARTESIAN_POINT ( 'NONE',  ( 32.99999662536855283, 60.62177826491078747, -9.999999999999998224 ) ) ;
#2515 = VECTOR ( 'NONE', #19728, 1000.000000000000000 ) ;
#2516 = LINE ( 'NONE', #31197, #12942 ) ;
#2517 = DIRECTION ( 'NONE',  ( -0.000000000000000000, -0.000000000000000000, 1.000000000000000000 ) ) ;
#2518 = ORIENTED_EDGE ( 'NONE', *, *, #4874, .T. ) ;
#2519 = ORIENTED_EDGE ( 'NONE', *, *, #13420, .F. ) ;
#2520 = ORIENTED_EDGE ( 'NONE', *, *, #3027, .F. ) ;
#2521 = DIRECTION ( 'NONE',  ( 0.000000000000000000, 0.000000000000000000, 1.000000000000000000 ) ) ;
#2522 = DIRECTION ( 'NONE',  ( 0.000000000000000000, -0.000000000000000000, 1.000000000000000000 ) ) ;
#2523 = ORIENTED_EDGE ( 'NONE', *, *, #6441, .T. ) ;
#2524 = CARTESIAN_POINT ( 'NONE',  ( 14.99999662536859901, 77.94228634059957983, -9.999999999999998224 ) ) ;
#2525 = EDGE_CURVE ( 'NONE', #18182, #17536, #4688, .T. ) ;
#2526 = ORIENTED_EDGE ( 'NONE', *, *, #7869, .F. ) ;
#2527 = DIRECTION ( 'NONE',  ( 1.000000000000000000, 0.000000000000000000, 0.000000000000000000 ) ) ;
#2528 = EDGE_LOOP ( 'NONE', ( #22457, #26208 ) ) ;
#2529 = DIRECTION ( 'NONE',  ( -0.000000000000000000, 0.000000000000000000, -1.000000000000000000 ) ) ;
#2530 = ORIENTED_EDGE ( 'NONE', *, *, #11336, .T. ) ;
#2531 = CARTESIAN_POINT ( 'NONE',  ( 44.99999662536849598, 60.62177826491077326, -9.999999999999998224 ) ) ;
#2532 = DIRECTION ( 'NONE',  ( 0.000000000000000000, 0.000000000000000000, 1.000000000000000000 ) ) ;
#2533 = AXIS2_PLACEMENT_3D ( 'NONE', #35485, #23660, #31889 ) ;
#2534 = ORIENTED_EDGE ( 'NONE', *, *, #28079, .F. ) ;
#2535 = DIRECTION ( 'NONE',  ( 1.000000000000000000, 0.000000000000000000, 0.000000000000000000 ) ) ;
#2536 = ITEM_DEFINED_TRANSFORMATION ( 'NONE', 'NONE', #8771,  #21385 ) ;
#2537 = DIRECTION ( 'NONE',  ( 1.000000000000000000, 0.000000000000000000, 0.000000000000000000 ) ) ;
#2538 = LINE ( 'NONE', #5920, #10414 ) ;
#2539 = EDGE_CURVE ( 'NONE', #2420, #9972, #9101, .T. ) ;
#2540 = VERTEX_POINT ( 'NONE', #10039 ) ;
#2541 = CARTESIAN_POINT ( 'NONE',  ( -70.00000337463099243, -2.428612866367529932E-14, -9.999999999999998224 ) ) ;
#2542 = DIRECTION ( 'NONE',  ( 0.000000000000000000, 0.000000000000000000, 1.000000000000000000 ) ) ;
#2543 = EDGE_LOOP ( 'NONE', ( #6067, #35259 ) ) ;
#2544 = EDGE_CURVE ( 'NONE', #30363, #26529, #11826, .T. ) ;
#2545 = DIRECTION ( 'NONE',  ( 0.000000000000000000, 0.000000000000000000, 1.000000000000000000 ) ) ;
#2546 = CARTESIAN_POINT ( 'NONE',  ( -45.00000337463111322, 60.62177826491077326, -9.999999999999998224 ) ) ;
#2547 = CYLINDRICAL_SURFACE ( 'NONE', #9388, 2.000000000000001776 ) ;
#2548 = DIRECTION ( 'NONE',  ( 1.000000000000000000, 0.000000000000000000, 0.000000000000000000 ) ) ;
#2549 = ADVANCED_FACE ( 'NONE', ( #1590 ), #4041, .F. ) ;
#2550 = AXIS2_PLACEMENT_3D ( 'NONE', #23646, #20453, #1151 ) ;
#2551 = AXIS2_PLACEMENT_3D ( 'NONE', #7357, #27038, #35675 ) ;
#2552 = ORIENTED_EDGE ( 'NONE', *, *, #28307, .T. ) ;
#2553 = VERTEX_POINT ( 'NONE', #3841 ) ;
#2554 = ADVANCED_FACE ( 'NONE', ( #35548 ), #18277, .T. ) ;
#2555 = DIRECTION ( 'NONE',  ( 1.000000000000000000, 0.000000000000000000, 0.000000000000000000 ) ) ;
#2556 = FACE_OUTER_BOUND ( 'NONE', #35426, .T. ) ;
#2557 = EDGE_CURVE ( 'NONE', #25534, #2372, #24485, .T. ) ;
#2558 = ORIENTED_EDGE ( 'NONE', *, *, #23004, .T. ) ;
#2559 = EDGE_LOOP ( 'NONE', ( #23582, #8615, #5048, #3963 ) ) ;
#2560 = CIRCLE ( 'NONE', #10341, 1.999999999999998224 ) ;
#2561 = CARTESIAN_POINT ( 'NONE',  ( -59.29837256189559724, -31.02796211690927564, -4.999999999999997335 ) ) ;
#2562 = CARTESIAN_POINT ( 'NONE',  ( -3.453178355211937944, 3.779809238954856099, -0.7375898304884446199 ) ) ;
#2563 = CARTESIAN_POINT ( 'NONE',  ( -92.00000337463090716, -1.016341149603137227E-14, -9.999999999999998224 ) ) ;
#2564 = EDGE_CURVE ( 'NONE', #16038, #35244, #25061, .T. ) ;
#2565 = ORIENTED_EDGE ( 'NONE', *, *, #26001, .F. ) ;
#2567 = VERTEX_POINT ( 'NONE', #24278 ) ;
#2566 = ADVANCED_FACE ( 'NONE', ( #35925 ), #10231, .F. ) ;
#2568 = DIRECTION ( 'NONE',  ( 0.000000000000000000, 0.000000000000000000, 1.000000000000000000 ) ) ;
#2569 = ADVANCED_FACE ( 'NONE', ( #1402 ), #12824, .F. ) ;
#2570 = CARTESIAN_POINT ( 'NONE',  ( -34.00000000000000000, 103.4105893997321743, 27.50000000000000000 ) ) ;
#2572 = EDGE_CURVE ( 'NONE', #32411, #25244, #497, .T. ) ;
#2571 = ORIENTED_EDGE ( 'NONE', *, *, #21867, .F. ) ;
#2573 = DIRECTION ( 'NONE',  ( 1.000000000000000000, 0.000000000000000000, 0.000000000000000000 ) ) ;
#2574 = ORIENTED_EDGE ( 'NONE', *, *, #8150, .F. ) ;
#2575 = FACE_BOUND ( 'NONE', #2672, .T. ) ;
#2576 = CIRCLE ( 'NONE', #16967, 27.00000000000001421 ) ;
#2577 = CARTESIAN_POINT ( 'NONE',  ( 81.99999662536832545, -17.32050807568879591, 17.49999999999999645 ) ) ;
#2578 = ORIENTED_EDGE ( 'NONE', *, *, #24390, .T. ) ;
#2579 = DIRECTION ( 'NONE',  ( -0.5000000000000041078, -0.8660254037844364872, 0.000000000000000000 ) ) ;
#2580 = FACE_OUTER_BOUND ( 'NONE', #23319, .T. ) ;
#2581 = AXIS2_PLACEMENT_3D ( 'NONE', #3831, #20705, #15829 ) ;
#2582 = CYLINDRICAL_SURFACE ( 'NONE', #11940, 8.500000000000003553 ) ;
#2583 = CARTESIAN_POINT ( 'NONE',  ( 54.99999662536844625, 43.30127018922198801, 12.50000000000000000 ) ) ;
#2584 = ORIENTED_EDGE ( 'NONE', *, *, #20644, .F. ) ;
#2585 = DIRECTION ( 'NONE',  ( 0.000000000000000000, 0.000000000000000000, 1.000000000000000000 ) ) ;
#2586 = DIRECTION ( 'NONE',  ( -0.000000000000000000, -0.000000000000000000, 1.000000000000000000 ) ) ;
#2587 = FACE_OUTER_BOUND ( 'NONE', #8879, .T. ) ;
#2588 = ORIENTED_EDGE ( 'NONE', *, *, #34596, .T. ) ;
#2589 = VERTEX_POINT ( 'NONE', #7233 ) ;
#2590 = ORIENTED_EDGE ( 'NONE', *, *, #3746, .F. ) ;
#2591 = CARTESIAN_POINT ( 'NONE',  ( 3.000000000000000000, 1.467624384280024730, -2.542000000000001592 ) ) ;
#2592 = CIRCLE ( 'NONE', #30123, 2.000000000000001776 ) ;
#2593 = DIRECTION ( 'NONE',  ( -0.4999999999999980571, 0.8660254037844399289, 0.000000000000000000 ) ) ;
#2594 = CIRCLE ( 'NONE', #19381, 27.00000000000001421 ) ;
#2595 = CARTESIAN_POINT ( 'NONE',  ( 66.99999662536841072, 25.98076211353318854, 12.50000000000000000 ) ) ;
#2596 = CARTESIAN_POINT ( 'NONE',  ( -65.00000337463106348, -60.62177826491083010, -9.999999999999998224 ) ) ;
#2597 = CARTESIAN_POINT ( 'NONE',  ( 106.4067760678514958, -40.94775080679610113, 32.50000000000000711 ) ) ;
#2598 = CARTESIAN_POINT ( 'NONE',  ( -99.75141825464123713, -65.47128713877522443, 32.50000000000000000 ) ) ;
#2599 = LINE ( 'NONE', #11032, #1631 ) ;
#2600 = LINE ( 'NONE', #11033, #29215 ) ;
#2601 = ORIENTED_EDGE ( 'NONE', *, *, #32048, .T. ) ;
#2602 = VECTOR ( 'NONE', #10246, 1000.000000000000000 ) ;
#2603 = ORIENTED_EDGE ( 'NONE', *, *, #35793, .F. ) ;
#2604 = CARTESIAN_POINT ( 'NONE',  ( -35.00000337463117717, -77.94228634059963667, -9.999999999999998224 ) ) ;
#2605 = VECTOR ( 'NONE', #4948, 1000.000000000000114 ) ;
#2606 = CYLINDRICAL_SURFACE ( 'NONE', #25353, 6.000000000000005329 ) ;
#2607 = ADVANCED_FACE ( 'NONE', ( #21276 ), #15464, .T. ) ;
#2608 = CARTESIAN_POINT ( 'NONE',  ( -72.77422209630326222, -61.06482292022084835, -5.000000000000000000 ) ) ;
#2609 = DIRECTION ( 'NONE',  ( 1.000000000000000000, 0.000000000000000000, 0.000000000000000000 ) ) ;
#2610 = EDGE_LOOP ( 'NONE', ( #3078, #11977, #36547, #276 ) ) ;
#2611 = AXIS2_PLACEMENT_3D ( 'NONE', #8921, #25425, #22619 ) ;
#2612 = FACE_BOUND ( 'NONE', #23037, .T. ) ;
#2613 = ORIENTED_EDGE ( 'NONE', *, *, #8439, .F. ) ;
#2614 = VERTEX_POINT ( 'NONE', #7042 ) ;
#2615 = DIRECTION ( 'NONE',  ( 1.000000000000000000, 0.000000000000000000, 0.000000000000000000 ) ) ;
#2616 = CIRCLE ( 'NONE', #25961, 2.000000000000001776 ) ;
#2617 = ORIENTED_EDGE ( 'NONE', *, *, #16998, .F. ) ;
#2618 = CARTESIAN_POINT ( 'NONE',  ( -75.00000337463100664, -43.30127018922202353, -5.000000000000000000 ) ) ;
#2619 = VECTOR ( 'NONE', #11370, 1000.000000000000000 ) ;
#2620 = CARTESIAN_POINT ( 'NONE',  ( 0.000000000000000000, 89.94802294027088863, 30.77834620192012594 ) ) ;
#2621 = CARTESIAN_POINT ( 'NONE',  ( 34.00000000000068923, 58.88972745734143643, 12.49999999999999822 ) ) ;
#2622 = ORIENTED_EDGE ( 'NONE', *, *, #35748, .T. ) ;
#2623 = VERTEX_POINT ( 'NONE', #12651 ) ;
#2624 = EDGE_CURVE ( 'NONE', #26555, #28818, #25647, .T. ) ;
#2625 = ORIENTED_EDGE ( 'NONE', *, *, #20397, .F. ) ;
#2626 = EDGE_CURVE ( 'NONE', #34851, #23895, #19062, .T. ) ;
#2627 =( GEOMETRIC_REPRESENTATION_CONTEXT ( 3 ) GLOBAL_UNCERTAINTY_ASSIGNED_CONTEXT ( ( #4325 ) ) GLOBAL_UNIT_ASSIGNED_CONTEXT ( ( #7421, #26546, #3684 ) ) REPRESENTATION_CONTEXT ( 'NONE', 'WORKASPACE' ) );
#2628 = ORIENTED_EDGE ( 'NONE', *, *, #21755, .F. ) ;
#2629 = ORIENTED_EDGE ( 'NONE', *, *, #36873, .F. ) ;
#2630 = DIRECTION ( 'NONE',  ( 0.000000000000000000, 0.000000000000000000, -1.000000000000000000 ) ) ;
#2631 = CARTESIAN_POINT ( 'NONE',  ( -10.00000337463127842, -69.28203230275519786, -9.999999999999998224 ) ) ;
#2632 = DIRECTION ( 'NONE',  ( 0.000000000000000000, 0.000000000000000000, 1.000000000000000000 ) ) ;
#2633 = DIRECTION ( 'NONE',  ( 1.000000000000000000, 0.000000000000000000, 0.000000000000000000 ) ) ;
#2634 = DIRECTION ( 'NONE',  ( -0.000000000000000000, -0.000000000000000000, 1.000000000000000000 ) ) ;
#2635 = ORIENTED_EDGE ( 'NONE', *, *, #31325, .F. ) ;
#2636 = DIRECTION ( 'NONE',  ( 1.000000000000000000, 0.000000000000000000, 0.000000000000000000 ) ) ;
#2637 = CYLINDRICAL_SURFACE ( 'NONE', #22796, 2.000000000000001776 ) ;
#2638 = EDGE_CURVE ( 'NONE', #29503, #29624, #18467, .T. ) ;
#2639 = DIRECTION ( 'NONE',  ( -0.000000000000000000, -0.000000000000000000, -1.000000000000000000 ) ) ;
#2640 = ORIENTED_EDGE ( 'NONE', *, *, #7808, .T. ) ;
#2641 = CARTESIAN_POINT ( 'NONE',  ( 17.99999662536861678, -86.60254037844400443, -9.999999999999998224 ) ) ;
#2642 = FACE_OUTER_BOUND ( 'NONE', #15803, .T. ) ;
#2643 = EDGE_LOOP ( 'NONE', ( #29990, #31165, #7832, #12203 ) ) ;
#2644 = AXIS2_PLACEMENT_3D ( 'NONE', #25344, #19725, #20271 ) ;
#2645 = ORIENTED_EDGE ( 'NONE', *, *, #29562, .T. ) ;
#2646 = PLANE ( 'NONE',  #20611 ) ;
#2647 = FACE_OUTER_BOUND ( 'NONE', #11058, .T. ) ;
#2648 = EDGE_CURVE ( 'NONE', #1959, #34152, #7676, .T. ) ;
#2649 = CARTESIAN_POINT ( 'NONE',  ( 77.93343913441695747, 72.12058696850802164, 32.50002500000000083 ) ) ;
#2650 = DIRECTION ( 'NONE',  ( 1.000000000000000000, 0.000000000000000000, 0.000000000000000000 ) ) ;
#2651 = VERTEX_POINT ( 'NONE', #12465 ) ;
#2652 = ORIENTED_EDGE ( 'NONE', *, *, #14446, .T. ) ;
#2653 = AXIS2_PLACEMENT_3D ( 'NONE', #15028, #26456, #763 ) ;
#2654 = CARTESIAN_POINT ( 'NONE',  ( 94.55012560584674475, -9.234378588654731601, 27.50000000000000000 ) ) ;
#2655 = VERTEX_POINT ( 'NONE', #21095 ) ;
#2656 = DIRECTION ( 'NONE',  ( 0.000000000000000000, 0.000000000000000000, 1.000000000000000000 ) ) ;
#2657 = ORIENTED_EDGE ( 'NONE', *, *, #5667, .F. ) ;
#2658 = CARTESIAN_POINT ( 'NONE',  ( 70.80619744048946984, -84.18124734178287838, 27.50000000000000000 ) ) ;
#2659 = DIRECTION ( 'NONE',  ( 0.000000000000000000, 0.000000000000000000, -1.000000000000000000 ) ) ;
#2660 = DIRECTION ( 'NONE',  ( 0.000000000000000000, 0.000000000000000000, 1.000000000000000000 ) ) ;
#2661 = ADVANCED_FACE ( 'NONE', ( #844 ), #4240, .F. ) ;
#2662 = DIRECTION ( 'NONE',  ( 0.000000000000000000, 0.000000000000000000, -1.000000000000000000 ) ) ;
#2663 = ORIENTED_EDGE ( 'NONE', *, *, #27147, .F. ) ;
#2664 = CIRCLE ( 'NONE', #23622, 2.000000000000001776 ) ;
#2665 = ORIENTED_EDGE ( 'NONE', *, *, #5511, .F. ) ;
#2666 = CARTESIAN_POINT ( 'NONE',  ( 9.999996625368655856, -86.60254037844400443, 12.50000000000000000 ) ) ;
#2667 = DIRECTION ( 'NONE',  ( 1.000000000000000000, 0.000000000000000000, 0.000000000000000000 ) ) ;
#2668 = EDGE_CURVE ( 'NONE', #26530, #21698, #11856, .T. ) ;
#2669 = DIRECTION ( 'NONE',  ( 1.000000000000000000, 0.000000000000000000, 0.000000000000000000 ) ) ;
#2670 = CARTESIAN_POINT ( 'NONE',  ( -48.00000337463110611, -69.28203230275519786, -9.999999999999998224 ) ) ;
#2671 = AXIS2_PLACEMENT_3D ( 'NONE', #5844, #5299, #36976 ) ;
#2672 = EDGE_LOOP ( 'NONE', ( #25843, #32072 ) ) ;
#2673 = CARTESIAN_POINT ( 'NONE',  ( -35.00000337463116296, 77.94228634059957983, 12.50000000000000000 ) ) ;
#2674 = PRODUCT_DEFINITION ( 'UNKNOWN', '', #29130, #14421 ) ;
#2675 = DIRECTION ( 'NONE',  ( 0.000000000000000000, 0.000000000000000000, 1.000000000000000000 ) ) ;
#2676 = EDGE_CURVE ( 'NONE', #31828, #15574, #7788, .T. ) ;
#2677 = DIRECTION ( 'NONE',  ( -1.000000000000000000, 0.000000000000000000, 0.000000000000000000 ) ) ;
#2678 = DIRECTION ( 'NONE',  ( 0.000000000000000000, 0.000000000000000000, -1.000000000000000000 ) ) ;
#2679 = CARTESIAN_POINT ( 'NONE',  ( -47.00000337463112743, -60.62177826491080168, -9.999999999999998224 ) ) ;
#2680 = FACE_OUTER_BOUND ( 'NONE', #35498, .T. ) ;
#2681 = AXIS2_PLACEMENT_3D ( 'NONE', #6004, #6721, #17426 ) ;
#2682 = AXIS2_PLACEMENT_3D ( 'NONE', #8607, #28477, #3553 ) ;
#2683 = CARTESIAN_POINT ( 'NONE',  ( -9.944410904869345202, 118.0778278770615657, 27.49998800000000188 ) ) ;
#2684 = EDGE_CURVE ( 'NONE', #4982, #10511, #23245, .T. ) ;
#2685 = AXIS2_PLACEMENT_3D ( 'NONE', #8365, #25963, #262 ) ;
#2686 = DIRECTION ( 'NONE',  ( -1.000000000000000000, 0.000000000000000000, 0.000000000000000000 ) ) ;
#2687 = VERTEX_POINT ( 'NONE', #16399 ) ;
#2688 = DIRECTION ( 'NONE',  ( -0.000000000000000000, -0.000000000000000000, -1.000000000000000000 ) ) ;
#2689 = CARTESIAN_POINT ( 'NONE',  ( -5.000000000000000888, -1.947799557644010582, -0.2684016432552386311 ) ) ;
#2690 = CYLINDRICAL_SURFACE ( 'NONE', #13192, 3.499999999999996003 ) ;
#2691 = VERTEX_POINT ( 'NONE', #22388 ) ;
#2692 = EDGE_LOOP ( 'NONE', ( #2950, #18707 ) ) ;
#2693 = ORIENTED_EDGE ( 'NONE', *, *, #1222, .F. ) ;
#2694 = CIRCLE ( 'NONE', #12244, 3.000000000000002665 ) ;
#2695 = DIRECTION ( 'NONE',  ( 0.000000000000000000, 0.000000000000000000, -1.000000000000000000 ) ) ;
#2696 = DIRECTION ( 'NONE',  ( 1.000000000000000000, 0.000000000000000000, 0.000000000000000000 ) ) ;
#2697 = AXIS2_PLACEMENT_3D ( 'NONE', #13812, #14164, #5182 ) ;
#2698 = VERTEX_POINT ( 'NONE', #16228 ) ;
#2699 = AXIS2_PLACEMENT_3D ( 'NONE', #17771, #17580, #14584 ) ;
#2700 = DIRECTION ( 'NONE',  ( 0.000000000000000000, 0.000000000000000000, -1.000000000000000000 ) ) ;
#2701 = ADVANCED_FACE ( 'NONE', ( #5355 ), #36653, .F. ) ;
#2702 = ORIENTED_EDGE ( 'NONE', *, *, #10157, .T. ) ;
#2703 = CYLINDRICAL_SURFACE ( 'NONE', #25764, 3.500000000000003109 ) ;
#2704 = EDGE_LOOP ( 'NONE', ( #3407, #26222, #4553, #31576 ) ) ;
#2705 = FACE_OUTER_BOUND ( 'NONE', #36826, .T. ) ;
#2706 = EDGE_LOOP ( 'NONE', ( #16258, #7473, #35621, #6717 ) ) ;
#2707 = AXIS2_PLACEMENT_3D ( 'NONE', #5216, #2018, #20008 ) ;
#2708 = ORIENTED_EDGE ( 'NONE', *, *, #24153, .F. ) ;
#2709 = EDGE_CURVE ( 'NONE', #33855, #4390, #8146, .T. ) ;
#2710 = AXIS2_PLACEMENT_3D ( 'NONE', #3464, #20496, #29321 ) ;
#2711 = DIRECTION ( 'NONE',  ( 0.000000000000000000, 0.000000000000000000, 1.000000000000000000 ) ) ;
#2712 = DIRECTION ( 'NONE',  ( 0.000000000000000000, 0.000000000000000000, -1.000000000000000000 ) ) ;
#2713 = ADVANCED_FACE ( 'NONE', ( #16589 ), #33086, .F. ) ;
#2714 = ORIENTED_EDGE ( 'NONE', *, *, #25915, .T. ) ;
#2715 = DIRECTION ( 'NONE',  ( 0.7071067811865563435, 0.7071067811865388020, 0.000000000000000000 ) ) ;
#2716 = CARTESIAN_POINT ( 'NONE',  ( 3.000000000000000000, 2.935248768560057453, -3.903127820947815962E-15 ) ) ;
#2717 = CARTESIAN_POINT ( 'NONE',  ( 3.000000000000000000, 2.935248768560057453, -3.903127820947815962E-15 ) ) ;
#2718 = AXIS2_PLACEMENT_3D ( 'NONE', #2364, #13801, #11345 ) ;
#2719 = ORIENTED_EDGE ( 'NONE', *, *, #8887, .T. ) ;
#2720 = DIRECTION ( 'NONE',  ( 0.000000000000000000, 0.000000000000000000, 1.000000000000000000 ) ) ;
#2721 = DIRECTION ( 'NONE',  ( 0.000000000000000000, 0.000000000000000000, -1.000000000000000000 ) ) ;
#2722 = VERTEX_POINT ( 'NONE', #10590 ) ;
#2723 = CARTESIAN_POINT ( 'NONE',  ( -53.00000337463106348, 60.62177826491078747, -9.999999999999998224 ) ) ;
#2724 = AXIS2_PLACEMENT_3D ( 'NONE', #7391, #16216, #33460 ) ;
#2725 = CARTESIAN_POINT ( 'NONE',  ( 67.99999662536839651, 51.96152422706640550, 17.49999999999999645 ) ) ;
#2726 = LINE ( 'NONE', #16976, #33360 ) ;
#2727 = AXIS2_PLACEMENT_3D ( 'NONE', #35506, #12421, #9444 ) ;
#2728 = VECTOR ( 'NONE', #33700, 1000.000000000000000 ) ;
#2729 = CARTESIAN_POINT ( 'NONE',  ( 86.99999662536832545, 8.660254037844394404, -9.999999999999998224 ) ) ;
#2730 = PRESENTATION_LAYER_ASSIGNMENT (  '', '', ( #19514 ) ) ;
#2731 = ORIENTED_EDGE ( 'NONE', *, *, #4905, .T. ) ;
#2732 = ADVANCED_FACE ( 'NONE', ( #19230 ), #13584, .F. ) ;
#2733 = AXIS2_PLACEMENT_3D ( 'NONE', #9394, #3598, #23287 ) ;
#2734 = EDGE_LOOP ( 'NONE', ( #28020, #1692 ) ) ;
#2735 = CARTESIAN_POINT ( 'NONE',  ( 0.000000000000000000, 0.000000000000000000, 27.50000000000000000 ) ) ;
#2736 = DIRECTION ( 'NONE',  ( 0.000000000000000000, 0.000000000000000000, 1.000000000000000000 ) ) ;
#2737 = AXIS2_PLACEMENT_3D ( 'NONE', #7617, #13803, #30491 ) ;
#2738 = CIRCLE ( 'NONE', #15310, 3.500000000000003109 ) ;
#2739 = ORIENTED_EDGE ( 'NONE', *, *, #29944, .T. ) ;
#2740 = EDGE_LOOP ( 'NONE', ( #28222, #6960, #21599 ) ) ;
#2741 = DIRECTION ( 'NONE',  ( 1.000000000000000000, 0.000000000000000000, 0.000000000000000000 ) ) ;
#2742 = CARTESIAN_POINT ( 'NONE',  ( -10.00000337463128197, 86.60254037844397601, -9.999999999999998224 ) ) ;
#2743 = CARTESIAN_POINT ( 'NONE',  ( -68.00000337463102085, -51.96152422706641971, -5.000000000000000000 ) ) ;
#2744 = ORIENTED_EDGE ( 'NONE', *, *, #25381, .F. ) ;
#2745 = EDGE_LOOP ( 'NONE', ( #11047, #12714 ) ) ;
#2746 = LINE ( 'NONE', #25640, #9925 ) ;
#2747 = EDGE_CURVE ( 'NONE', #35934, #20160, #25045, .T. ) ;
#2748 = CIRCLE ( 'NONE', #19506, 2.000000000000001776 ) ;
#2749 = DIRECTION ( 'NONE',  ( 1.000000000000000000, 0.000000000000000000, 0.000000000000000000 ) ) ;
#2750 = ORIENTED_EDGE ( 'NONE', *, *, #7367, .F. ) ;
#2751 = EDGE_CURVE ( 'NONE', #2567, #26082, #13667, .T. ) ;
#2752 = CIRCLE ( 'NONE', #31475, 2.000000000000001776 ) ;
#2753 = DIRECTION ( 'NONE',  ( -1.000000000000000000, 0.000000000000000000, 0.000000000000000000 ) ) ;
#2754 = VERTEX_POINT ( 'NONE', #28203 ) ;
#2755 = LINE ( 'NONE', #22830, #30881 ) ;
#2756 = AXIS2_PLACEMENT_3D ( 'NONE', #30561, #19675, #13676 ) ;
#2757 = CIRCLE ( 'NONE', #17132, 2.000000000000001776 ) ;
#2758 = EDGE_CURVE ( 'NONE', #24629, #10920, #12743, .T. ) ;
#2759 = CIRCLE ( 'NONE', #23124, 2.000000000000001776 ) ;
#2760 = CIRCLE ( 'NONE', #36305, 2.000000000000001776 ) ;
#2761 = DIRECTION ( 'NONE',  ( 0.000000000000000000, 0.000000000000000000, 1.000000000000000000 ) ) ;
#2762 = ADVANCED_FACE ( 'NONE', ( #30268 ), #22034, .F. ) ;
#2763 = AXIS2_PLACEMENT_3D ( 'NONE', #13417, #10818, #21870 ) ;
#2764 = ORIENTED_EDGE ( 'NONE', *, *, #2904, .T. ) ;
#2765 = EDGE_CURVE ( 'NONE', #10183, #18228, #28331, .T. ) ;
#2766 = CARTESIAN_POINT ( 'NONE',  ( -37.50000000000000000, 103.4105893997321743, 38.50000000000000711 ) ) ;
#2767 = AXIS2_PLACEMENT_3D ( 'NONE', #1600, #2911, #28576 ) ;
#2768 = CARTESIAN_POINT ( 'NONE',  ( -67.00000337463102085, 43.30127018922198801, 17.49999999999999645 ) ) ;
#2769 = CARTESIAN_POINT ( 'NONE',  ( 86.45172111230354517, -31.46585318596159553, 12.49999999999999822 ) ) ;
#2770 = CARTESIAN_POINT ( 'NONE',  ( 0.000000000000000000, 0.000000000000000000, -5.000000000000000000 ) ) ;
#2771 = ORIENTED_EDGE ( 'NONE', *, *, #17662, .T. ) ;
#2772 = LINE ( 'NONE', #5024, #32218 ) ;
#2773 = DIRECTION ( 'NONE',  ( 0.000000000000000000, 0.000000000000000000, 1.000000000000000000 ) ) ;
#2774 = DIRECTION ( 'NONE',  ( 0.000000000000000000, 0.000000000000000000, -1.000000000000000000 ) ) ;
#2775 = ADVANCED_FACE ( 'NONE', ( #4959 ), #21833, .F. ) ;
#2776 = CIRCLE ( 'NONE', #25526, 3.000000000000006661 ) ;
#2777 = ADVANCED_FACE ( 'NONE', ( #19046 ), #27819, .F. ) ;
#2778 = ORIENTED_EDGE ( 'NONE', *, *, #32946, .T. ) ;
#2779 = EDGE_LOOP ( 'NONE', ( #10001, #7376, #20857, #5494 ) ) ;
#2780 = EDGE_CURVE ( 'NONE', #15508, #36358, #4977, .T. ) ;
#2781 = CIRCLE ( 'NONE', #23737, 2.000000000000001776 ) ;
#2783 = ADVANCED_FACE ( 'NONE', ( #13780 ), #25225, .F. ) ;
#2782 = ORIENTED_EDGE ( 'NONE', *, *, #13290, .T. ) ;
#2784 = AXIS2_PLACEMENT_3D ( 'NONE', #687, #300, #1058 ) ;
#2785 = DIRECTION ( 'NONE',  ( -1.000000000000000000, 0.000000000000000000, 0.000000000000000000 ) ) ;
#2786 = AXIS2_PLACEMENT_3D ( 'NONE', #8512, #5695, #37026 ) ;
#2787 = AXIS2_PLACEMENT_3D ( 'NONE', #19013, #34008, #30619 ) ;
#2788 = AXIS2_PLACEMENT_3D ( 'NONE', #197, #23080, #18393 ) ;
#2789 = AXIS2_PLACEMENT_3D ( 'NONE', #11858, #34927, #20475 ) ;
#2790 = CARTESIAN_POINT ( 'NONE',  ( 78.38501592334911550, 33.46125459406803060, 12.50000000000000000 ) ) ;
#2791 = AXIS2_PLACEMENT_3D ( 'NONE', #20164, #34063, #34615 ) ;
#2792 = CARTESIAN_POINT ( 'NONE',  ( 71.99999662536839651, 34.64101615137758472, -9.999999999999998224 ) ) ;
#2793 = LINE ( 'NONE', #11223, #30457 ) ;
#2794 = DIRECTION ( 'NONE',  ( -0.000000000000000000, -0.000000000000000000, 1.000000000000000000 ) ) ;
#2795 = DIRECTION ( 'NONE',  ( 1.000000000000000000, 0.000000000000000000, 0.000000000000000000 ) ) ;
#2796 = DIRECTION ( 'NONE',  ( 0.000000000000000000, 0.000000000000000000, 1.000000000000000000 ) ) ;
#2797 = EDGE_LOOP ( 'NONE', ( #7959, #33060, #6471, #16756 ) ) ;
#2798 = CIRCLE ( 'NONE', #23164, 33.00000000000001421 ) ;
#2799 = ORIENTED_EDGE ( 'NONE', *, *, #27985, .T. ) ;
#2800 = DIRECTION ( 'NONE',  ( 1.000000000000000000, 0.000000000000000000, 0.000000000000000000 ) ) ;
#2801 = EDGE_CURVE ( 'NONE', #18680, #7314, #7387, .T. ) ;
#2802 = CARTESIAN_POINT ( 'NONE',  ( 66.99999662536841072, -25.98076211353320275, 17.49999999999999645 ) ) ;
#2803 = LINE ( 'NONE', #3675, #25247 ) ;
#2804 = DIRECTION ( 'NONE',  ( 0.000000000000000000, 0.8660254037844380415, -0.5000000000000012212 ) ) ;
#2805 = ORIENTED_EDGE ( 'NONE', *, *, #7890, .T. ) ;
#2806 = AXIS2_PLACEMENT_3D ( 'NONE', #27999, #16764, #28352 ) ;
#2807 = AXIS2_PLACEMENT_3D ( 'NONE', #1863, #15924, #18924 ) ;
#2808 = FACE_BOUND ( 'NONE', #9716, .T. ) ;
#2809 = ORIENTED_EDGE ( 'NONE', *, *, #3813, .T. ) ;
#2810 = EDGE_LOOP ( 'NONE', ( #29669, #1915, #18969, #23575 ) ) ;
#2811 = EDGE_CURVE ( 'NONE', #3797, #26674, #36138, .T. ) ;
#2812 = VERTEX_POINT ( 'NONE', #28581 ) ;
#2813 = CARTESIAN_POINT ( 'NONE',  ( -9.974659986866640793E-15, -5.773502691896262640, -5.553418012614792509 ) ) ;
#2814 = ORIENTED_EDGE ( 'NONE', *, *, #21581, .T. ) ;
#2815 = AXIS2_PLACEMENT_3D ( 'NONE', #33287, #18291, #27280 ) ;
#2816 = CARTESIAN_POINT ( 'NONE',  ( -20.00000337463123756, -86.60254037844400443, -5.000000000000000000 ) ) ;
#2817 = CARTESIAN_POINT ( 'NONE',  ( -82.00000337463094979, 34.64101615137757051, -9.999999999999998224 ) ) ;
#2818 = AXIS2_PLACEMENT_3D ( 'NONE', #7218, #35711, #20701 ) ;
#2819 = CARTESIAN_POINT ( 'NONE',  ( 72.99999662536835388, -25.98076211353319565, -9.999999999999998224 ) ) ;
#2820 = ORIENTED_EDGE ( 'NONE', *, *, #34666, .F. ) ;
#2821 = ORIENTED_EDGE ( 'NONE', *, *, #20519, .T. ) ;
#2822 = ORIENTED_EDGE ( 'NONE', *, *, #34666, .T. ) ;
#2823 = VECTOR ( 'NONE', #33795, 1000.000000000000000 ) ;
#2824 = EDGE_CURVE ( 'NONE', #16319, #10634, #31897, .T. ) ;
#2825 = ORIENTED_EDGE ( 'NONE', *, *, #28978, .T. ) ;
#2826 = ORIENTED_EDGE ( 'NONE', *, *, #22046, .F. ) ;
#2827 = EDGE_CURVE ( 'NONE', #22214, #19789, #29530, .T. ) ;
#2828 = LINE ( 'NONE', #3016, #25423 ) ;
#2829 = EDGE_CURVE ( 'NONE', #953, #23803, #15162, .T. ) ;
#2830 = DIRECTION ( 'NONE',  ( 1.000000000000000000, 0.000000000000000000, 0.000000000000000000 ) ) ;
#2832 = CIRCLE ( 'NONE', #33461, 2.000000000000001776 ) ;
#2831 = CARTESIAN_POINT ( 'NONE',  ( 11.99999662536865763, -69.28203230275519786, 17.49999999999999645 ) ) ;
#2833 = DIRECTION ( 'NONE',  ( 0.000000000000000000, 0.000000000000000000, 1.000000000000000000 ) ) ;
#2834 = CARTESIAN_POINT ( 'NONE',  ( 67.99999662536839651, 51.96152422706640550, -9.999999999999998224 ) ) ;
#2835 = CIRCLE ( 'NONE', #30361, 2.000000000000000000 ) ;
#2836 = EDGE_LOOP ( 'NONE', ( #8618, #2442, #9985, #20484 ) ) ;
#2837 = CARTESIAN_POINT ( 'NONE',  ( 34.46585318596250858, 86.45172111230321832, -49.86348611802629449 ) ) ;
#2838 = CIRCLE ( 'NONE', #9995, 95.00000000000001421 ) ;
#2839 = DIRECTION ( 'NONE',  ( 0.000000000000000000, 0.000000000000000000, 1.000000000000000000 ) ) ;
#2840 = VECTOR ( 'NONE', #31547, 1000.000000000000000 ) ;
#2841 = CARTESIAN_POINT ( 'NONE',  ( -4.279621169095561228, 62.97617850287782915, 12.49999999999999822 ) ) ;
#2842 = VERTEX_POINT ( 'NONE', #5898 ) ;
#2843 = CARTESIAN_POINT ( 'NONE',  ( -28.00000337463119493, -69.28203230275522628, -9.999999999999998224 ) ) ;
#2844 = CIRCLE ( 'NONE', #23992, 2.000000000000001776 ) ;
#2845 = DIRECTION ( 'NONE',  ( 0.000000000000000000, 0.000000000000000000, 1.000000000000000000 ) ) ;
#2846 = CONICAL_SURFACE ( 'NONE', #6416, 4.999999999999997335, 0.9110539511682894664 ) ;
#2847 = ORIENTED_EDGE ( 'NONE', *, *, #326, .F. ) ;
#2848 = CIRCLE ( 'NONE', #20814, 3.499999999999987566 ) ;
#2849 = EDGE_LOOP ( 'NONE', ( #5620, #4658 ) ) ;
#2850 = AXIS2_PLACEMENT_3D ( 'NONE', #4208, #10365, #13354 ) ;
#2851 = DIRECTION ( 'NONE',  ( 0.000000000000000000, 0.000000000000000000, 1.000000000000000000 ) ) ;
#2852 = DIRECTION ( 'NONE',  ( 0.000000000000000000, 0.000000000000000000, 1.000000000000000000 ) ) ;
#2853 = LINE ( 'NONE', #14628, #25274 ) ;
#2854 = DIRECTION ( 'NONE',  ( 0.000000000000000000, 0.000000000000000000, 1.000000000000000000 ) ) ;
#2855 = ORIENTED_EDGE ( 'NONE', *, *, #19948, .T. ) ;
#2856 = VERTEX_POINT ( 'NONE', #23324 ) ;
#2857 = CIRCLE ( 'NONE', #14800, 1.999999999999998224 ) ;
#2858 = ADVANCED_FACE ( 'NONE', ( #31204 ), #19965, .T. ) ;
#2859 = DIRECTION ( 'NONE',  ( -0.000000000000000000, -0.000000000000000000, 1.000000000000000000 ) ) ;
#2860 = DIRECTION ( 'NONE',  ( 1.000000000000000000, 0.000000000000000000, 0.000000000000000000 ) ) ;
#2861 = VECTOR ( 'NONE', #23326, 1000.000000000000000 ) ;
#2862 = ORIENTED_EDGE ( 'NONE', *, *, #24667, .F. ) ;
#2863 = CIRCLE ( 'NONE', #31587, 4.999999999999997335 ) ;
#2864 = CARTESIAN_POINT ( 'NONE',  ( 19.99999662536861678, -69.28203230275519786, 12.50000000000000000 ) ) ;
#2865 = VERTEX_POINT ( 'NONE', #8347 ) ;
#2866 = CIRCLE ( 'NONE', #22613, 27.00000000000000711 ) ;
#2867 = EDGE_LOOP ( 'NONE', ( #31463, #3366, #20490, #19599, #8376 ) ) ;
#2868 = DIRECTION ( 'NONE',  ( 0.000000000000000000, 0.000000000000000000, 1.000000000000000000 ) ) ;
#2869 = DIRECTION ( 'NONE',  ( 0.000000000000000000, 0.000000000000000000, -1.000000000000000000 ) ) ;
#2870 = AXIS2_PLACEMENT_3D ( 'NONE', #4353, #4543, #27767 ) ;
#2871 = FACE_BOUND ( 'NONE', #17915, .T. ) ;
#2872 = ORIENTED_EDGE ( 'NONE', *, *, #5946, .F. ) ;
#2873 = ORIENTED_EDGE ( 'NONE', *, *, #24308, .T. ) ;
#2874 = DIRECTION ( 'NONE',  ( 1.000000000000000000, 0.000000000000000000, 0.000000000000000000 ) ) ;
#2875 = CARTESIAN_POINT ( 'NONE',  ( 31.99999662536856704, 69.28203230275518365, -9.999999999999998224 ) ) ;
#2876 = DIRECTION ( 'NONE',  ( -0.000000000000000000, 0.000000000000000000, -1.000000000000000000 ) ) ;
#2877 = CYLINDRICAL_SURFACE ( 'NONE', #1127, 2.000000000000000000 ) ;
#2878 = VERTEX_POINT ( 'NONE', #3444 ) ;
#2879 = DIRECTION ( 'NONE',  ( 0.000000000000000000, 0.000000000000000000, 1.000000000000000000 ) ) ;
#2880 = EDGE_CURVE ( 'NONE', #13349, #22389, #194, .T. ) ;
#2881 = FACE_BOUND ( 'NONE', #3641, .T. ) ;
#2882 = CARTESIAN_POINT ( 'NONE',  ( -70.00000337463099243, 34.64101615137758472, 12.50000000000000000 ) ) ;
#2883 = CYLINDRICAL_SURFACE ( 'NONE', #27068, 3.000000000000002665 ) ;
#2884 = AXIS2_PLACEMENT_3D ( 'NONE', #29890, #32693, #10016 ) ;
#2885 = CARTESIAN_POINT ( 'NONE',  ( 37.50000000000000000, 103.4105893997321743, 27.50000000000000000 ) ) ;
#2886 = CARTESIAN_POINT ( 'NONE',  ( 0.000000000000000000, 0.000000000000000000, -5.000000000000000000 ) ) ;
#2887 = CYLINDRICAL_SURFACE ( 'NONE', #20958, 2.000000000000001776 ) ;
#2888 = CARTESIAN_POINT ( 'NONE',  ( 4.999999999999999112, 2.886751345948125991, -3.984345921091767551 ) ) ;
#2889 = EDGE_LOOP ( 'NONE', ( #10879, #4992, #27135, #13817, #15532 ) ) ;
#2890 = LINE ( 'NONE', #19580, #10066 ) ;
#2891 = VECTOR ( 'NONE', #27089, 1000.000000000000000 ) ;
#2892 = AXIS2_PLACEMENT_3D ( 'NONE', #35312, #27404, #9607 ) ;
#2893 = DIRECTION ( 'NONE',  ( 1.000000000000000000, 0.000000000000000000, 0.000000000000000000 ) ) ;
#2894 = CARTESIAN_POINT ( 'NONE',  ( 49.99999662536846756, -69.28203230275519786, 17.49999999999999645 ) ) ;
#2895 = CIRCLE ( 'NONE', #20833, 2.000000000000001776 ) ;
#2896 = ORIENTED_EDGE ( 'NONE', *, *, #8998, .F. ) ;
#2897 = EDGE_LOOP ( 'NONE', ( #32096, #34103, #27596, #30792, #11181 ) ) ;
#2898 = ORIENTED_EDGE ( 'NONE', *, *, #28312, .F. ) ;
#2899 = AXIS2_PLACEMENT_3D ( 'NONE', #22721, #22893, #31317 ) ;
#2900 = DIRECTION ( 'NONE',  ( 0.000000000000000000, 0.000000000000000000, 1.000000000000000000 ) ) ;
#2901 = DIRECTION ( 'NONE',  ( -1.000000000000000000, 0.000000000000000000, 0.000000000000000000 ) ) ;
#2902 = CARTESIAN_POINT ( 'NONE',  ( 60.93295298011005201, 19.13981058454729123, 12.49999999999999822 ) ) ;
#2903 = ORIENTED_EDGE ( 'NONE', *, *, #15040, .T. ) ;
#2904 = EDGE_CURVE ( 'NONE', #2026, #29492, #34343, .T. ) ;
#2905 = AXIS2_PLACEMENT_3D ( 'NONE', #19556, #10751, #22355 ) ;
#2906 = CARTESIAN_POINT ( 'NONE',  ( 59.99999662536842493, -51.96152422706639840, -9.999999999999998224 ) ) ;
#2907 = ORIENTED_EDGE ( 'NONE', *, *, #18493, .F. ) ;
#2908 = DIRECTION ( 'NONE',  ( 0.000000000000000000, 0.000000000000000000, 1.000000000000000000 ) ) ;
#2909 = EDGE_CURVE ( 'NONE', #37038, #23091, #21134, .T. ) ;
#2910 = ORIENTED_EDGE ( 'NONE', *, *, #5531, .F. ) ;
#2911 = DIRECTION ( 'NONE',  ( 0.000000000000000000, 0.000000000000000000, 1.000000000000000000 ) ) ;
#2912 = VECTOR ( 'NONE', #17474, 1000.000000000000000 ) ;
#2913 = ORIENTED_EDGE ( 'NONE', *, *, #33665, .T. ) ;
#2914 = ORIENTED_EDGE ( 'NONE', *, *, #4748, .T. ) ;
#2915 = EDGE_CURVE ( 'NONE', #34742, #20792, #18159, .T. ) ;
#2916 = CARTESIAN_POINT ( 'NONE',  ( 44.99999662536849598, 60.62177826491077326, 17.49999999999999645 ) ) ;
#2917 = FACE_OUTER_BOUND ( 'NONE', #31080, .T. ) ;
#2918 = AXIS2_PLACEMENT_3D ( 'NONE', #32451, #18407, #30015 ) ;
#2919 = DIRECTION ( 'NONE',  ( 1.000000000000000000, 0.000000000000000000, 0.000000000000000000 ) ) ;
#2920 = ORIENTED_EDGE ( 'NONE', *, *, #20416, .F. ) ;
#2921 = CARTESIAN_POINT ( 'NONE',  ( 31.83425564451589196, 89.42901512340320380, -49.86348611802629449 ) ) ;
#2922 = CIRCLE ( 'NONE', #23246, 2.000000000000001776 ) ;
#2923 = DIRECTION ( 'NONE',  ( 1.000000000000000000, 0.000000000000000000, 0.000000000000000000 ) ) ;
#2924 = DIRECTION ( 'NONE',  ( -1.000000000000000000, 0.000000000000000000, 0.000000000000000000 ) ) ;
#2925 = VECTOR ( 'NONE', #4879, 1000.000000000000000 ) ;
#2926 = ORIENTED_EDGE ( 'NONE', *, *, #15793, .F. ) ;
#2927 = CARTESIAN_POINT ( 'NONE',  ( 70.80619744049005249, 84.18124734178236679, 27.50000000000000000 ) ) ;
#2928 = DIRECTION ( 'NONE',  ( 1.000000000000000000, 0.000000000000000000, 0.000000000000000000 ) ) ;
#2929 = ORIENTED_EDGE ( 'NONE', *, *, #20759, .T. ) ;
#2930 = EDGE_CURVE ( 'NONE', #34239, #16670, #26318, .T. ) ;
#2931 = CYLINDRICAL_SURFACE ( 'NONE', #37007, 1.999999999999998224 ) ;
#2932 = DIRECTION ( 'NONE',  ( 1.000000000000000000, 0.000000000000000000, 0.000000000000000000 ) ) ;
#2933 = DIRECTION ( 'NONE',  ( 1.000000000000000000, 0.000000000000000000, 0.000000000000000000 ) ) ;
#2934 = AXIS2_PLACEMENT_3D ( 'NONE', #32823, #26625, #18389 ) ;
#2935 = CARTESIAN_POINT ( 'NONE',  ( -78.00000337463094979, 17.32050807568878525, -9.999999999999998224 ) ) ;
#2936 = CIRCLE ( 'NONE', #17882, 2.000000000000001776 ) ;
#2937 = ORIENTED_EDGE ( 'NONE', *, *, #18375, .T. ) ;
#2938 = ORIENTED_EDGE ( 'NONE', *, *, #17116, .T. ) ;
#2939 = DIRECTION ( 'NONE',  ( -1.000000000000000000, -0.000000000000000000, -0.000000000000000000 ) ) ;
#2940 = FACE_OUTER_BOUND ( 'NONE', #24265, .T. ) ;
#2941 = EDGE_CURVE ( 'NONE', #26674, #34191, #1383, .T. ) ;
#2942 = VERTEX_POINT ( 'NONE', #22578 ) ;
#2943 = ORIENTED_EDGE ( 'NONE', *, *, #29143, .F. ) ;
#2944 = AXIS2_PLACEMENT_3D ( 'NONE', #18355, #4294, #4113 ) ;
#2945 = EDGE_CURVE ( 'NONE', #374, #33065, #32532, .T. ) ;
#2946 = DIRECTION ( 'NONE',  ( 0.000000000000000000, 0.000000000000000000, 1.000000000000000000 ) ) ;
#2947 = DIRECTION ( 'NONE',  ( 1.000000000000000000, 0.000000000000000000, 0.000000000000000000 ) ) ;
#2948 = DIRECTION ( 'NONE',  ( 0.000000000000000000, 0.000000000000000000, 1.000000000000000000 ) ) ;
#2949 = EDGE_CURVE ( 'NONE', #9993, #30809, #31328, .T. ) ;
#2950 = ORIENTED_EDGE ( 'NONE', *, *, #29826, .T. ) ;
#2951 = FACE_OUTER_BOUND ( 'NONE', #7690, .T. ) ;
#2952 = ORIENTED_EDGE ( 'NONE', *, *, #16444, .F. ) ;
#2953 = CARTESIAN_POINT ( 'NONE',  ( -43.00331345287344931, -60.50675932581249583, -5.000000000000000000 ) ) ;
#2954 = EDGE_CURVE ( 'NONE', #18222, #5353, #24761, .T. ) ;
#2955 = ORIENTED_EDGE ( 'NONE', *, *, #5766, .F. ) ;
#2956 = CYLINDRICAL_SURFACE ( 'NONE', #17141, 2.000000000000001776 ) ;
#2957 = AXIS2_PLACEMENT_3D ( 'NONE', #2997, #5991, #17417 ) ;
#2958 = EDGE_CURVE ( 'NONE', #29981, #15962, #16358, .T. ) ;
#2959 = LINE ( 'NONE', #36703, #14914 ) ;
#2960 = DIRECTION ( 'NONE',  ( 0.000000000000000000, 0.000000000000000000, 1.000000000000000000 ) ) ;
#2961 = ORIENTED_EDGE ( 'NONE', *, *, #30807, .F. ) ;
#2962 = CARTESIAN_POINT ( 'NONE',  ( 108.3061974404897541, -19.22934205795014861, -26.00000000000000000 ) ) ;
#2963 = DIRECTION ( 'NONE',  ( -1.000000000000000000, 0.000000000000000000, 0.000000000000000000 ) ) ;
#2964 = AXIS2_PLACEMENT_3D ( 'NONE', #5614, #8063, #14045 ) ;
#2965 = CIRCLE ( 'NONE', #32913, 2.000000000000001776 ) ;
#2966 = LINE ( 'NONE', #19460, #28732 ) ;
#2967 = DIRECTION ( 'NONE',  ( 0.000000000000000000, 0.000000000000000000, -1.000000000000000000 ) ) ;
#2968 = ORIENTED_EDGE ( 'NONE', *, *, #873, .F. ) ;
#2969 = DIRECTION ( 'NONE',  ( 0.000000000000000000, 0.000000000000000000, 1.000000000000000000 ) ) ;
#2970 = CIRCLE ( 'NONE', #13721, 2.000000000000001776 ) ;
#2971 = CARTESIAN_POINT ( 'NONE',  ( -48.00000337463109190, 69.28203230275518365, 17.49999999999999645 ) ) ;
#2972 = DIRECTION ( 'NONE',  ( -1.000000000000000000, 0.000000000000000000, 0.000000000000000000 ) ) ;
#2973 = VERTEX_POINT ( 'NONE', #31904 ) ;
#2974 = EDGE_CURVE ( 'NONE', #14063, #14131, #30715, .T. ) ;
#2975 = ORIENTED_EDGE ( 'NONE', *, *, #8019, .F. ) ;
#2976 = B_SPLINE_CURVE_WITH_KNOTS ( 'NONE', 3,
 ( #7325, #30922, #7886, #25147, #13310, #33388, #27384, #1883, #8056, #18951, #24757, #13864, #30737, #1703 ),
 .UNSPECIFIED., .F., .F.,
 ( 4, 2, 2, 2, 2, 2, 4 ),
 ( 0.01481111731982464805, 0.01564725794959783214, 0.01648339857937101624, 0.01690146889425760829, 0.01731953920914420034, 0.01773760952403079239, 0.01815567983891738443 ),
 .UNSPECIFIED. ) ;
#2977 =( REPRESENTATION_RELATIONSHIP ('NONE','NONE', #15268, #22738 ) REPRESENTATION_RELATIONSHIP_WITH_TRANSFORMATION ( #23517 )SHAPE_REPRESENTATION_RELATIONSHIP( ) );
#2978 = VERTEX_POINT ( 'NONE', #14331 ) ;
#2979 = AXIS2_PLACEMENT_3D ( 'NONE', #16101, #4460, #24340 ) ;
#2980 = EDGE_CURVE ( 'NONE', #27460, #32112, #2592, .T. ) ;
#2981 = DIRECTION ( 'NONE',  ( 0.000000000000000000, 0.000000000000000000, 1.000000000000000000 ) ) ;
#2982 = CIRCLE ( 'NONE', #8366, 3.500000000000003109 ) ;
#2983 = CARTESIAN_POINT ( 'NONE',  ( -65.00000337463106348, -60.62177826491083010, 12.50000000000000000 ) ) ;
#2984 = ADVANCED_FACE ( 'NONE', ( #73 ), #237, .F. ) ;
#2985 = CARTESIAN_POINT ( 'NONE',  ( 82.38669124558430212, -72.56045967525361107, 32.50000000000000000 ) ) ;
#2986 = CARTESIAN_POINT ( 'NONE',  ( -14.80603122773056768, 87.83969979969874942, -49.86561046011506448 ) ) ;
#2987 = EDGE_CURVE ( 'NONE', #9972, #36720, #13959, .T. ) ;
#2988 = CARTESIAN_POINT ( 'NONE',  ( 0.000000000000000000, 55.00000000000000000, -10.00000000000000178 ) ) ;
#2989 = CIRCLE ( 'NONE', #31135, 2.000000000000001776 ) ;
#2990 = ORIENTED_EDGE ( 'NONE', *, *, #23402, .T. ) ;
#2991 = ORIENTED_EDGE ( 'NONE', *, *, #28888, .T. ) ;
#2992 = DIRECTION ( 'NONE',  ( 0.000000000000000000, -0.5000000000000011102, -0.8660254037844379305 ) ) ;
#2993 = AXIS2_PLACEMENT_3D ( 'NONE', #459, #94, #2928 ) ;
#2994 = PLANE ( 'NONE',  #29532 ) ;
#2995 = CARTESIAN_POINT ( 'NONE',  ( -90.00000337463090716, -1.040834085586084257E-14, 12.50000000000000000 ) ) ;
#2996 = B_SPLINE_CURVE_WITH_KNOTS ( 'NONE', 3,
 ( #18780, #24974, #16169, #7344, #35659 ),
 .UNSPECIFIED., .F., .F.,
 ( 4, 1, 4 ),
 ( 0.000000000000000000, 0.002886751345948134623, 0.005773502691896269245 ),
 .UNSPECIFIED. ) ;
#2997 = CARTESIAN_POINT ( 'NONE',  ( 27.78182860042856461, 56.67878100130339902, -4.999999999999997335 ) ) ;
#2998 = EDGE_LOOP ( 'NONE', ( #2043, #15950, #27792, #21738 ) ) ;
#2999 = ADVANCED_FACE ( 'NONE', ( #20869 ), #9983, .F. ) ;
#3000 = FACE_BOUND ( 'NONE', #18631, .T. ) ;
#3001 = ORIENTED_EDGE ( 'NONE', *, *, #20598, .F. ) ;
#3002 = VERTEX_POINT ( 'NONE', #4359 ) ;
#3003 = LINE ( 'NONE', #5809, #36811 ) ;
#3004 = ORIENTED_EDGE ( 'NONE', *, *, #249, .F. ) ;
#3005 = SURFACE_STYLE_USAGE ( .BOTH. , #36939 ) ;
#3006 = DIRECTION ( 'NONE',  ( 0.000000000000000000, 0.000000000000000000, 1.000000000000000000 ) ) ;
#3007 = CARTESIAN_POINT ( 'NONE',  ( 101.7384897088151234, 110.2237710830533217, 27.50000000000000000 ) ) ;
#3008 = CIRCLE ( 'NONE', #36531, 2.000000000000001776 ) ;
#3009 = EDGE_LOOP ( 'NONE', ( #33677, #13074 ) ) ;
#3010 = ORIENTED_EDGE ( 'NONE', *, *, #27990, .F. ) ;
#3011 = CIRCLE ( 'NONE', #13205, 2.000000000000001776 ) ;
#3012 = ORIENTED_EDGE ( 'NONE', *, *, #31052, .F. ) ;
#3013 = VERTEX_POINT ( 'NONE', #29862 ) ;
#3014 = ADVANCED_FACE ( 'NONE', ( #26672 ), #23675, .F. ) ;
#3015 = EDGE_LOOP ( 'NONE', ( #9068, #21045 ) ) ;
#3016 = CARTESIAN_POINT ( 'NONE',  ( 82.99999662536831124, -8.660254037844397956, -9.999999999999998224 ) ) ;
#3017 = AXIS2_PLACEMENT_3D ( 'NONE', #29391, #6883, #12114 ) ;
#3018 = CYLINDRICAL_SURFACE ( 'NONE', #17385, 3.000000000000006217 ) ;
#3019 = EDGE_CURVE ( 'NONE', #6052, #11631, #26874, .T. ) ;
#3020 = AXIS2_PLACEMENT_3D ( 'NONE', #10419, #29933, #12849 ) ;
#3021 = DIRECTION ( 'NONE',  ( 1.000000000000000000, 0.000000000000000000, 0.000000000000000000 ) ) ;
#3022 = CARTESIAN_POINT ( 'NONE',  ( -3.499999999999991562, -55.00000000000000000, -10.00000000000000000 ) ) ;
#3023 = DIRECTION ( 'NONE',  ( 1.000000000000000000, 0.000000000000000000, 0.000000000000000000 ) ) ;
#3024 = ORIENTED_EDGE ( 'NONE', *, *, #1396, .T. ) ;
#3025 = DIRECTION ( 'NONE',  ( 0.000000000000000000, -0.8660254037844419273, 0.4999999999999945599 ) ) ;
#3026 =( BOUNDED_SURFACE ( )  B_SPLINE_SURFACE ( 3, 2, ( 
 ( #14412, #141, #11571 ),
 ( #34475, #648, #32327 ),
 ( #32125, #1208, #23519 ),
 ( #12439, #17697, #6645 ),
 ( #12628, #29137, #4216 ),
 ( #18074, #29885, #29326 ) ),
 .UNSPECIFIED., .F., .F., .T. ) 
 B_SPLINE_SURFACE_WITH_KNOTS ( ( 4, 2, 4 ),
 ( 3, 3 ),
 ( 0.02453827135564170051, 0.02760610364996546329, 0.03067393594428922607 ),
 ( 0.000000000000000000, 1.000000000000000000 ),
 .UNSPECIFIED. ) 
 GEOMETRIC_REPRESENTATION_ITEM ( )  RATIONAL_B_SPLINE_SURFACE ( (
 ( 1.000000000000000000, 0.8047780919262715882, 1.000000000000000000),
 ( 1.000000000000000000, 0.8123791475856069200, 1.000000000000000000),
 ( 1.000000000000000000, 0.8190679386130260697, 1.000000000000000000),
 ( 1.000000000000000000, 0.8192344721910548300, 1.000000000000000000),
 ( 1.000000000000000000, 0.8126125954010035013, 1.000000000000000000),
 ( 1.000000000000000000, 0.8047712666188978625, 1.000000000000000000) ) ) 
 REPRESENTATION_ITEM ( '' )  SURFACE ( )  );
#3027 = EDGE_CURVE ( 'NONE', #8351, #15508, #29304, .T. ) ;
#3028 = DIRECTION ( 'NONE',  ( -1.000000000000000000, 0.000000000000000000, 0.000000000000000000 ) ) ;
#3029 = DIRECTION ( 'NONE',  ( 1.000000000000000000, 0.000000000000000000, 0.000000000000000000 ) ) ;
#3030 = EDGE_LOOP ( 'NONE', ( #30592, #21771, #3521, #11712 ) ) ;
#3031 = VECTOR ( 'NONE', #32655, 1000.000000000000000 ) ;
#3032 = CYLINDRICAL_SURFACE ( 'NONE', #31620, 2.000000000000001776 ) ;
#3033 = EDGE_CURVE ( 'NONE', #29904, #18462, #28912, .T. ) ;
#3034 = DIRECTION ( 'NONE',  ( 0.000000000000000000, -0.4999999999999996114, 0.8660254037844388186 ) ) ;
#3035 = EDGE_CURVE ( 'NONE', #17786, #28544, #21425, .T. ) ;
#3036 = ORIENTED_EDGE ( 'NONE', *, *, #10642, .F. ) ;
#3037 = ORIENTED_EDGE ( 'NONE', *, *, #5291, .T. ) ;
#3038 = CARTESIAN_POINT ( 'NONE',  ( 59.99999662536843914, -34.64101615137759893, 17.49999999999999645 ) ) ;
#3039 = CARTESIAN_POINT ( 'NONE',  ( 21.99999662536857770, 86.60254037844397601, 12.50000000000000000 ) ) ;
#3040 = CIRCLE ( 'NONE', #6032, 2.000000000000001776 ) ;
#3041 = FACE_BOUND ( 'NONE', #30009, .T. ) ;
#3042 = DIRECTION ( 'NONE',  ( 0.000000000000000000, 0.000000000000000000, 1.000000000000000000 ) ) ;
#3043 = VERTEX_POINT ( 'NONE', #12775 ) ;
#3044 = ORIENTED_EDGE ( 'NONE', *, *, #31062, .F. ) ;
#3045 = EDGE_CURVE ( 'NONE', #6546, #20763, #32868, .T. ) ;
#3046 = DIRECTION ( 'NONE',  ( 0.000000000000000000, 0.000000000000000000, 1.000000000000000000 ) ) ;
#3047 = CARTESIAN_POINT ( 'NONE',  ( 3.050000000000000711, 0.000000000000000000, 2.266666666666999674 ) ) ;
#3048 = EDGE_CURVE ( 'NONE', #26912, #20671, #22370, .T. ) ;
#3049 = FACE_BOUND ( 'NONE', #20436, .T. ) ;
#3050 = ADVANCED_FACE ( 'NONE', ( #9231 ), #32303, .F. ) ;
#3051 = VERTEX_POINT ( 'NONE', #30039 ) ;
#3052 = EDGE_CURVE ( 'NONE', #30350, #1819, #6197, .T. ) ;
#3053 = CARTESIAN_POINT ( 'NONE',  ( 0.000000000000000000, 5.939536975864662969E-16, -4.700000000000000178 ) ) ;
#3054 = EDGE_LOOP ( 'NONE', ( #116, #12528, #22839, #23482 ) ) ;
#3055 = ORIENTED_EDGE ( 'NONE', *, *, #32137, .F. ) ;
#3056 = CARTESIAN_POINT ( 'NONE',  ( -25.00000337463121980, -77.94228634059963667, 12.50000000000000000 ) ) ;
#3057 = CARTESIAN_POINT ( 'NONE',  ( -51.13139720814438505, -27.49999999999955591, -15.00000000000000000 ) ) ;
#3058 = ORIENTED_EDGE ( 'NONE', *, *, #16911, .T. ) ;
#3059 = ORIENTED_EDGE ( 'NONE', *, *, #2557, .F. ) ;
#3060 = CARTESIAN_POINT ( 'NONE',  ( -2.000003374631289521, -69.28203230275519786, -9.999999999999998224 ) ) ;
#3061 = CARTESIAN_POINT ( 'NONE',  ( 49.99999662536846756, -69.28203230275519786, 17.49999999999999645 ) ) ;
#3062 = LINE ( 'NONE', #31183, #7099 ) ;
#3063 = VERTEX_POINT ( 'NONE', #15229 ) ;
#3064 = CARTESIAN_POINT ( 'NONE',  ( 79.99999662536833966, 17.32050807568879236, 12.50000000000000000 ) ) ;
#3065 = AXIS2_PLACEMENT_3D ( 'NONE', #7485, #8034, #33919 ) ;
#3066 = FACE_BOUND ( 'NONE', #20042, .T. ) ;
#3067 = CARTESIAN_POINT ( 'NONE',  ( 44.13139720814418610, 27.49999999999988987, -5.000000000000000888 ) ) ;
#3068 = FACE_OUTER_BOUND ( 'NONE', #29152, .T. ) ;
#3069 = CARTESIAN_POINT ( 'NONE',  ( 44.99999662536849598, -77.94228634059960825, -9.999999999999998224 ) ) ;
#3070 = DIRECTION ( 'NONE',  ( 1.000000000000000000, 0.000000000000000000, 0.000000000000000000 ) ) ;
#3071 = DIRECTION ( 'NONE',  ( 1.000000000000000000, 0.000000000000000000, 0.000000000000000000 ) ) ;
#3072 = CARTESIAN_POINT ( 'NONE',  ( -58.48108235278846934, -36.97203788309006001, 12.49999999999999645 ) ) ;
#3073 = EDGE_LOOP ( 'NONE', ( #17456, #12380, #2145, #18604 ) ) ;
#3074 = DIRECTION ( 'NONE',  ( 0.000000000000000000, 0.000000000000000000, 1.000000000000000000 ) ) ;
#3075 = CARTESIAN_POINT ( 'NONE',  ( -0.8653900595644542504, 5.556556492855577289, -4.190801088233095051 ) ) ;
#3076 = DIRECTION ( 'NONE',  ( 0.000000000000000000, 0.000000000000000000, 1.000000000000000000 ) ) ;
#3077 = ORIENTED_EDGE ( 'NONE', *, *, #30519, .F. ) ;
#3078 = ORIENTED_EDGE ( 'NONE', *, *, #7785, .F. ) ;
#3079 = ORIENTED_EDGE ( 'NONE', *, *, #4809, .T. ) ;
#3080 = CARTESIAN_POINT ( 'NONE',  ( 9.999996625368625658, 86.60254037844397601, -9.999999999999998224 ) ) ;
#3081 = DIRECTION ( 'NONE',  ( 1.000000000000000000, 0.000000000000000000, 0.000000000000000000 ) ) ;
#3082 = DIRECTION ( 'NONE',  ( 1.000000000000000000, 0.000000000000000000, 0.000000000000000000 ) ) ;
#3083 = ORIENTED_EDGE ( 'NONE', *, *, #14865, .T. ) ;
#3084 = DIRECTION ( 'NONE',  ( -1.000000000000000000, 0.000000000000000000, 0.000000000000000000 ) ) ;
#3085 = VERTEX_POINT ( 'NONE', #12037 ) ;
#3086 = ADVANCED_FACE ( 'NONE', ( #23495 ), #32100, .F. ) ;
#3087 = DIRECTION ( 'NONE',  ( 0.000000000000000000, 0.000000000000000000, 1.000000000000000000 ) ) ;
#3088 = ORIENTED_EDGE ( 'NONE', *, *, #20087, .F. ) ;
#3089 = DIRECTION ( 'NONE',  ( -0.000000000000000000, -0.000000000000000000, -1.000000000000000000 ) ) ;
#3090 = EDGE_LOOP ( 'NONE', ( #28997, #6446, #27276, #35613 ) ) ;
#3091 = ORIENTED_EDGE ( 'NONE', *, *, #22663, .F. ) ;
#3092 = DIRECTION ( 'NONE',  ( 0.000000000000000000, 0.000000000000000000, 1.000000000000000000 ) ) ;
#3093 = CARTESIAN_POINT ( 'NONE',  ( 19.99999662536858835, 69.28203230275516944, -9.999999999999998224 ) ) ;
#3094 = CARTESIAN_POINT ( 'NONE',  ( 3.514986608498387177, 4.017641317389688993, -4.057689166958403426 ) ) ;
#3095 = VERTEX_POINT ( 'NONE', #17875 ) ;
#3096 = CARTESIAN_POINT ( 'NONE',  ( 21.99999662536862033, -86.60254037844400443, -9.999999999999998224 ) ) ;
#3097 = DIRECTION ( 'NONE',  ( 0.000000000000000000, 0.000000000000000000, 1.000000000000000000 ) ) ;
#3098 = LINE ( 'NONE', #26149, #15179 ) ;
#3099 = ORIENTED_EDGE ( 'NONE', *, *, #14997, .F. ) ;
#3100 = LINE ( 'NONE', #650, #5161 ) ;
#3101 = DIRECTION ( 'NONE',  ( 0.000000000000000000, 0.000000000000000000, 1.000000000000000000 ) ) ;
#3102 = AXIS2_PLACEMENT_3D ( 'NONE', #35158, #6644, #12626 ) ;
#3103 = ORIENTED_EDGE ( 'NONE', *, *, #2827, .T. ) ;
#3104 = CYLINDRICAL_SURFACE ( 'NONE', #24427, 2.000000000000000000 ) ;
#3105 = DIRECTION ( 'NONE',  ( 0.000000000000000000, 0.000000000000000000, 1.000000000000000000 ) ) ;
#3106 = DIRECTION ( 'NONE',  ( -1.000000000000000000, 0.000000000000000000, 0.000000000000000000 ) ) ;
#3107 = EDGE_CURVE ( 'NONE', #17753, #29194, #9784, .T. ) ;
#3108 = EDGE_CURVE ( 'NONE', #9038, #22407, #2616, .T. ) ;
#3109 = CARTESIAN_POINT ( 'NONE',  ( 72.99999662536836809, 25.98076211353319565, -9.999999999999998224 ) ) ;
#3110 = B_SPLINE_CURVE_WITH_KNOTS ( 'NONE', 3,
 ( #35453, #12720, #9927, #30555, #36727, #1864, #11027, #28104 ),
 .UNSPECIFIED., .F., .F.,
 ( 4, 2, 2, 4 ),
 ( 2.451332856840218572E-07, 0.001475502392055680302, 0.002213131021440678352, 0.002950759650825675751 ),
 .UNSPECIFIED. ) ;
#3111 = LINE ( 'NONE', #12452, #34095 ) ;
#3112 = EDGE_LOOP ( 'NONE', ( #16665, #3669, #14434, #31474, #12126 ) ) ;
#3113 = CARTESIAN_POINT ( 'NONE',  ( 79.99999662536833966, -3.469446951953614189E-15, -9.999999999999998224 ) ) ;
#3114 = DIRECTION ( 'NONE',  ( 0.000000000000000000, 0.000000000000000000, 1.000000000000000000 ) ) ;
#3115 = ORIENTED_EDGE ( 'NONE', *, *, #3137, .T. ) ;
#3117 = EDGE_LOOP ( 'NONE', ( #1931, #25655, #439, #24884, #18028 ) ) ;
#3116 = ADVANCED_FACE ( 'NONE', ( #24058 ), #35501, .F. ) ;
#3118 = VERTEX_POINT ( 'NONE', #16354 ) ;
#3119 =( NAMED_UNIT ( * ) PLANE_ANGLE_UNIT ( ) SI_UNIT ( $, .RADIAN. ) );
#3120 = CARTESIAN_POINT ( 'NONE',  ( 46.99999662536849598, 60.62177826491077326, -5.000000000000000000 ) ) ;
#3121 = CARTESIAN_POINT ( 'NONE',  ( -22.00000337463124112, 69.28203230275516944, -9.999999999999998224 ) ) ;
#3122 = AXIS2_PLACEMENT_3D ( 'NONE', #13159, #35858, #21408 ) ;
#3123 = CARTESIAN_POINT ( 'NONE',  ( -10.21421600225141724, -84.61404523131187716, -5.000000000000000000 ) ) ;
#3124 = ORIENTED_EDGE ( 'NONE', *, *, #35306, .F. ) ;
#3125 = ADVANCED_FACE ( 'NONE', ( #30773 ), #36093, .F. ) ;
#3126 = CARTESIAN_POINT ( 'NONE',  ( -82.00000337463094979, 17.32050807568878525, -9.999999999999998224 ) ) ;
#3127 = VERTEX_POINT ( 'NONE', #13730 ) ;
#3128 = FACE_BOUND ( 'NONE', #6857, .T. ) ;
#3129 = CARTESIAN_POINT ( 'NONE',  ( -75.00000337463100664, -43.30127018922202353, 12.50000000000000000 ) ) ;
#3130 = CARTESIAN_POINT ( 'NONE',  ( 0.000000000000000000, 81.28776890242656350, -29.99999999999985434 ) ) ;
#3131 = CARTESIAN_POINT ( 'NONE',  ( 74.99999662536835388, -43.30127018922199511, 12.50000000000000000 ) ) ;
#3132 = DIRECTION ( 'NONE',  ( 0.000000000000000000, 0.000000000000000000, 1.000000000000000000 ) ) ;
#3133 = DIRECTION ( 'NONE',  ( 1.000000000000000000, 0.000000000000000000, 0.000000000000000000 ) ) ;
#3134 = CIRCLE ( 'NONE', #22915, 2.000000000000001776 ) ;
#3135 = CARTESIAN_POINT ( 'NONE',  ( -53.00000337463106348, 43.30127018922197379, -9.999999999999998224 ) ) ;
#3136 = CARTESIAN_POINT ( 'NONE',  ( 61.06482292022109704, -72.77422209630303485, -5.000000000000000000 ) ) ;
#3137 = EDGE_CURVE ( 'NONE', #36216, #9400, #12770, .T. ) ;
#3138 = ORIENTED_EDGE ( 'NONE', *, *, #34210, .T. ) ;
#3139 = CARTESIAN_POINT ( 'NONE',  ( 0.000000000000000000, 89.94802294027097389, -24.99999999999990763 ) ) ;
#3140 = DIRECTION ( 'NONE',  ( 0.000000000000000000, 0.000000000000000000, -1.000000000000000000 ) ) ;
#3141 = DIRECTION ( 'NONE',  ( 1.000000000000000000, 0.000000000000000000, 0.000000000000000000 ) ) ;
#3142 = ORIENTED_EDGE ( 'NONE', *, *, #32210, .T. ) ;
#3143 = EDGE_LOOP ( 'NONE', ( #16788, #5054 ) ) ;
#3144 = VECTOR ( 'NONE', #23613, 1000.000000000000000 ) ;
#3145 = ORIENTED_EDGE ( 'NONE', *, *, #15609, .T. ) ;
#3146 = EDGE_CURVE ( 'NONE', #695, #17257, #27150, .T. ) ;
#3147 = DIRECTION ( 'NONE',  ( 3.491481338843133355E-15, 1.000000000000000000, 0.000000000000000000 ) ) ;
#3148 = ADVANCED_FACE ( 'NONE', ( #36055 ), #16184, .T. ) ;
#3149 = DIRECTION ( 'NONE',  ( -1.000000000000000000, 0.000000000000000000, 0.000000000000000000 ) ) ;
#3150 = DIRECTION ( 'NONE',  ( 0.000000000000000000, 0.000000000000000000, 1.000000000000000000 ) ) ;
#3151 = DIRECTION ( 'NONE',  ( 0.000000000000000000, 0.000000000000000000, -1.000000000000000000 ) ) ;
#3152 = CARTESIAN_POINT ( 'NONE',  ( -37.00000337463116296, 60.62177826491077326, -9.999999999999998224 ) ) ;
#3153 = ORIENTED_EDGE ( 'NONE', *, *, #22779, .F. ) ;
#3154 = EDGE_LOOP ( 'NONE', ( #27426, #3715 ) ) ;
#3155 = CIRCLE ( 'NONE', #15140, 2.000000000000001776 ) ;
#3156 = CARTESIAN_POINT ( 'NONE',  ( 47.99999662536848177, -51.96152422706640550, 17.49999999999999645 ) ) ;
#3157 = CARTESIAN_POINT ( 'NONE',  ( -25.00000000000000000, 0.000000000000000000, 15.00000000000000000 ) ) ;
#3158 = FACE_OUTER_BOUND ( 'NONE', #23959, .T. ) ;
#3159 = VERTEX_POINT ( 'NONE', #10186 ) ;
#3160 = EDGE_CURVE ( 'NONE', #36052, #13357, #33221, .T. ) ;
#3161 = CARTESIAN_POINT ( 'NONE',  ( 0.000000000000000000, 89.94802294027088863, -24.99999999999999645 ) ) ;
#3162 = EDGE_LOOP ( 'NONE', ( #10503, #25222, #32784, #8227 ) ) ;
#3163 = CIRCLE ( 'NONE', #31885, 3.000000000000008882 ) ;
#3164 = ORIENTED_EDGE ( 'NONE', *, *, #31640, .F. ) ;
#3165 = AXIS2_PLACEMENT_3D ( 'NONE', #19480, #16307, #19308 ) ;
#3166 = CARTESIAN_POINT ( 'NONE',  ( -77.00000337463097821, 43.30127018922197379, 12.50000000000000000 ) ) ;
#3167 = VERTEX_POINT ( 'NONE', #4549 ) ;
#3168 =( NAMED_UNIT ( * ) SI_UNIT ( $, .STERADIAN. ) SOLID_ANGLE_UNIT ( ) );
#3169 = ADVANCED_FACE ( 'NONE', ( #8097 ), #18991, .F. ) ;
#3170 = CARTESIAN_POINT ( 'NONE',  ( 44.99999662536851019, -60.62177826491080168, -9.999999999999998224 ) ) ;
#3171 = CYLINDRICAL_SURFACE ( 'NONE', #4713, 2.000000000000001776 ) ;
#3172 = EDGE_CURVE ( 'NONE', #35280, #29596, #27218, .T. ) ;
#3173 = ORIENTED_EDGE ( 'NONE', *, *, #3048, .T. ) ;
#3174 = APPLICATION_CONTEXT ( 'automotive_design' ) ;
#3175 = ORIENTED_EDGE ( 'NONE', *, *, #18253, .T. ) ;
#3176 = AXIS2_PLACEMENT_3D ( 'NONE', #35134, #12208, #24227 ) ;
#3177 = ORIENTED_EDGE ( 'NONE', *, *, #36558, .F. ) ;
#3178 = ORIENTED_EDGE ( 'NONE', *, *, #493, .T. ) ;
#3179 = ORIENTED_EDGE ( 'NONE', *, *, #31846, .F. ) ;
#3180 = DIRECTION ( 'NONE',  ( 0.000000000000000000, 0.000000000000000000, 1.000000000000000000 ) ) ;
#3181 = DIRECTION ( 'NONE',  ( 0.000000000000000000, 0.000000000000000000, 1.000000000000000000 ) ) ;
#3182 = CYLINDRICAL_SURFACE ( 'NONE', #11857, 2.000000000000000000 ) ;
#3183 = DIRECTION ( 'NONE',  ( 0.000000000000000000, 0.000000000000000000, -1.000000000000000000 ) ) ;
#3184 = DIRECTION ( 'NONE',  ( 0.000000000000000000, 0.000000000000000000, -1.000000000000000000 ) ) ;
#3185 = ORIENTED_EDGE ( 'NONE', *, *, #20789, .F. ) ;
#3186 = LINE ( 'NONE', #20805, #36237 ) ;
#3187 = DIRECTION ( 'NONE',  ( 0.000000000000000000, 0.000000000000000000, 1.000000000000000000 ) ) ;
#3188 = EDGE_CURVE ( 'NONE', #20479, #16067, #10987, .T. ) ;
#3189 = AXIS2_PLACEMENT_3D ( 'NONE', #5345, #28192, #10773 ) ;
#3190 = DIRECTION ( 'NONE',  ( -1.000000000000000000, -0.000000000000000000, -0.000000000000000000 ) ) ;
#3191 = ORIENTED_EDGE ( 'NONE', *, *, #5240, .T. ) ;
#3192 = DIRECTION ( 'NONE',  ( 0.000000000000000000, 0.000000000000000000, 1.000000000000000000 ) ) ;
#3193 = DIRECTION ( 'NONE',  ( 1.000000000000000000, 0.000000000000000000, 0.000000000000000000 ) ) ;
#3194 = EDGE_LOOP ( 'NONE', ( #2337, #34005, #15980, #817 ) ) ;
#3195 = ORIENTED_EDGE ( 'NONE', *, *, #4704, .T. ) ;
#3196 = DIRECTION ( 'NONE',  ( -0.7071067811865439090, 0.7071067811865512365, 0.000000000000000000 ) ) ;
#3197 = DIRECTION ( 'NONE',  ( -1.000000000000000000, 0.000000000000000000, 0.000000000000000000 ) ) ;
#3198 = CARTESIAN_POINT ( 'NONE',  ( -47.63139720814380951, 27.50000000000055422, -5.000000000000000888 ) ) ;
#3199 = CARTESIAN_POINT ( 'NONE',  ( 0.000000000000000000, 0.000000000000000000, -5.000000000000000000 ) ) ;
#3200 = ORIENTED_EDGE ( 'NONE', *, *, #18319, .T. ) ;
#3201 = AXIS2_PLACEMENT_3D ( 'NONE', #27421, #11082, #25730 ) ;
#3202 = DIRECTION ( 'NONE',  ( 1.000000000000000000, 0.000000000000000000, 0.000000000000000000 ) ) ;
#3203 = LINE ( 'NONE', #387, #28521 ) ;
#3204 = CARTESIAN_POINT ( 'NONE',  ( -55.88972745734202618, -33.99999999999965894, 12.49999999999999822 ) ) ;
#3205 = AXIS2_PLACEMENT_3D ( 'NONE', #13860, #7882, #24943 ) ;
#3206 = EDGE_CURVE ( 'NONE', #29329, #27821, #36748, .T. ) ;
#3207 = ORIENTED_EDGE ( 'NONE', *, *, #13498, .F. ) ;
#3208 = EDGE_CURVE ( 'NONE', #25631, #28369, #4420, .T. ) ;
#3209 = CARTESIAN_POINT ( 'NONE',  ( 62.99999662536839651, -60.62177826491080168, -9.999999999999998224 ) ) ;
#3210 = ORIENTED_EDGE ( 'NONE', *, *, #13181, .F. ) ;
#3211 = FACE_OUTER_BOUND ( 'NONE', #31371, .T. ) ;
#3212 = VECTOR ( 'NONE', #18504, 1000.000000000000000 ) ;
#3213 = EDGE_CURVE ( 'NONE', #36127, #20281, #24432, .T. ) ;
#3214 = LINE ( 'NONE', #23289, #29559 ) ;
#3215 = AXIS2_PLACEMENT_3D ( 'NONE', #33415, #7908, #1524 ) ;
#3216 = DIRECTION ( 'NONE',  ( 0.000000000000000000, 0.000000000000000000, 1.000000000000000000 ) ) ;
#3217 = ORIENTED_EDGE ( 'NONE', *, *, #9460, .T. ) ;
#3218 = VERTEX_POINT ( 'NONE', #33046 ) ;
#3219 = EDGE_CURVE ( 'NONE', #23390, #21452, #21160, .T. ) ;
#3220 = DIRECTION ( 'NONE',  ( 0.000000000000000000, 0.000000000000000000, -1.000000000000000000 ) ) ;
#3221 = EDGE_CURVE ( 'NONE', #20810, #14063, #5003, .T. ) ;
#3222 = CIRCLE ( 'NONE', #18180, 2.000000000000001776 ) ;
#3223 = DIRECTION ( 'NONE',  ( 1.000000000000000000, 0.000000000000000000, 0.000000000000000000 ) ) ;
#3224 = DIRECTION ( 'NONE',  ( 1.000000000000000000, 0.000000000000000000, 0.000000000000000000 ) ) ;
#3225 = EDGE_LOOP ( 'NONE', ( #35673, #24923, #9340, #11117 ) ) ;
#3226 = DIRECTION ( 'NONE',  ( 0.000000000000000000, 0.000000000000000000, 1.000000000000000000 ) ) ;
#3227 = FACE_BOUND ( 'NONE', #35804, .T. ) ;
#3228 = DIRECTION ( 'NONE',  ( 1.000000000000000000, 0.000000000000000000, 0.000000000000000000 ) ) ;
#3229 = DIRECTION ( 'NONE',  ( -0.000000000000000000, -0.000000000000000000, -1.000000000000000000 ) ) ;
#3230 = FACE_OUTER_BOUND ( 'NONE', #22273, .T. ) ;
#3231 = EDGE_CURVE ( 'NONE', #3360, #29817, #17084, .T. ) ;
#3232 = CARTESIAN_POINT ( 'NONE',  ( 7.999996625368656744, -86.60254037844400443, -5.000000000000000000 ) ) ;
#3233 = EDGE_CURVE ( 'NONE', #460, #28766, #28711, .T. ) ;
#3234 = AXIS2_PLACEMENT_3D ( 'NONE', #1081, #12507, #21693 ) ;
#3235 = FACE_OUTER_BOUND ( 'NONE', #14571, .T. ) ;
#3236 = EDGE_CURVE ( 'NONE', #29323, #29299, #28826, .T. ) ;
#3237 = EDGE_CURVE ( 'NONE', #24381, #26240, #35447, .T. ) ;
#3238 = CARTESIAN_POINT ( 'NONE',  ( 69.99999662536838230, -51.96152422706639840, 17.49999999999999645 ) ) ;
#3239 = EDGE_LOOP ( 'NONE', ( #14781, #30688 ) ) ;
#3240 = EDGE_CURVE ( 'NONE', #33684, #32017, #11282, .T. ) ;
#3241 = DIRECTION ( 'NONE',  ( 0.000000000000000000, -0.000000000000000000, -1.000000000000000000 ) ) ;
#3242 = LINE ( 'NONE', #17667, #10545 ) ;
#3243 = DIRECTION ( 'NONE',  ( 0.000000000000000000, 0.000000000000000000, 1.000000000000000000 ) ) ;
#3244 = AXIS2_PLACEMENT_3D ( 'NONE', #36753, #36584, #7892 ) ;
#3245 = ORIENTED_EDGE ( 'NONE', *, *, #27611, .T. ) ;
#3246 = ORIENTED_EDGE ( 'NONE', *, *, #15145, .F. ) ;
#3247 = ORIENTED_EDGE ( 'NONE', *, *, #32470, .F. ) ;
#3248 = CIRCLE ( 'NONE', #30778, 6.000000000000005329 ) ;
#3249 = DIRECTION ( 'NONE',  ( 0.000000000000000000, 0.000000000000000000, -1.000000000000000000 ) ) ;
#3250 = CARTESIAN_POINT ( 'NONE',  ( 0.000000000000000000, 0.000000000000000000, 0.000000000000000000 ) ) ;
#3251 = CYLINDRICAL_SURFACE ( 'NONE', #25031, 2.000000000000001776 ) ;
#3252 = VERTEX_POINT ( 'NONE', #20442 ) ;
#3253 = FACE_OUTER_BOUND ( 'NONE', #19160, .T. ) ;
#3254 = VERTEX_POINT ( 'NONE', #22529 ) ;
#3255 = CARTESIAN_POINT ( 'NONE',  ( 5.078940004773329520, -119.6165172753982375, 32.50000000000000000 ) ) ;
#3256 = AXIS2_PLACEMENT_3D ( 'NONE', #18164, #15733, #27155 ) ;
#3257 = ORIENTED_EDGE ( 'NONE', *, *, #28542, .T. ) ;
#3258 = DIRECTION ( 'NONE',  ( 0.000000000000000000, 0.000000000000000000, 1.000000000000000000 ) ) ;
#3259 = EDGE_LOOP ( 'NONE', ( #28821, #10348 ) ) ;
#3260 = ORIENTED_EDGE ( 'NONE', *, *, #35132, .F. ) ;
#3261 = AXIS2_PLACEMENT_3D ( 'NONE', #29911, #13726, #27773 ) ;
#3262 = DIRECTION ( 'NONE',  ( 0.000000000000000000, 0.000000000000000000, 1.000000000000000000 ) ) ;
#3263 = CARTESIAN_POINT ( 'NONE',  ( 59.99999662536842493, 51.96152422706639129, 17.49999999999999645 ) ) ;
#3264 = ORIENTED_EDGE ( 'NONE', *, *, #26845, .T. ) ;
#3265 = CARTESIAN_POINT ( 'NONE',  ( 49.99999662536848177, -51.96152422706640550, -9.999999999999998224 ) ) ;
#3266 = CIRCLE ( 'NONE', #24221, 2.000000000000000000 ) ;
#3267 = DIRECTION ( 'NONE',  ( 1.000000000000000000, 0.000000000000000000, 0.000000000000000000 ) ) ;
#3268 = DIRECTION ( 'NONE',  ( 0.000000000000000000, 0.000000000000000000, 1.000000000000000000 ) ) ;
#3269 = EDGE_LOOP ( 'NONE', ( #17380, #35791, #20188, #31378 ) ) ;
#3270 = AXIS2_PLACEMENT_3D ( 'NONE', #27491, #33299, #24685 ) ;
#3271 = DIRECTION ( 'NONE',  ( 0.000000000000000000, 0.000000000000000000, 1.000000000000000000 ) ) ;
#3272 = LINE ( 'NONE', #14707, #20967 ) ;
#3273 = ORIENTED_EDGE ( 'NONE', *, *, #3350, .T. ) ;
#3274 = CYLINDRICAL_SURFACE ( 'NONE', #34601, 2.000000000000001776 ) ;
#3275 = CARTESIAN_POINT ( 'NONE',  ( 51.99999662536848888, -51.96152422706640550, -5.000000000000000000 ) ) ;
#3276 = CYLINDRICAL_SURFACE ( 'NONE', #18962, 3.000000000000002665 ) ;
#3277 = CARTESIAN_POINT ( 'NONE',  ( -56.52018970185233826, 35.83991598322119643, -4.999999999999997335 ) ) ;
#3278 = EDGE_CURVE ( 'NONE', #23804, #31278, #34841, .T. ) ;
#3279 = DIRECTION ( 'NONE',  ( 1.000000000000000000, 0.000000000000000000, 0.000000000000000000 ) ) ;
#3280 = AXIS2_PLACEMENT_3D ( 'NONE', #34999, #32373, #14557 ) ;
#3281 = EDGE_CURVE ( 'NONE', #17590, #24370, #24061, .T. ) ;
#3282 = ORIENTED_EDGE ( 'NONE', *, *, #19239, .F. ) ;
#3284 = CIRCLE ( 'NONE', #24845, 2.000000000000000000 ) ;
#3283 = CARTESIAN_POINT ( 'NONE',  ( -25.00000337463120914, 77.94228634059957983, -9.999999999999998224 ) ) ;
#3285 = DIRECTION ( 'NONE',  ( -0.8660254037844383745, 0.5000000000000005551, 0.000000000000000000 ) ) ;
#3286 = DIRECTION ( 'NONE',  ( -0.000000000000000000, 0.000000000000000000, -1.000000000000000000 ) ) ;
#3287 = VERTEX_POINT ( 'NONE', #34175 ) ;
#3288 = VECTOR ( 'NONE', #18584, 1000.000000000000000 ) ;
#3289 = ORIENTED_EDGE ( 'NONE', *, *, #20583, .F. ) ;
#3290 = ORIENTED_EDGE ( 'NONE', *, *, #3240, .F. ) ;
#3291 = SURFACE_STYLE_FILL_AREA ( #31782 ) ;
#3292 = DIRECTION ( 'NONE',  ( -1.000000000000000000, 0.000000000000000000, 0.000000000000000000 ) ) ;
#3293 = DIRECTION ( 'NONE',  ( 0.000000000000000000, 0.000000000000000000, 1.000000000000000000 ) ) ;
#3294 = CIRCLE ( 'NONE', #6290, 2.000000000000000000 ) ;
#3295 = CIRCLE ( 'NONE', #4510, 65.00000000000000000 ) ;
#3296 = DIRECTION ( 'NONE',  ( -0.000000000000000000, -0.000000000000000000, -1.000000000000000000 ) ) ;
#3297 = ORIENTED_EDGE ( 'NONE', *, *, #35692, .F. ) ;
#3298 = DIRECTION ( 'NONE',  ( 0.000000000000000000, 0.000000000000000000, 1.000000000000000000 ) ) ;
#3299 = ORIENTED_EDGE ( 'NONE', *, *, #31791, .T. ) ;
#3300 = FACE_BOUND ( 'NONE', #27954, .T. ) ;
#3301 = EDGE_CURVE ( 'NONE', #15339, #11692, #31814, .T. ) ;
#3302 = CARTESIAN_POINT ( 'NONE',  ( -27.00000337463121625, -77.94228634059963667, -9.999999999999998224 ) ) ;
#3303 = CIRCLE ( 'NONE', #21882, 2.000000000000001776 ) ;
#3304 = DIRECTION ( 'NONE',  ( 1.000000000000000000, 0.000000000000000000, 0.000000000000000000 ) ) ;
#3305 = AXIS2_PLACEMENT_3D ( 'NONE', #3479, #23917, #15469 ) ;
#3306 = ORIENTED_EDGE ( 'NONE', *, *, #16688, .F. ) ;
#3307 = DIRECTION ( 'NONE',  ( 0.000000000000000000, 0.000000000000000000, -1.000000000000000000 ) ) ;
#3308 = AXIS2_PLACEMENT_3D ( 'NONE', #36235, #25352, #16359 ) ;
#3309 = APPLICATION_PROTOCOL_DEFINITION ( 'draft international standard', 'automotive_design', 1998, #4893 ) ;
#3310 = AXIS2_PLACEMENT_3D ( 'NONE', #28071, #5203, #30687 ) ;
#3311 = CIRCLE ( 'NONE', #16485, 2.000000000000001776 ) ;
#3312 = CARTESIAN_POINT ( 'NONE',  ( 66.99999662536841072, -25.98076211353320275, 12.50000000000000000 ) ) ;
#3313 = EDGE_CURVE ( 'NONE', #8115, #13345, #2853, .T. ) ;
#3314 = PLANE ( 'NONE',  #23956 ) ;
#3315 = DIRECTION ( 'NONE',  ( -1.051347561198064495E-14, -1.000000000000000000, 0.000000000000000000 ) ) ;
#3316 = ORIENTED_EDGE ( 'NONE', *, *, #15234, .F. ) ;
#3317 = DIRECTION ( 'NONE',  ( 1.000000000000000000, 0.000000000000000000, 0.000000000000000000 ) ) ;
#3318 = CARTESIAN_POINT ( 'NONE',  ( 0.000000000000000000, 0.000000000000000000, 0.000000000000000000 ) ) ;
#3319 = CIRCLE ( 'NONE', #35099, 2.000000000000001776 ) ;
#3320 = DIRECTION ( 'NONE',  ( 0.000000000000000000, 0.000000000000000000, 1.000000000000000000 ) ) ;
#3321 = CIRCLE ( 'NONE', #15906, 24.99999999999999289 ) ;
#3322 = AXIS2_PLACEMENT_3D ( 'NONE', #14632, #5851, #3202 ) ;
#3323 = ORIENTED_EDGE ( 'NONE', *, *, #437, .T. ) ;
#3324 = VERTEX_POINT ( 'NONE', #22732 ) ;
#3325 = EDGE_CURVE ( 'NONE', #10822, #16313, #6097, .T. ) ;
#3326 = ORIENTED_EDGE ( 'NONE', *, *, #12201, .F. ) ;
#3327 = CARTESIAN_POINT ( 'NONE',  ( 69.13212189986965939, 2.778182860042805125, -4.999999999999997335 ) ) ;
#3328 = DIRECTION ( 'NONE',  ( 1.000000000000000000, 0.000000000000000000, -0.000000000000000000 ) ) ;
#3329 = CIRCLE ( 'NONE', #18919, 2.000000000000001776 ) ;
#3330 = CARTESIAN_POINT ( 'NONE',  ( -22.00000337463122690, 86.60254037844397601, -9.999999999999998224 ) ) ;
#3331 = CARTESIAN_POINT ( 'NONE',  ( 6.000000000000000000, 0.000000000000000000, 27.50000000000000000 ) ) ;
#3332 = AXIS2_PLACEMENT_3D ( 'NONE', #23108, #29461, #15045 ) ;
#3333 = DIRECTION ( 'NONE',  ( 1.000000000000000000, 0.000000000000000000, 0.000000000000000000 ) ) ;
#3334 = AXIS2_PLACEMENT_3D ( 'NONE', #18322, #35589, #21133 ) ;
#3335 = AXIS2_PLACEMENT_3D ( 'NONE', #13182, #24631, #33228 ) ;
#3336 = CARTESIAN_POINT ( 'NONE',  ( -56.67878100130369035, 27.78182860042797131, 12.49999999999999822 ) ) ;
#3337 = VECTOR ( 'NONE', #35736, 1000.000000000000000 ) ;
#3338 = ORIENTED_EDGE ( 'NONE', *, *, #7196, .T. ) ;
#3339 = VERTEX_POINT ( 'NONE', #26075 ) ;
#3340 = CARTESIAN_POINT ( 'NONE',  ( -5.000003374631307729, 77.94228634059957983, -9.999999999999998224 ) ) ;
#3341 = EDGE_CURVE ( 'NONE', #792, #36127, #4902, .T. ) ;
#3342 = DIRECTION ( 'NONE',  ( 0.000000000000000000, 0.000000000000000000, -1.000000000000000000 ) ) ;
#3343 = DIRECTION ( 'NONE',  ( -1.000000000000000000, 0.000000000000000000, 0.000000000000000000 ) ) ;
#3344 = ORIENTED_EDGE ( 'NONE', *, *, #14200, .F. ) ;
#3345 = EDGE_CURVE ( 'NONE', #33803, #22230, #5645, .T. ) ;
#3346 = AXIS2_PLACEMENT_3D ( 'NONE', #27136, #36342, #36149 ) ;
#3347 = FACE_OUTER_BOUND ( 'NONE', #20210, .T. ) ;
#3348 = ORIENTED_EDGE ( 'NONE', *, *, #1825, .F. ) ;
#3349 = ORIENTED_EDGE ( 'NONE', *, *, #21588, .F. ) ;
#3350 = EDGE_CURVE ( 'NONE', #14947, #35287, #13877, .T. ) ;
#3351 = CARTESIAN_POINT ( 'NONE',  ( -25.00000337463120914, 77.94228634059957983, 12.50000000000000000 ) ) ;
#3352 = ORIENTED_EDGE ( 'NONE', *, *, #14752, .T. ) ;
#3353 = PRESENTATION_STYLE_ASSIGNMENT (( #26590 ) ) ;
#3354 = AXIS2_PLACEMENT_3D ( 'NONE', #13364, #22009, #18827 ) ;
#3355 = FACE_OUTER_BOUND ( 'NONE', #13531, .T. ) ;
#3356 = ADVANCED_FACE ( 'NONE', ( #11815, #16738, #3041, #2480, #5479, #16905, #36978, #34524 ), #8469, .F. ) ;
#3357 = VECTOR ( 'NONE', #17271, 1000.000000000000000 ) ;
#3358 = DIRECTION ( 'NONE',  ( -0.7071067811865382469, 8.659560562355048722E-17, -0.7071067811865568986 ) ) ;
#3359 = ORIENTED_EDGE ( 'NONE', *, *, #36714, .F. ) ;
#3360 = VERTEX_POINT ( 'NONE', #34339 ) ;
#3361 = CIRCLE ( 'NONE', #15351, 2.000000000000001776 ) ;
#3362 = VECTOR ( 'NONE', #20623, 1000.000000000000000 ) ;
#3363 = EDGE_LOOP ( 'NONE', ( #25159, #14521, #17445, #32150 ) ) ;
#3364 = AXIS2_PLACEMENT_3D ( 'NONE', #21386, #15946, #1497 ) ;
#3365 = AXIS2_PLACEMENT_3D ( 'NONE', #24268, #21469, #32907 ) ;
#3366 = ORIENTED_EDGE ( 'NONE', *, *, #1618, .T. ) ;
#3367 = CIRCLE ( 'NONE', #960, 2.000000000000001776 ) ;
#3368 = ORIENTED_EDGE ( 'NONE', *, *, #5978, .T. ) ;
#3369 = DIRECTION ( 'NONE',  ( 1.000000000000000000, 0.000000000000000000, 0.000000000000000000 ) ) ;
#3370 = ADVANCED_FACE ( 'NONE', ( #8639 ), #25893, .F. ) ;
#3371 = CARTESIAN_POINT ( 'NONE',  ( 39.99999662536853151, -69.28203230275519786, 12.50000000000000000 ) ) ;
#3372 = ORIENTED_EDGE ( 'NONE', *, *, #25765, .F. ) ;
#3373 = CARTESIAN_POINT ( 'NONE',  ( -80.00000337463096400, -34.64101615137762025, -9.999999999999998224 ) ) ;
#3374 = CARTESIAN_POINT ( 'NONE',  ( 107.3056475171454593, 47.85569953350209715, 32.50000000000000000 ) ) ;
#3375 = CARTESIAN_POINT ( 'NONE',  ( -45.00000337463111322, -77.94228634059960825, -9.999999999999998224 ) ) ;
#3376 = EDGE_LOOP ( 'NONE', ( #9996, #17506 ) ) ;
#3377 = LINE ( 'NONE', #6021, #17032 ) ;
#3378 = AXIS2_PLACEMENT_3D ( 'NONE', #6634, #5907, #26328 ) ;
#3379 = ADVANCED_FACE ( 'NONE', ( #23832 ), #9186, .T. ) ;
#3380 = CARTESIAN_POINT ( 'NONE',  ( 64.99999662536842493, 43.30127018922200222, 12.50000000000000000 ) ) ;
#3381 = DIRECTION ( 'NONE',  ( 0.000000000000000000, 0.000000000000000000, 1.000000000000000000 ) ) ;
#3382 = ORIENTED_EDGE ( 'NONE', *, *, #14250, .F. ) ;
#3383 = CARTESIAN_POINT ( 'NONE',  ( -89.42901512340354486, 31.83425564451495404, 12.49999999999999822 ) ) ;
#3384 = DIRECTION ( 'NONE',  ( 1.000000000000000000, 0.000000000000000000, 0.000000000000000000 ) ) ;
#3385 = VERTEX_POINT ( 'NONE', #35636 ) ;
#3386 = CIRCLE ( 'NONE', #24349, 95.00000000000000000 ) ;
#3387 = EDGE_CURVE ( 'NONE', #34182, #4700, #23464, .T. ) ;
#3388 = VERTEX_POINT ( 'NONE', #9938 ) ;
#3389 = DIRECTION ( 'NONE',  ( 1.000000000000000000, 0.000000000000000000, 0.000000000000000000 ) ) ;
#3390 = EDGE_CURVE ( 'NONE', #30431, #35240, #21051, .T. ) ;
#3391 = CARTESIAN_POINT ( 'NONE',  ( -63.00000337463104927, -43.30127018922202353, -5.000000000000000000 ) ) ;
#3392 = DIRECTION ( 'NONE',  ( 1.000000000000000000, 0.000000000000000000, 0.000000000000000000 ) ) ;
#3393 = DIRECTION ( 'NONE',  ( 1.000000000000000000, 0.000000000000000000, 0.000000000000000000 ) ) ;
#3394 = AXIS2_PLACEMENT_3D ( 'NONE', #5960, #31434, #5764 ) ;
#3395 = EDGE_LOOP ( 'NONE', ( #7115, #36322, #33273, #20770 ) ) ;
#3396 = AXIS2_PLACEMENT_3D ( 'NONE', #12624, #4011, #30237 ) ;
#3397 = CIRCLE ( 'NONE', #35155, 2.000000000000001776 ) ;
#3398 = CARTESIAN_POINT ( 'NONE',  ( -60.00000337463108480, -51.96152422706641971, -9.999999999999998224 ) ) ;
#3399 = ADVANCED_FACE ( 'NONE', ( #27004 ), #22267, .T. ) ;
#3401 = AXIS2_PLACEMENT_3D ( 'NONE', #10898, #33978, #11275 ) ;
#3400 = CARTESIAN_POINT ( 'NONE',  ( -4.999999999999997335, 0.000000000000000000, 0.000000000000000000 ) ) ;
#3402 = DIRECTION ( 'NONE',  ( 1.000000000000000000, 0.000000000000000000, 0.000000000000000000 ) ) ;
#3403 = CIRCLE ( 'NONE', #32126, 2.000000000000001776 ) ;
#3404 = ORIENTED_EDGE ( 'NONE', *, *, #19687, .T. ) ;
#3405 = EDGE_CURVE ( 'NONE', #18237, #11435, #98, .T. ) ;
#3406 = DIRECTION ( 'NONE',  ( 0.000000000000000000, 0.000000000000000000, 1.000000000000000000 ) ) ;
#3407 = ORIENTED_EDGE ( 'NONE', *, *, #14229, .F. ) ;
#3408 = DIRECTION ( 'NONE',  ( 1.000000000000000000, 0.000000000000000000, 0.000000000000000000 ) ) ;
#3409 = DIRECTION ( 'NONE',  ( -1.000000000000000000, 0.000000000000000000, 0.000000000000000000 ) ) ;
#3410 = EDGE_CURVE ( 'NONE', #17105, #7306, #20450, .T. ) ;
#3411 = DIRECTION ( 'NONE',  ( 0.000000000000000000, -1.000000000000000000, 0.000000000000000000 ) ) ;
#3412 = ORIENTED_EDGE ( 'NONE', *, *, #6554, .F. ) ;
#3413 = ORIENTED_EDGE ( 'NONE', *, *, #6964, .T. ) ;
#3414 = DIRECTION ( 'NONE',  ( 0.000000000000000000, 0.000000000000000000, 1.000000000000000000 ) ) ;
#3415 = AXIS2_PLACEMENT_3D ( 'NONE', #24206, #30396, #7341 ) ;
#3416 = FACE_OUTER_BOUND ( 'NONE', #14902, .T. ) ;
#3417 = DIRECTION ( 'NONE',  ( 1.000000000000000000, 0.000000000000000000, 0.000000000000000000 ) ) ;
#3418 = VECTOR ( 'NONE', #15474, 1000.000000000000000 ) ;
#3419 = EDGE_LOOP ( 'NONE', ( #4535, #9732 ) ) ;
#3420 = DIRECTION ( 'NONE',  ( 0.000000000000000000, 0.000000000000000000, -1.000000000000000000 ) ) ;
#3421 = TOROIDAL_SURFACE ( 'NONE', #24386, 17.55872235085560007, 2.000000000000000000 ) ;
#3422 = FACE_BOUND ( 'NONE', #10202, .T. ) ;
#3423 = LINE ( 'NONE', #25868, #29850 ) ;
#3424 = CYLINDRICAL_SURFACE ( 'NONE', #35230, 2.000000000000000000 ) ;
#3425 = CARTESIAN_POINT ( 'NONE',  ( 37.50000000000000000, 103.4105893997321743, -19.99999999999999645 ) ) ;
#3426 = CARTESIAN_POINT ( 'NONE',  ( -45.00000337463111322, -77.94228634059960825, -9.999999999999998224 ) ) ;
#3427 = COLOUR_RGB ( '', 0.08235294, 0.09019608, 0.10196078) ;
#3428 = DIRECTION ( 'NONE',  ( 0.000000000000000000, 0.000000000000000000, -1.000000000000000000 ) ) ;
#3429 = VECTOR ( 'NONE', #5045, 1000.000000000000114 ) ;
#3430 = EDGE_CURVE ( 'NONE', #14001, #27785, #7303, .T. ) ;
#3431 = CYLINDRICAL_SURFACE ( 'NONE', #31338, 24.99999999999999289 ) ;
#3432 = VERTEX_POINT ( 'NONE', #34894 ) ;
#3433 = CARTESIAN_POINT ( 'NONE',  ( 56.56138580058825482, 61.87160379013676703, -5.000000000000000000 ) ) ;
#3434 = CARTESIAN_POINT ( 'NONE',  ( 32.99999662536855283, -60.62177826491080168, -9.999999999999998224 ) ) ;
#3435 = CARTESIAN_POINT ( 'NONE',  ( 52.99999662536844625, -60.62177826491080168, -9.999999999999998224 ) ) ;
#3436 = AXIS2_PLACEMENT_3D ( 'NONE', #32548, #33110, #10422 ) ;
#3437 = ORIENTED_EDGE ( 'NONE', *, *, #34374, .F. ) ;
#3438 = AXIS2_PLACEMENT_3D ( 'NONE', #19153, #22314, #2615 ) ;
#3439 = EDGE_CURVE ( 'NONE', #29585, #11539, #32439, .T. ) ;
#3440 = EDGE_LOOP ( 'NONE', ( #23350, #21801 ) ) ;
#3441 = ORIENTED_EDGE ( 'NONE', *, *, #32369, .T. ) ;
#3442 = ADVANCED_FACE ( 'NONE', ( #14829 ), #35285, .F. ) ;
#3443 = CARTESIAN_POINT ( 'NONE',  ( 5.000000000000007994, -2.886751345948139758, -0.5999999999999998668 ) ) ;
#3444 = CARTESIAN_POINT ( 'NONE',  ( 12.99999662536863632, -77.94228634059960825, 17.49999999999999645 ) ) ;
#3445 = EDGE_CURVE ( 'NONE', #12415, #35643, #686, .T. ) ;
#3446 = CARTESIAN_POINT ( 'NONE',  ( 124.4080600076930665, -12.15049814296675201, 32.50002500000000083 ) ) ;
#3447 = VERTEX_POINT ( 'NONE', #18185 ) ;
#3448 = VERTEX_POINT ( 'NONE', #6941 ) ;
#3449 = VECTOR ( 'NONE', #17851, 1000.000000000000000 ) ;
#3450 = CIRCLE ( 'NONE', #10031, 2.000000000000001776 ) ;
#3451 = DIRECTION ( 'NONE',  ( 0.000000000000000000, 0.000000000000000000, -1.000000000000000000 ) ) ;
#3452 = CIRCLE ( 'NONE', #31019, 2.000000000000001776 ) ;
#3453 = ORIENTED_EDGE ( 'NONE', *, *, #6651, .T. ) ;
#3454 = CARTESIAN_POINT ( 'NONE',  ( -21.64585576624245888, -107.6291973900578398, 32.50000000000000000 ) ) ;
#3455 = VERTEX_POINT ( 'NONE', #3587 ) ;
#3456 = FACE_OUTER_BOUND ( 'NONE', #5639, .T. ) ;
#3457 = VERTEX_POINT ( 'NONE', #9581 ) ;
#3458 = ORIENTED_EDGE ( 'NONE', *, *, #4537, .F. ) ;
#3459 = CIRCLE ( 'NONE', #9453, 2.000000000000000000 ) ;
#3460 = VECTOR ( 'NONE', #2532, 1000.000000000000000 ) ;
#3461 = CYLINDRICAL_SURFACE ( 'NONE', #11780, 3.500000000000003109 ) ;
#3462 = CARTESIAN_POINT ( 'NONE',  ( 0.1714266706912579152, -5.674529457426388923, -1.878862934774795823 ) ) ;
#3463 = ADVANCED_FACE ( 'NONE', ( #12564 ), #20616, .F. ) ;
#3464 = CARTESIAN_POINT ( 'NONE',  ( 64.99999662536839651, -43.30127018922199511, 12.50000000000000000 ) ) ;
#3465 = ORIENTED_EDGE ( 'NONE', *, *, #37075, .F. ) ;
#3466 = CARTESIAN_POINT ( 'NONE',  ( 44.13139720814420031, 27.49999999999988987, -10.00000000000000178 ) ) ;
#3467 = AXIS2_PLACEMENT_3D ( 'NONE', #270, #26516, #827 ) ;
#3468 = DIRECTION ( 'NONE',  ( -0.000000000000000000, -0.000000000000000000, 1.000000000000000000 ) ) ;
#3469 = DIRECTION ( 'NONE',  ( 0.4999999999999924505, -0.8660254037844429265, 0.000000000000000000 ) ) ;
#3470 = VERTEX_POINT ( 'NONE', #29815 ) ;
#3471 = CARTESIAN_POINT ( 'NONE',  ( 24.99999662536857059, 77.94228634059957983, -9.999999999999998224 ) ) ;
#3473 = CARTESIAN_POINT ( 'NONE',  ( 56.99999662536844625, -60.62177826491080168, 12.50000000000000000 ) ) ;
#3472 = AXIS2_PLACEMENT_3D ( 'NONE', #24530, #10264, #21696 ) ;
#3474 = ORIENTED_EDGE ( 'NONE', *, *, #27292, .F. ) ;
#3475 = DIRECTION ( 'NONE',  ( -0.000000000000000000, -0.000000000000000000, 1.000000000000000000 ) ) ;
#3476 = AXIS2_PLACEMENT_3D ( 'NONE', #10985, #5195, #16826 ) ;
#3477 = CARTESIAN_POINT ( 'NONE',  ( -18.00000337463123046, 86.60254037844397601, -9.999999999999998224 ) ) ;
#3478 = LINE ( 'NONE', #26349, #22592 ) ;
#3480 = VECTOR ( 'NONE', #24309, 1000.000000000000000 ) ;
#3479 = CARTESIAN_POINT ( 'NONE',  ( -10.00000337463127842, -69.28203230275519786, 17.49999999999999645 ) ) ;
#3481 = EDGE_CURVE ( 'NONE', #24271, #10050, #34822, .T. ) ;
#3482 = DIRECTION ( 'NONE',  ( 1.000000000000000000, 0.000000000000000000, 0.000000000000000000 ) ) ;
#3483 = AXIS2_PLACEMENT_3D ( 'NONE', #32431, #20607, #23825 ) ;
#3484 = DIRECTION ( 'NONE',  ( 1.000000000000000000, 0.000000000000000000, 0.000000000000000000 ) ) ;
#3485 = ORIENTED_EDGE ( 'NONE', *, *, #29941, .T. ) ;
#3486 = ADVANCED_FACE ( 'NONE', ( #24019 ), #35464, .T. ) ;
#3487 = CARTESIAN_POINT ( 'NONE',  ( 70.80619744049005249, 84.18124734178236679, 27.50000000000000000 ) ) ;
#3488 = CARTESIAN_POINT ( 'NONE',  ( 0.000000000000000000, 0.000000000000000000, 2.266666666666999674 ) ) ;
#3489 = DIRECTION ( 'NONE',  ( 0.000000000000000000, 0.000000000000000000, 1.000000000000000000 ) ) ;
#3490 = EDGE_LOOP ( 'NONE', ( #31243, #21509, #9417, #11187 ) ) ;
#3491 = CIRCLE ( 'NONE', #11269, 4.700000000000000178 ) ;
#3492 = ORIENTED_EDGE ( 'NONE', *, *, #17442, .F. ) ;
#3493 = ORIENTED_EDGE ( 'NONE', *, *, #8225, .F. ) ;
#3494 = CARTESIAN_POINT ( 'NONE',  ( 67.99999662536838230, 34.64101615137758472, 12.50000000000000000 ) ) ;
#3495 = FACE_OUTER_BOUND ( 'NONE', #19885, .T. ) ;
#3496 = EDGE_CURVE ( 'NONE', #18808, #28322, #18055, .T. ) ;
#3497 = CARTESIAN_POINT ( 'NONE',  ( 54.99999662536846046, -43.30127018922200222, 12.50000000000000000 ) ) ;
#3498 = AXIS2_PLACEMENT_3D ( 'NONE', #6049, #3220, #14649 ) ;
#3499 = CIRCLE ( 'NONE', #22050, 2.000000000000000000 ) ;
#3500 = CARTESIAN_POINT ( 'NONE',  ( 32.99999662536853862, 77.94228634059959404, -9.999999999999998224 ) ) ;
#3501 = EDGE_LOOP ( 'NONE', ( #18075, #4481 ) ) ;
#3502 = DIRECTION ( 'NONE',  ( 0.000000000000000000, 0.000000000000000000, 1.000000000000000000 ) ) ;
#3503 = EDGE_LOOP ( 'NONE', ( #19832, #16387, #30975, #20074, #33416, #34688, #17333, #26568, #26235, #1193, #10198, #1495, #16110, #25708, #16757, #13808, #27140, #16838, #31913, #3804, #10124, #19565, #36063, #26828 ) ) ;
#3504 = AXIS2_PLACEMENT_3D ( 'NONE', #6565, #12148, #24002 ) ;
#3505 = FACE_BOUND ( 'NONE', #35164, .T. ) ;
#3506 = EDGE_CURVE ( 'NONE', #22424, #23506, #2488, .T. ) ;
#3507 = AXIS2_PLACEMENT_3D ( 'NONE', #33679, #36853, #31396 ) ;
#3508 = EDGE_CURVE ( 'NONE', #17720, #15986, #76, .T. ) ;
#3509 = AXIS2_PLACEMENT_3D ( 'NONE', #17764, #29555, #35020 ) ;
#3510 = CARTESIAN_POINT ( 'NONE',  ( -35.00000337463116296, 77.94228634059957983, -9.999999999999998224 ) ) ;
#3511 = EDGE_CURVE ( 'NONE', #5353, #18222, #30609, .T. ) ;
#3512 = ADVANCED_FACE ( 'NONE', ( #4322 ), #36383, .F. ) ;
#3513 = CARTESIAN_POINT ( 'NONE',  ( -73.00000337463097821, 25.98076211353318854, 17.49999999999999645 ) ) ;
#3514 = VERTEX_POINT ( 'NONE', #24944 ) ;
#3515 = FACE_OUTER_BOUND ( 'NONE', #18788, .T. ) ;
#3516 = PRODUCT_CONTEXT ( 'NONE', #17321, 'mechanical' ) ;
#3517 = AXIS2_PLACEMENT_3D ( 'NONE', #7695, #7884, #16491 ) ;
#3518 = DIRECTION ( 'NONE',  ( -1.000000000000000000, 0.000000000000000000, 0.000000000000000000 ) ) ;
#3519 = CARTESIAN_POINT ( 'NONE',  ( -50.00000337463109190, 51.96152422706637708, -9.999999999999998224 ) ) ;
#3520 = LINE ( 'NONE', #12098, #568 ) ;
#3521 = ORIENTED_EDGE ( 'NONE', *, *, #12132, .T. ) ;
#3522 = DIRECTION ( 'NONE',  ( 1.000000000000000000, 0.000000000000000000, 0.000000000000000000 ) ) ;
#3523 = DIRECTION ( 'NONE',  ( 1.000000000000000000, 0.000000000000000000, 0.000000000000000000 ) ) ;
#3524 = DIRECTION ( 'NONE',  ( 1.000000000000000000, 0.000000000000000000, 0.000000000000000000 ) ) ;
#3525 = ORIENTED_EDGE ( 'NONE', *, *, #10328, .F. ) ;
#3526 = ORIENTED_EDGE ( 'NONE', *, *, #1103, .T. ) ;
#3527 = AXIS2_PLACEMENT_3D ( 'NONE', #29023, #34312, #20047 ) ;
#3528 = ORIENTED_EDGE ( 'NONE', *, *, #26953, .F. ) ;
#3529 = AXIS2_PLACEMENT_3D ( 'NONE', #297, #2960, #14388 ) ;
#3530 = DIRECTION ( 'NONE',  ( -0.000000000000000000, -0.000000000000000000, 1.000000000000000000 ) ) ;
#3531 = EDGE_CURVE ( 'NONE', #6894, #10997, #10692, .T. ) ;
#3532 = CARTESIAN_POINT ( 'NONE',  ( 39.27785635698568711, 86.50000000000001421, 32.50000000000000000 ) ) ;
#3533 = AXIS2_PLACEMENT_3D ( 'NONE', #25782, #31745, #14884 ) ;
#3534 = DIRECTION ( 'NONE',  ( 0.000000000000000000, 0.000000000000000000, 1.000000000000000000 ) ) ;
#3535 = CARTESIAN_POINT ( 'NONE',  ( 70.80619744048946984, -84.18124734178287838, 32.50000000000000000 ) ) ;
#3536 = DIRECTION ( 'NONE',  ( -0.000000000000000000, -0.000000000000000000, -1.000000000000000000 ) ) ;
#3538 = DIRECTION ( 'NONE',  ( -0.000000000000000000, -0.000000000000000000, 1.000000000000000000 ) ) ;
#3537 = AXIS2_PLACEMENT_3D ( 'NONE', #5802, #20034, #11040 ) ;
#3539 = ORIENTED_EDGE ( 'NONE', *, *, #16911, .F. ) ;
#3540 = ORIENTED_EDGE ( 'NONE', *, *, #26107, .F. ) ;
#3541 = DIRECTION ( 'NONE',  ( 0.000000000000000000, 0.000000000000000000, 1.000000000000000000 ) ) ;
#3542 = AXIS2_PLACEMENT_3D ( 'NONE', #14386, #17550, #31792 ) ;
#3543 = DIRECTION ( 'NONE',  ( 1.000000000000000000, 0.000000000000000000, 0.000000000000000000 ) ) ;
#3544 = AXIS2_PLACEMENT_3D ( 'NONE', #17912, #23920, #3279 ) ;
#3545 = FACE_OUTER_BOUND ( 'NONE', #15002, .T. ) ;
#3546 = ORIENTED_EDGE ( 'NONE', *, *, #44, .T. ) ;
#3547 = FACE_BOUND ( 'NONE', #29513, .T. ) ;
#3548 = AXIS2_PLACEMENT_3D ( 'NONE', #25112, #4676, #5219 ) ;
#3549 = ORIENTED_EDGE ( 'NONE', *, *, #31767, .T. ) ;
#3550 = ORIENTED_EDGE ( 'NONE', *, *, #19687, .F. ) ;
#3551 = EDGE_CURVE ( 'NONE', #20954, #12074, #12643, .T. ) ;
#3552 = CIRCLE ( 'NONE', #24519, 33.00000000000001421 ) ;
#3553 = DIRECTION ( 'NONE',  ( 1.000000000000000000, 0.000000000000000000, 0.000000000000000000 ) ) ;
#3554 = ORIENTED_EDGE ( 'NONE', *, *, #25836, .F. ) ;
#3555 = CARTESIAN_POINT ( 'NONE',  ( -75.00000337463100664, -43.30127018922202353, -9.999999999999998224 ) ) ;
#3556 = LINE ( 'NONE', #14990, #12526 ) ;
#3557 = FACE_BOUND ( 'NONE', #264, .T. ) ;
#3558 = AXIS2_PLACEMENT_3D ( 'NONE', #31282, #17035, #28469 ) ;
#3559 = VERTEX_POINT ( 'NONE', #25141 ) ;
#3560 = VERTEX_POINT ( 'NONE', #24388 ) ;
#3561 = VERTEX_POINT ( 'NONE', #22134 ) ;
#3562 = ORIENTED_EDGE ( 'NONE', *, *, #1567, .T. ) ;
#3563 = AXIS2_PLACEMENT_3D ( 'NONE', #1052, #17740, #502 ) ;
#3564 = ORIENTED_EDGE ( 'NONE', *, *, #6531, .T. ) ;
#3565 = CARTESIAN_POINT ( 'NONE',  ( -45.00000337463111322, 77.94228634059959404, 17.49999999999999645 ) ) ;
#3567 = CARTESIAN_POINT ( 'NONE',  ( -86.45172111230354517, 31.46585318596159553, -49.86348611802629449 ) ) ;
#3566 = CIRCLE ( 'NONE', #1076, 2.000000000000001776 ) ;
#3568 = ORIENTED_EDGE ( 'NONE', *, *, #23168, .T. ) ;
#3569 = PLANE ( 'NONE',  #34638 ) ;
#3570 = CARTESIAN_POINT ( 'NONE',  ( 92.89147506197157611, 70.24558514894413008, 32.49999999999999289 ) ) ;
#3571 = FACE_OUTER_BOUND ( 'NONE', #9966, .T. ) ;
#3572 = EDGE_CURVE ( 'NONE', #3470, #35481, #27638, .T. ) ;
#3573 = ORIENTED_EDGE ( 'NONE', *, *, #3705, .F. ) ;
#3574 = CARTESIAN_POINT ( 'NONE',  ( 0.000000000000000000, 0.000000000000000000, -4.599999999999999645 ) ) ;
#3575 = EDGE_CURVE ( 'NONE', #4901, #14195, #23440, .T. ) ;
#3576 = DIRECTION ( 'NONE',  ( -0.000000000000000000, -0.000000000000000000, 1.000000000000000000 ) ) ;
#3577 = DIRECTION ( 'NONE',  ( 1.000000000000000000, 0.000000000000000000, 0.000000000000000000 ) ) ;
#3578 = ORIENTED_EDGE ( 'NONE', *, *, #8649, .T. ) ;
#3579 = DIRECTION ( 'NONE',  ( 0.000000000000000000, 0.000000000000000000, 1.000000000000000000 ) ) ;
#3580 = CIRCLE ( 'NONE', #7789, 2.000000000000001776 ) ;
#3581 = DIRECTION ( 'NONE',  ( 0.000000000000000000, 0.000000000000000000, 1.000000000000000000 ) ) ;
#3582 = VERTEX_POINT ( 'NONE', #27376 ) ;
#3583 = ORIENTED_EDGE ( 'NONE', *, *, #20457, .T. ) ;
#3584 = EDGE_CURVE ( 'NONE', #29631, #18343, #33577, .T. ) ;
#3585 = CARTESIAN_POINT ( 'NONE',  ( 5.750000000000035527, 83.21147890756138565, 32.49999999999999289 ) ) ;
#3586 = DIRECTION ( 'NONE',  ( 1.000000000000000000, 0.000000000000000000, 0.000000000000000000 ) ) ;
#3587 = CARTESIAN_POINT ( 'NONE',  ( -110.2237710830543733, -101.7384897088139724, 32.50000000000000000 ) ) ;
#3588 = DIRECTION ( 'NONE',  ( -0.000000000000000000, -0.000000000000000000, 1.000000000000000000 ) ) ;
#3589 = ORIENTED_EDGE ( 'NONE', *, *, #33507, .F. ) ;
#3590 = CARTESIAN_POINT ( 'NONE',  ( 77.99999662536833966, 17.32050807568879236, -9.999999999999998224 ) ) ;
#3591 = CARTESIAN_POINT ( 'NONE',  ( 56.99999662536844625, 60.62177826491077326, -5.000000000000000000 ) ) ;
#3592 = VERTEX_POINT ( 'NONE', #16490 ) ;
#3593 = AXIS2_PLACEMENT_3D ( 'NONE', #60, #17317, #22933 ) ;
#3594 = ADVANCED_FACE ( 'NONE', ( #7883 ), #30732, .F. ) ;
#3595 = LINE ( 'NONE', #22912, #27362 ) ;
#3596 = AXIS2_PLACEMENT_3D ( 'NONE', #15212, #33026, #3969 ) ;
#3597 = ORIENTED_EDGE ( 'NONE', *, *, #13848, .F. ) ;
#3598 = DIRECTION ( 'NONE',  ( 0.000000000000000000, 0.000000000000000000, 1.000000000000000000 ) ) ;
#3599 = DIRECTION ( 'NONE',  ( 0.000000000000000000, 0.000000000000000000, 1.000000000000000000 ) ) ;
#3600 = AXIS2_PLACEMENT_3D ( 'NONE', #11159, #25613, #29142 ) ;
#3601 = LINE ( 'NONE', #3057, #11251 ) ;
#3602 = ORIENTED_EDGE ( 'NONE', *, *, #9371, .T. ) ;
#3603 = EDGE_LOOP ( 'NONE', ( #13637, #908, #34139, #192 ) ) ;
#3604 = CIRCLE ( 'NONE', #17976, 2.541999999999999815 ) ;
#3605 = DIRECTION ( 'NONE',  ( 0.000000000000000000, 0.000000000000000000, 1.000000000000000000 ) ) ;
#3606 = CARTESIAN_POINT ( 'NONE',  ( -65.00000337463104927, -43.30127018922202353, 12.50000000000000000 ) ) ;
#3607 = DIRECTION ( 'NONE',  ( 0.000000000000000000, 0.000000000000000000, 1.000000000000000000 ) ) ;
#3608 = ORIENTED_EDGE ( 'NONE', *, *, #10532, .F. ) ;
#3609 = CYLINDRICAL_SURFACE ( 'NONE', #5189, 2.000000000000001776 ) ;
#3610 = EDGE_CURVE ( 'NONE', #23016, #19957, #4881, .T. ) ;
#3611 = FACE_BOUND ( 'NONE', #34955, .T. ) ;
#3612 = FACE_OUTER_BOUND ( 'NONE', #9599, .T. ) ;
#3613 = CARTESIAN_POINT ( 'NONE',  ( -75.00000337463097821, 8.660254037844374864, -5.000000000000000000 ) ) ;
#3614 = CARTESIAN_POINT ( 'NONE',  ( -22.00000337463122690, 86.60254037844397601, -5.000000000000000000 ) ) ;
#3615 = EDGE_LOOP ( 'NONE', ( #16192, #3857 ) ) ;
#3616 = LINE ( 'NONE', #23308, #28459 ) ;
#3617 = LINE ( 'NONE', #782, #24566 ) ;
#3618 = VECTOR ( 'NONE', #23063, 1000.000000000000000 ) ;
#3619 = VERTEX_POINT ( 'NONE', #36188 ) ;
#3620 = LINE ( 'NONE', #34760, #36407 ) ;
#3621 = ADVANCED_FACE ( 'NONE', ( #10492 ), #16144, .F. ) ;
#3622 = FACE_BOUND ( 'NONE', #25500, .T. ) ;
#3623 = AXIS2_PLACEMENT_3D ( 'NONE', #8029, #33730, #28099 ) ;
#3624 = DIRECTION ( 'NONE',  ( 0.000000000000000000, 0.000000000000000000, 1.000000000000000000 ) ) ;
#3625 = ORIENTED_EDGE ( 'NONE', *, *, #8745, .F. ) ;
#3626 = VERTEX_POINT ( 'NONE', #5052 ) ;
#3627 = ORIENTED_EDGE ( 'NONE', *, *, #11949, .T. ) ;
#3628 = EDGE_CURVE ( 'NONE', #27334, #36171, #19253, .T. ) ;
#3629 = CARTESIAN_POINT ( 'NONE',  ( -90.00000337463090716, -1.040834085586084257E-14, -5.000000000000000000 ) ) ;
#3630 = CARTESIAN_POINT ( 'NONE',  ( 101.7384897088151234, 110.2237710830533217, 32.55002500000000509 ) ) ;
#3631 = DIRECTION ( 'NONE',  ( 0.000000000000000000, 0.4999999999999991118, -0.8660254037844391517 ) ) ;
#3632 = ORIENTED_EDGE ( 'NONE', *, *, #9070, .T. ) ;
#3633 = ORIENTED_EDGE ( 'NONE', *, *, #19962, .F. ) ;
#3634 = ORIENTED_EDGE ( 'NONE', *, *, #17630, .T. ) ;
#3635 = DIRECTION ( 'NONE',  ( 0.000000000000000000, 0.000000000000000000, 1.000000000000000000 ) ) ;
#3636 = ORIENTED_EDGE ( 'NONE', *, *, #7763, .T. ) ;
#3637 = CARTESIAN_POINT ( 'NONE',  ( -8.711298609632770251, -118.4422998056053160, 32.50000000000000000 ) ) ;
#3638 = EDGE_LOOP ( 'NONE', ( #22948, #34679 ) ) ;
#3639 = DIRECTION ( 'NONE',  ( 1.000000000000000000, 0.000000000000000000, 0.000000000000000000 ) ) ;
#3640 = ORIENTED_EDGE ( 'NONE', *, *, #12272, .F. ) ;
#3641 = EDGE_LOOP ( 'NONE', ( #7283, #7896 ) ) ;
#3642 = ADVANCED_FACE ( 'NONE', ( #13303 ), #18755, .F. ) ;
#3643 = CARTESIAN_POINT ( 'NONE',  ( -65.00000337463102085, 43.30127018922198801, -9.999999999999998224 ) ) ;
#3644 = FACE_BOUND ( 'NONE', #12085, .T. ) ;
#3646 = AXIS2_PLACEMENT_3D ( 'NONE', #15180, #26611, #12918 ) ;
#3645 = LINE ( 'NONE', #15074, #20651 ) ;
#3647 = ORIENTED_EDGE ( 'NONE', *, *, #24373, .F. ) ;
#3648 = ORIENTED_EDGE ( 'NONE', *, *, #10882, .F. ) ;
#3649 = CARTESIAN_POINT ( 'NONE',  ( 34.99999662536855283, -60.62177826491080168, -9.999999999999998224 ) ) ;
#3650 = EDGE_CURVE ( 'NONE', #4700, #34182, #32420, .T. ) ;
#3651 = CARTESIAN_POINT ( 'NONE',  ( -28.99999999999998934, 103.4105893997321886, -11.00000000000000355 ) ) ;
#3652 = DIRECTION ( 'NONE',  ( 1.000000000000000000, 0.000000000000000000, 0.000000000000000000 ) ) ;
#3653 = ORIENTED_EDGE ( 'NONE', *, *, #33769, .F. ) ;
#3654 = DIRECTION ( 'NONE',  ( 1.000000000000000000, 0.000000000000000000, 0.000000000000000000 ) ) ;
#3655 = CARTESIAN_POINT ( 'NONE',  ( 96.53048327204960799, 102.5304832720492527, 27.50000000000000000 ) ) ;
#3657 = EDGE_LOOP ( 'NONE', ( #3539, #19970 ) ) ;
#3656 = EDGE_CURVE ( 'NONE', #23102, #9991, #9662, .T. ) ;
#3658 = CARTESIAN_POINT ( 'NONE',  ( 6.123233995736731770E-16, -145.0000000000000568, 27.50000000000000000 ) ) ;
#3659 = CARTESIAN_POINT ( 'NONE',  ( -82.27241335952113843, 47.50000000000096634, 32.50002500000000083 ) ) ;
#3660 = CARTESIAN_POINT ( 'NONE',  ( 79.99999662536833966, 34.64101615137759183, 12.50000000000000000 ) ) ;
#3661 = CARTESIAN_POINT ( 'NONE',  ( 7.999996625368656744, -86.60254037844400443, 12.50000000000000000 ) ) ;
#3662 = CARTESIAN_POINT ( 'NONE',  ( -10.00000337463128730, 69.28203230275516944, -9.999999999999998224 ) ) ;
#3663 = DIRECTION ( 'NONE',  ( 0.000000000000000000, 0.000000000000000000, 1.000000000000000000 ) ) ;
#3664 = ORIENTED_EDGE ( 'NONE', *, *, #34211, .F. ) ;
#3665 = CYLINDRICAL_SURFACE ( 'NONE', #7038, 3.000000000000002665 ) ;
#3666 = DIRECTION ( 'NONE',  ( 1.000000000000000000, 0.000000000000000000, 0.000000000000000000 ) ) ;
#3667 = LINE ( 'NONE', #23535, #34360 ) ;
#3668 = ORIENTED_EDGE ( 'NONE', *, *, #26855, .T. ) ;
#3669 = ORIENTED_EDGE ( 'NONE', *, *, #5032, .T. ) ;
#3670 = VERTEX_POINT ( 'NONE', #18587 ) ;
#3671 = EDGE_CURVE ( 'NONE', #13923, #18360, #21743, .T. ) ;
#3672 = PRESENTATION_STYLE_ASSIGNMENT (( #20716 ) ) ;
#3673 = CARTESIAN_POINT ( 'NONE',  ( -5.000000000000000000, 25.00000000000000000, 15.00000000000000000 ) ) ;
#3674 = CYLINDRICAL_SURFACE ( 'NONE', #24280, 2.000000000000001776 ) ;
#3675 = CARTESIAN_POINT ( 'NONE',  ( 72.99999662536835388, -43.30127018922199511, -9.999999999999998224 ) ) ;
#3676 = CARTESIAN_POINT ( 'NONE',  ( 9.999996625368618552, 69.28203230275516944, -9.999999999999998224 ) ) ;
#3677 = ORIENTED_EDGE ( 'NONE', *, *, #12616, .F. ) ;
#3678 = APPLICATION_CONTEXT ( 'automotive_design' ) ;
#3679 = FACE_OUTER_BOUND ( 'NONE', #21697, .T. ) ;
#3680 = ORIENTED_EDGE ( 'NONE', *, *, #34602, .F. ) ;
#3681 = FACE_BOUND ( 'NONE', #19890, .T. ) ;
#3682 = ADVANCED_FACE ( 'NONE', ( #31115 ), #33748, .F. ) ;
#3683 = DIRECTION ( 'NONE',  ( 1.000000000000000000, 0.000000000000000000, 0.000000000000000000 ) ) ;
#3684 =( NAMED_UNIT ( * ) SI_UNIT ( $, .STERADIAN. ) SOLID_ANGLE_UNIT ( ) );
#3685 = EDGE_CURVE ( 'NONE', #12225, #19686, #9285, .T. ) ;
#3686 = ORIENTED_EDGE ( 'NONE', *, *, #17001, .T. ) ;
#3687 = CARTESIAN_POINT ( 'NONE',  ( 5.248984340851194474, 2.531668808681894145, -4.266868479993926044 ) ) ;
#3688 = VECTOR ( 'NONE', #7497, 1000.000000000000000 ) ;
#3689 = DIRECTION ( 'NONE',  ( 0.000000000000000000, 0.000000000000000000, 1.000000000000000000 ) ) ;
#3690 = EDGE_CURVE ( 'NONE', #18793, #15817, #11417, .T. ) ;
#3691 = CARTESIAN_POINT ( 'NONE',  ( 29.99999662536856349, 69.28203230275518365, -9.999999999999998224 ) ) ;
#3692 = CARTESIAN_POINT ( 'NONE',  ( -45.00000000000000000, 0.000000000000000000, 15.00000000000000000 ) ) ;
#3693 = CARTESIAN_POINT ( 'NONE',  ( -30.00000337463118427, 69.28203230275516944, -9.999999999999998224 ) ) ;
#3694 = VERTEX_POINT ( 'NONE', #22861 ) ;
#3695 = LINE ( 'NONE', #26386, #7025 ) ;
#3696 = EDGE_CURVE ( 'NONE', #24370, #5854, #12082, .T. ) ;
#3697 = DIRECTION ( 'NONE',  ( -1.000000000000000000, 0.000000000000000000, 0.000000000000000000 ) ) ;
#3698 = CARTESIAN_POINT ( 'NONE',  ( 26.99999662536856704, 77.94228634059957983, 17.49999999999999645 ) ) ;
#3699 = EDGE_CURVE ( 'NONE', #31147, #31233, #15060, .T. ) ;
#3700 = EDGE_LOOP ( 'NONE', ( #1070, #30331 ) ) ;
#3701 = ORIENTED_EDGE ( 'NONE', *, *, #7925, .T. ) ;
#3702 = ORIENTED_EDGE ( 'NONE', *, *, #23999, .T. ) ;
#3703 = DIRECTION ( 'NONE',  ( 0.000000000000000000, -1.000000000000000000, 1.034244904716769672E-15 ) ) ;
#3704 = CARTESIAN_POINT ( 'NONE',  ( 0.000000000000000000, 0.000000000000000000, -4.599999999999999645 ) ) ;
#3705 = EDGE_CURVE ( 'NONE', #18803, #19499, #34987, .T. ) ;
#3706 = EDGE_CURVE ( 'NONE', #8132, #8981, #22854, .T. ) ;
#3707 = DIRECTION ( 'NONE',  ( 1.000000000000000000, 0.000000000000000000, 0.000000000000000000 ) ) ;
#3708 = EDGE_CURVE ( 'NONE', #10163, #33312, #36618, .T. ) ;
#3709 = AXIS2_PLACEMENT_3D ( 'NONE', #33632, #7935, #36074 ) ;
#3710 = ADVANCED_FACE ( 'NONE', ( #36740 ), #28287, .F. ) ;
#3711 = CARTESIAN_POINT ( 'NONE',  ( -3.374631327851540519E-06, 86.60254037844397601, -5.000000000000000000 ) ) ;
#3712 = CARTESIAN_POINT ( 'NONE',  ( 102.5304832720496080, 102.5304832720492527, 32.50000000000000000 ) ) ;
#3713 = EDGE_CURVE ( 'NONE', #24720, #15837, #2803, .T. ) ;
#3714 = CARTESIAN_POINT ( 'NONE',  ( 74.99999662536835388, -43.30127018922199511, -9.999999999999998224 ) ) ;
#3715 = ORIENTED_EDGE ( 'NONE', *, *, #27481, .F. ) ;
#3716 = EDGE_LOOP ( 'NONE', ( #30677, #7672, #10091, #21475, #15396, #15031 ) ) ;
#3717 = DIRECTION ( 'NONE',  ( 1.000000000000000000, 0.000000000000000000, 0.000000000000000000 ) ) ;
#3718 = DIRECTION ( 'NONE',  ( 1.000000000000000000, 0.000000000000000000, 0.000000000000000000 ) ) ;
#3719 = ORIENTED_EDGE ( 'NONE', *, *, #22834, .F. ) ;
#3720 = CARTESIAN_POINT ( 'NONE',  ( 74.99999662536836809, 43.30127018922198801, 12.50000000000000000 ) ) ;
#3721 = ORIENTED_EDGE ( 'NONE', *, *, #11363, .F. ) ;
#3722 = FACE_BOUND ( 'NONE', #11433, .T. ) ;
#3723 = ORIENTED_EDGE ( 'NONE', *, *, #31276, .T. ) ;
#3724 = ORIENTED_EDGE ( 'NONE', *, *, #25866, .T. ) ;
#3725 = DIRECTION ( 'NONE',  ( 0.000000000000000000, 0.000000000000000000, 1.000000000000000000 ) ) ;
#3726 = ORIENTED_EDGE ( 'NONE', *, *, #24604, .F. ) ;
#3727 = DIRECTION ( 'NONE',  ( 0.000000000000000000, 0.000000000000000000, -1.000000000000000000 ) ) ;
#3728 = CIRCLE ( 'NONE', #34281, 2.000000000000001776 ) ;
#3729 = FACE_OUTER_BOUND ( 'NONE', #11059, .T. ) ;
#3730 = DIRECTION ( 'NONE',  ( 0.000000000000000000, 0.000000000000000000, 1.000000000000000000 ) ) ;
#3731 = ORIENTED_EDGE ( 'NONE', *, *, #16812, .F. ) ;
#3732 = ORIENTED_EDGE ( 'NONE', *, *, #29115, .F. ) ;
#3733 = VERTEX_POINT ( 'NONE', #15103 ) ;
#3734 = ORIENTED_EDGE ( 'NONE', *, *, #934, .T. ) ;
#3735 = VERTEX_POINT ( 'NONE', #2608 ) ;
#3736 = CARTESIAN_POINT ( 'NONE',  ( -80.00000337463094979, -2.428612866367529932E-14, -5.000000000000000000 ) ) ;
#3737 = CARTESIAN_POINT ( 'NONE',  ( 77.99999662536833966, 34.64101615137759183, -9.999999999999998224 ) ) ;
#3738 = ORIENTED_EDGE ( 'NONE', *, *, #19930, .F. ) ;
#3739 = DIRECTION ( 'NONE',  ( 1.000000000000000000, 0.000000000000000000, 0.000000000000000000 ) ) ;
#3740 = CARTESIAN_POINT ( 'NONE',  ( 105.2117281555539705, 57.76803422138092259, 32.50000000000000711 ) ) ;
#3741 = LINE ( 'NONE', #6567, #6973 ) ;
#3742 = ORIENTED_EDGE ( 'NONE', *, *, #18105, .F. ) ;
#3743 = FACE_OUTER_BOUND ( 'NONE', #7188, .T. ) ;
#3744 = AXIS2_PLACEMENT_3D ( 'NONE', #2292, #5478, #8300 ) ;
#3745 = CYLINDRICAL_SURFACE ( 'NONE', #36600, 2.000000000000001776 ) ;
#3746 = EDGE_CURVE ( 'NONE', #716, #29611, #11438, .T. ) ;
#3747 = CARTESIAN_POINT ( 'NONE',  ( 66.99999662536839651, 60.62177826491078747, -9.999999999999998224 ) ) ;
#3748 = ORIENTED_EDGE ( 'NONE', *, *, #15092, .F. ) ;
#3749 = CARTESIAN_POINT ( 'NONE',  ( 55.27226924886075921, -77.26562141134597539, 32.50000000000000000 ) ) ;
#3750 = CARTESIAN_POINT ( 'NONE',  ( 34.99999662536855283, -60.62177826491080168, 12.50000000000000000 ) ) ;
#3751 = VERTEX_POINT ( 'NONE', #8431 ) ;
#3752 = ORIENTED_EDGE ( 'NONE', *, *, #19894, .F. ) ;
#3753 = CYLINDRICAL_SURFACE ( 'NONE', #31976, 2.000000000000001776 ) ;
#3754 = DIRECTION ( 'NONE',  ( 0.000000000000000000, 0.000000000000000000, 1.000000000000000000 ) ) ;
#3755 = DIRECTION ( 'NONE',  ( -1.000000000000000000, 0.000000000000000000, 0.000000000000000000 ) ) ;
#3756 = DIRECTION ( 'NONE',  ( 1.000000000000000000, 0.000000000000000000, 0.000000000000000000 ) ) ;
#3757 = ORIENTED_EDGE ( 'NONE', *, *, #13202, .F. ) ;
#3758 = CARTESIAN_POINT ( 'NONE',  ( -30.00000337463118427, 69.28203230275516944, 12.50000000000000000 ) ) ;
#3759 = DIRECTION ( 'NONE',  ( 0.000000000000000000, 0.000000000000000000, 1.000000000000000000 ) ) ;
#3760 = ORIENTED_EDGE ( 'NONE', *, *, #12376, .T. ) ;
#3761 = DIRECTION ( 'NONE',  ( -0.000000000000000000, -0.000000000000000000, 1.000000000000000000 ) ) ;
#3762 = EDGE_LOOP ( 'NONE', ( #8508, #22112 ) ) ;
#3763 = EDGE_CURVE ( 'NONE', #3694, #34519, #5253, .T. ) ;
#3764 = DIRECTION ( 'NONE',  ( 0.000000000000000000, 0.000000000000000000, 1.000000000000000000 ) ) ;
#3765 = CIRCLE ( 'NONE', #21140, 2.999999999999999556 ) ;
#3766 = DIRECTION ( 'NONE',  ( -1.000000000000000000, 0.000000000000000000, 0.000000000000000000 ) ) ;
#3767 = DIRECTION ( 'NONE',  ( 0.000000000000000000, 0.000000000000000000, 1.000000000000000000 ) ) ;
#3768 = ORIENTED_EDGE ( 'NONE', *, *, #3231, .T. ) ;
#3769 = ORIENTED_EDGE ( 'NONE', *, *, #32301, .T. ) ;
#3770 = CARTESIAN_POINT ( 'NONE',  ( 70.80619744049005249, 84.18124734178236679, 32.50000000000000000 ) ) ;
#3771 = VERTEX_POINT ( 'NONE', #672 ) ;
#3772 = DIRECTION ( 'NONE',  ( 1.000000000000000000, 0.000000000000000000, 0.000000000000000000 ) ) ;
#3773 = CIRCLE ( 'NONE', #1987, 2.000000000000001776 ) ;
#3774 = CARTESIAN_POINT ( 'NONE',  ( 0.000000000000000000, 0.000000000000000000, 17.49999999999999645 ) ) ;
#3775 = CARTESIAN_POINT ( 'NONE',  ( -31.09745072740852123, -83.47442710120346021, 12.49999999999999645 ) ) ;
#3776 = DIRECTION ( 'NONE',  ( -0.000000000000000000, -0.000000000000000000, 1.000000000000000000 ) ) ;
#3777 = CARTESIAN_POINT ( 'NONE',  ( -32.16008401677954254, -61.25926521283091830, -49.22241343995298024 ) ) ;
#3778 = EDGE_LOOP ( 'NONE', ( #24758, #15893 ) ) ;
#3779 = DIRECTION ( 'NONE',  ( 0.000000000000000000, 0.000000000000000000, -1.000000000000000000 ) ) ;
#3780 = B_SPLINE_CURVE_WITH_KNOTS ( 'NONE', 3,
 ( #15796, #23677, #26875, #35135, #12605, #20871, #24059, #15230, #18992, #24993, #13903, #16185, #36431, #18800, #24627, #30218, #19352, #33787, #16544, #10738 ),
 .UNSPECIFIED., .F., .F.,
 ( 4, 2, 2, 2, 2, 2, 2, 2, 2, 4 ),
 ( 2.781148923622390442E-07, 0.0008372784139766601373, 0.001674278713060957900, 0.002511279012145256097, 0.003348279311229553860, 0.003766779460771703825, 0.004185279610313853357, 0.005022279909398152421, 0.005859280208482451485, 0.006696280507566749682 ),
 .UNSPECIFIED. ) ;
#3781 = SURFACE_SIDE_STYLE ('',( #11655 ) ) ;
#3782 = EDGE_CURVE ( 'NONE', #13768, #7831, #21651, .T. ) ;
#3783 =( NAMED_UNIT ( * ) SI_UNIT ( $, .STERADIAN. ) SOLID_ANGLE_UNIT ( ) );
#3784 = ORIENTED_EDGE ( 'NONE', *, *, #6674, .T. ) ;
#3785 = DIRECTION ( 'NONE',  ( -1.000000000000000000, 0.000000000000000000, 0.000000000000000000 ) ) ;
#3786 = DIRECTION ( 'NONE',  ( 0.000000000000000000, 0.000000000000000000, 1.000000000000000000 ) ) ;
#3787 = AXIS2_PLACEMENT_3D ( 'NONE', #33656, #7958, #36825 ) ;
#3788 = DIRECTION ( 'NONE',  ( 1.000000000000000000, 0.000000000000000000, 0.000000000000000000 ) ) ;
#3789 = VERTEX_POINT ( 'NONE', #36923 ) ;
#3790 = AXIS2_PLACEMENT_3D ( 'NONE', #10491, #22133, #30731 ) ;
#3791 = ORIENTED_EDGE ( 'NONE', *, *, #21551, .F. ) ;
#3792 = CARTESIAN_POINT ( 'NONE',  ( 0.000000000000000000, -1.467624384280027172, 2.542000000000001592 ) ) ;
#3793 = CARTESIAN_POINT ( 'NONE',  ( -10.00000337463127842, -69.28203230275519786, -5.000000000000000000 ) ) ;
#3794 = DIRECTION ( 'NONE',  ( 0.000000000000000000, 0.000000000000000000, 1.000000000000000000 ) ) ;
#3795 = EDGE_LOOP ( 'NONE', ( #532, #22246 ) ) ;
#3796 = ORIENTED_EDGE ( 'NONE', *, *, #31417, .F. ) ;
#3797 = VERTEX_POINT ( 'NONE', #19491 ) ;
#3798 = AXIS2_PLACEMENT_3D ( 'NONE', #21850, #2868, #33290 ) ;
#3799 = DIRECTION ( 'NONE',  ( -0.000000000000000000, -0.000000000000000000, 1.000000000000000000 ) ) ;
#3800 = CIRCLE ( 'NONE', #4991, 2.000000000000001776 ) ;
#3801 = EDGE_LOOP ( 'NONE', ( #16195, #9358 ) ) ;
#3802 = EDGE_CURVE ( 'NONE', #2177, #8794, #20032, .T. ) ;
#3803 = CARTESIAN_POINT ( 'NONE',  ( -20.26379314223832395, -109.7460900736713540, 32.49999999999999289 ) ) ;
#3804 = ORIENTED_EDGE ( 'NONE', *, *, #16288, .T. ) ;
#3805 = DIRECTION ( 'NONE',  ( 1.000000000000000000, 0.000000000000000000, 0.000000000000000000 ) ) ;
#3806 = EDGE_LOOP ( 'NONE', ( #1209, #3217, #5314, #6545 ) ) ;
#3807 = EDGE_CURVE ( 'NONE', #21828, #12432, #26428, .T. ) ;
#3808 = CIRCLE ( 'NONE', #25368, 2.000000000000001776 ) ;
#3809 = ORIENTED_EDGE ( 'NONE', *, *, #15029, .F. ) ;
#3810 = DIRECTION ( 'NONE',  ( -1.000000000000000000, 0.000000000000000000, 0.000000000000000000 ) ) ;
#3811 = CARTESIAN_POINT ( 'NONE',  ( 66.99999662536839651, -60.62177826491080168, -9.999999999999998224 ) ) ;
#3812 = EDGE_LOOP ( 'NONE', ( #18038, #12025, #16189, #35900 ) ) ;
#3813 = EDGE_CURVE ( 'NONE', #14280, #12923, #31229, .T. ) ;
#3814 = ORIENTED_EDGE ( 'NONE', *, *, #18805, .F. ) ;
#3815 = CARTESIAN_POINT ( 'NONE',  ( 71.99999662536839651, -3.469446951953614189E-15, -9.999999999999998224 ) ) ;
#3816 = CARTESIAN_POINT ( 'NONE',  ( 5.122341571230611734, 2.957385285031201239, -4.281776566113604687 ) ) ;
#3817 = DIRECTION ( 'NONE',  ( -0.000000000000000000, -0.000000000000000000, 1.000000000000000000 ) ) ;
#3818 = DIRECTION ( 'NONE',  ( 0.000000000000000000, 0.000000000000000000, -1.000000000000000000 ) ) ;
#3819 = ADVANCED_FACE ( 'NONE', ( #28664 ), #2439, .T. ) ;
#3820 = ORIENTED_EDGE ( 'NONE', *, *, #13282, .F. ) ;
#3821 = FACE_OUTER_BOUND ( 'NONE', #10290, .T. ) ;
#3822 = CARTESIAN_POINT ( 'NONE',  ( -2.503857664561936813E-16, -5.773502691896267081, -6.000000000000000000 ) ) ;
#3823 = EDGE_LOOP ( 'NONE', ( #19189, #13639, #4459, #25732, #19468 ) ) ;
#3824 = CARTESIAN_POINT ( 'NONE',  ( 0.000000000000000000, 0.000000000000000000, 27.50000000000000000 ) ) ;
#3825 = DIRECTION ( 'NONE',  ( -0.000000000000000000, -0.000000000000000000, 1.000000000000000000 ) ) ;
#3826 = PLANE ( 'NONE',  #21979 ) ;
#3827 = CARTESIAN_POINT ( 'NONE',  ( -5.999999999999998224, -145.0000000000000568, 32.55002500000000509 ) ) ;
#3828 = CIRCLE ( 'NONE', #22403, 30.00000000000001421 ) ;
#3829 = CARTESIAN_POINT ( 'NONE',  ( 101.7384897088143560, -110.2237710830540180, 27.50000000000000000 ) ) ;
#3830 = VECTOR ( 'NONE', #20435, 1000.000000000000000 ) ;
#3831 = CARTESIAN_POINT ( 'NONE',  ( -86.45172111230354517, 31.46585318596159553, -4.999999999999997335 ) ) ;
#3832 = ORIENTED_EDGE ( 'NONE', *, *, #21506, .F. ) ;
#3833 = DIRECTION ( 'NONE',  ( -1.000000000000000000, 0.000000000000000000, 0.000000000000000000 ) ) ;
#3834 = DIRECTION ( 'NONE',  ( 0.000000000000000000, 0.000000000000000000, 1.000000000000000000 ) ) ;
#3835 = CARTESIAN_POINT ( 'NONE',  ( -65.00000337463104927, -43.30127018922202353, 17.49999999999999645 ) ) ;
#3836 = ORIENTED_EDGE ( 'NONE', *, *, #35591, .F. ) ;
#3837 = EDGE_CURVE ( 'NONE', #7714, #8170, #23736, .T. ) ;
#3838 = ORIENTED_EDGE ( 'NONE', *, *, #27411, .F. ) ;
#3839 = VERTEX_POINT ( 'NONE', #1406 ) ;
#3840 = DIRECTION ( 'NONE',  ( -0.000000000000000000, -0.000000000000000000, -1.000000000000000000 ) ) ;
#3841 = CARTESIAN_POINT ( 'NONE',  ( 57.99999662536843914, -34.64101615137759893, 17.49999999999999645 ) ) ;
#3842 = CARTESIAN_POINT ( 'NONE',  ( 84.99999662536831124, -8.660254037844397956, 12.50000000000000000 ) ) ;
#3843 = EDGE_CURVE ( 'NONE', #21147, #5770, #23311, .T. ) ;
#3844 =( GEOMETRIC_REPRESENTATION_CONTEXT ( 3 ) GLOBAL_UNCERTAINTY_ASSIGNED_CONTEXT ( ( #33178 ) ) GLOBAL_UNIT_ASSIGNED_CONTEXT ( ( #285, #3119, #34628 ) ) REPRESENTATION_CONTEXT ( 'NONE', 'WORKASPACE' ) );
#3845 = CARTESIAN_POINT ( 'NONE',  ( 79.99999662536833966, -3.469446951953614189E-15, 12.50000000000000000 ) ) ;
#3846 = CARTESIAN_POINT ( 'NONE',  ( 149.8799519615616020, -6.000000000000508038, 32.55002500000000509 ) ) ;
#3847 = ORIENTED_EDGE ( 'NONE', *, *, #26135, .T. ) ;
#3848 = ADVANCED_FACE ( 'NONE', ( #1236 ), #7235, .F. ) ;
#3849 = CARTESIAN_POINT ( 'NONE',  ( 55.27226924886075921, -77.26562141134598960, 27.50000000000000000 ) ) ;
#3850 = EDGE_LOOP ( 'NONE', ( #26634, #10376, #24662, #5165, #17182, #35032, #5481, #168, #33522, #25667, #19228, #22128, #12935, #9351, #21001, #14227 ) ) ;
#3851 = FACE_BOUND ( 'NONE', #26506, .T. ) ;
#3852 = AXIS2_PLACEMENT_3D ( 'NONE', #28679, #25154, #8443 ) ;
#3853 = VECTOR ( 'NONE', #8795, 1000.000000000000000 ) ;
#3854 = CARTESIAN_POINT ( 'NONE',  ( 0.000000000000000000, 0.000000000000000000, -15.00000000000000000 ) ) ;
#3855 = AXIS2_PLACEMENT_3D ( 'NONE', #15743, #2236, #27166 ) ;
#3856 = CARTESIAN_POINT ( 'NONE',  ( -59.13646009116099833, 70.47608876694653190, 12.49999999999999822 ) ) ;
#3857 = ORIENTED_EDGE ( 'NONE', *, *, #3551, .T. ) ;
#3858 = CARTESIAN_POINT ( 'NONE',  ( -78.00000337463094979, 34.64101615137757051, -9.999999999999998224 ) ) ;
#3859 = DIRECTION ( 'NONE',  ( 0.000000000000000000, 0.000000000000000000, 1.000000000000000000 ) ) ;
#3860 = CARTESIAN_POINT ( 'NONE',  ( -57.00000337463107059, 43.30127018922197379, 17.49999999999999645 ) ) ;
#3861 = EDGE_CURVE ( 'NONE', #29787, #9742, #30985, .T. ) ;
#3862 = CIRCLE ( 'NONE', #863, 2.000000000000001776 ) ;
#3863 = CARTESIAN_POINT ( 'NONE',  ( -72.00000337463100664, -2.404119930384582903E-14, 17.49999999999999645 ) ) ;
#3864 = CARTESIAN_POINT ( 'NONE',  ( -50.00000337463112032, -51.96152422706641971, 17.49999999999999645 ) ) ;
#3865 = ORIENTED_EDGE ( 'NONE', *, *, #16134, .T. ) ;
#3866 = CARTESIAN_POINT ( 'NONE',  ( 72.72667006429115588, 101.6652913307178636, 27.50000000000000000 ) ) ;
#3867 = CIRCLE ( 'NONE', #18234, 2.000000000000001776 ) ;
#3868 = CARTESIAN_POINT ( 'NONE',  ( 0.000000000000000000, 98.60827697811544112, -19.99999999999999645 ) ) ;
#3869 = CARTESIAN_POINT ( 'NONE',  ( 34.99999662536855283, -77.94228634059960825, 17.49999999999999645 ) ) ;
#3870 = ORIENTED_EDGE ( 'NONE', *, *, #18751, .F. ) ;
#3871 = VECTOR ( 'NONE', #23270, 1000.000000000000000 ) ;
#3872 = VERTEX_POINT ( 'NONE', #12653 ) ;
#3873 = ORIENTED_EDGE ( 'NONE', *, *, #16935, .T. ) ;
#3874 = LINE ( 'NONE', #29386, #27318 ) ;
#3875 = CYLINDRICAL_SURFACE ( 'NONE', #34529, 2.000000000000001776 ) ;
#3876 = CIRCLE ( 'NONE', #258, 2.000000000000001776 ) ;
#3877 = AXIS2_PLACEMENT_3D ( 'NONE', #33943, #31124, #25315 ) ;
#3878 = CARTESIAN_POINT ( 'NONE',  ( 0.000000000000000000, 0.000000000000000000, 27.50000000000000000 ) ) ;
#3879 = EDGE_CURVE ( 'NONE', #30974, #985, #10151, .T. ) ;
#3880 = DIRECTION ( 'NONE',  ( 1.000000000000000000, 0.000000000000000000, 0.000000000000000000 ) ) ;
#3881 = CARTESIAN_POINT ( 'NONE',  ( 0.000000000000000000, 0.000000000000000000, -5.700000000000000178 ) ) ;
#3882 = EDGE_CURVE ( 'NONE', #4744, #14689, #24525, .T. ) ;
#3883 = DIRECTION ( 'NONE',  ( 0.6439740589782694258, 0.7650473262243666639, 0.000000000000000000 ) ) ;
#3884 = ORIENTED_EDGE ( 'NONE', *, *, #5109, .T. ) ;
#3885 = ADVANCED_FACE ( 'NONE', ( #18283 ), #35929, .F. ) ;
#3886 = ORIENTED_EDGE ( 'NONE', *, *, #27351, .T. ) ;
#3887 = DIRECTION ( 'NONE',  ( 1.000000000000000000, 0.000000000000000000, 0.000000000000000000 ) ) ;
#3888 = AXIS2_PLACEMENT_3D ( 'NONE', #9689, #20733, #32170 ) ;
#3889 = FACE_OUTER_BOUND ( 'NONE', #31067, .T. ) ;
#3890 = ORIENTED_EDGE ( 'NONE', *, *, #18021, .T. ) ;
#3891 = CIRCLE ( 'NONE', #18267, 2.000000000000001776 ) ;
#3892 = EDGE_CURVE ( 'NONE', #19957, #27668, #7152, .T. ) ;
#3893 = ORIENTED_EDGE ( 'NONE', *, *, #812, .F. ) ;
#3894 = EDGE_CURVE ( 'NONE', #23537, #9788, #17932, .T. ) ;
#3895 = CIRCLE ( 'NONE', #24270, 17.55872235085560007 ) ;
#3896 = DIRECTION ( 'NONE',  ( 0.000000000000000000, 0.000000000000000000, 1.000000000000000000 ) ) ;
#3897 = ORIENTED_EDGE ( 'NONE', *, *, #28920, .T. ) ;
#3898 = ORIENTED_EDGE ( 'NONE', *, *, #12393, .T. ) ;
#3899 = PLANE ( 'NONE',  #33818 ) ;
#3900 = ORIENTED_EDGE ( 'NONE', *, *, #12178, .F. ) ;
#3901 = EDGE_CURVE ( 'NONE', #30601, #1442, #34110, .T. ) ;
#3902 =( NAMED_UNIT ( * ) SI_UNIT ( $, .STERADIAN. ) SOLID_ANGLE_UNIT ( ) );
#3903 = AXIS2_PLACEMENT_3D ( 'NONE', #6307, #14391, #3518 ) ;
#3904 = EDGE_CURVE ( 'NONE', #21416, #30265, #32718, .T. ) ;
#3905 = DIRECTION ( 'NONE',  ( 1.000000000000000000, 0.000000000000000000, 0.000000000000000000 ) ) ;
#3906 = EDGE_CURVE ( 'NONE', #26494, #1764, #37102, .T. ) ;
#3907 = FACE_OUTER_BOUND ( 'NONE', #34314, .T. ) ;
#3908 = DIRECTION ( 'NONE',  ( 0.000000000000000000, 0.000000000000000000, 1.000000000000000000 ) ) ;
#3909 = ORIENTED_EDGE ( 'NONE', *, *, #33038, .T. ) ;
#3910 = ORIENTED_EDGE ( 'NONE', *, *, #16650, .T. ) ;
#3911 = ORIENTED_EDGE ( 'NONE', *, *, #21136, .F. ) ;
#3912 = ORIENTED_EDGE ( 'NONE', *, *, #29505, .T. ) ;
#3913 = ORIENTED_EDGE ( 'NONE', *, *, #13313, .T. ) ;
#3915 = DIRECTION ( 'NONE',  ( 0.000000000000000000, 0.000000000000000000, 1.000000000000000000 ) ) ;
#3914 = CIRCLE ( 'NONE', #28454, 2.000000000000001776 ) ;
#3916 = DIRECTION ( 'NONE',  ( 3.554796214472773777E-16, 1.000000000000000000, 0.000000000000000000 ) ) ;
#3917 = VERTEX_POINT ( 'NONE', #4243 ) ;
#3918 = AXIS2_PLACEMENT_3D ( 'NONE', #25029, #8331, #10934 ) ;
#3919 = CARTESIAN_POINT ( 'NONE',  ( 81.99999662536833966, 17.32050807568879236, -9.999999999999998224 ) ) ;
#3920 = CARTESIAN_POINT ( 'NONE',  ( 77.93337901593585570, 72.12093275448846441, 32.50001250000000397 ) ) ;
#3921 = CARTESIAN_POINT ( 'NONE',  ( 9.999996625368655856, -69.28203230275519786, 17.49999999999999645 ) ) ;
#3922 = AXIS2_PLACEMENT_3D ( 'NONE', #14082, #17294, #11459 ) ;
#3923 = VERTEX_POINT ( 'NONE', #12469 ) ;
#3924 = VECTOR ( 'NONE', #26447, 1000.000000000000000 ) ;
#3925 = LINE ( 'NONE', #9924, #26641 ) ;
#3926 = AXIS2_PLACEMENT_3D ( 'NONE', #36875, #16997, #11184 ) ;
#3927 = DIRECTION ( 'NONE',  ( 0.000000000000000000, 0.000000000000000000, 1.000000000000000000 ) ) ;
#3928 = EDGE_CURVE ( 'NONE', #29624, #10165, #32920, .T. ) ;
#3929 = DIRECTION ( 'NONE',  ( 0.000000000000000000, -0.000000000000000000, -1.000000000000000000 ) ) ;
#3930 = ORIENTED_EDGE ( 'NONE', *, *, #1391, .F. ) ;
#3931 = DIRECTION ( 'NONE',  ( 0.000000000000000000, 0.000000000000000000, 1.000000000000000000 ) ) ;
#3932 = EDGE_CURVE ( 'NONE', #35812, #19005, #32358, .T. ) ;
#3933 = DIRECTION ( 'NONE',  ( 1.000000000000000000, 0.000000000000000000, 0.000000000000000000 ) ) ;
#3934 = ORIENTED_EDGE ( 'NONE', *, *, #16860, .F. ) ;
#3935 = CIRCLE ( 'NONE', #27272, 2.000000000000001776 ) ;
#3936 = ORIENTED_EDGE ( 'NONE', *, *, #17223, .F. ) ;
#3937 = CARTESIAN_POINT ( 'NONE',  ( -34.60911769017402406, 75.98085615278088767, -5.000000000000000000 ) ) ;
#3938 = LINE ( 'NONE', #15382, #25940 ) ;
#3939 = DIRECTION ( 'NONE',  ( -1.000000000000000000, 1.773272886554068598E-14, 0.000000000000000000 ) ) ;
#3940 = DIRECTION ( 'NONE',  ( 0.000000000000000000, 0.000000000000000000, 1.000000000000000000 ) ) ;
#3941 = EDGE_CURVE ( 'NONE', #12218, #22555, #1766, .T. ) ;
#3942 = ORIENTED_EDGE ( 'NONE', *, *, #5104, .T. ) ;
#3943 = VECTOR ( 'NONE', #19020, 1000.000000000000000 ) ;
#3944 = DIRECTION ( 'NONE',  ( -0.000000000000000000, -0.000000000000000000, 1.000000000000000000 ) ) ;
#3945 = CARTESIAN_POINT ( 'NONE',  ( -2.500000000000000444, 3.061616997868383634E-16, 1.716666666667001406 ) ) ;
#3946 = AXIS2_PLACEMENT_3D ( 'NONE', #21461, #10217, #13564 ) ;
#3947 = VERTEX_POINT ( 'NONE', #6673 ) ;
#3948 = AXIS2_PLACEMENT_3D ( 'NONE', #178, #26255, #26610 ) ;
#3949 = STYLED_ITEM ( 'NONE', ( #24763 ), #20178 ) ;
#3950 = FACE_OUTER_BOUND ( 'NONE', #9162, .T. ) ;
#3951 = ORIENTED_EDGE ( 'NONE', *, *, #31804, .T. ) ;
#3952 = VECTOR ( 'NONE', #30376, 999.9999999999998863 ) ;
#3953 = EDGE_CURVE ( 'NONE', #14173, #3447, #27472, .T. ) ;
#3954 = CIRCLE ( 'NONE', #21321, 4.999999999999997335 ) ;
#3955 = DIRECTION ( 'NONE',  ( 1.000000000000000000, 0.000000000000000000, 0.000000000000000000 ) ) ;
#3956 = VECTOR ( 'NONE', #20517, 1000.000000000000000 ) ;
#3957 = EDGE_CURVE ( 'NONE', #18237, #20586, #14937, .T. ) ;
#3958 = CARTESIAN_POINT ( 'NONE',  ( -70.00000337463102085, -34.64101615137762025, 12.50000000000000000 ) ) ;
#3959 = CIRCLE ( 'NONE', #20729, 3.500000000000003109 ) ;
#3960 = EDGE_CURVE ( 'NONE', #11611, #2623, #8933, .T. ) ;
#3961 = CARTESIAN_POINT ( 'NONE',  ( 3.447886558751866115, 3.782864459065575780, -0.7348938709837807837 ) ) ;
#3962 = ADVANCED_FACE ( 'NONE', ( #8149 ), #22391, .F. ) ;
#3963 = ORIENTED_EDGE ( 'NONE', *, *, #17637, .F. ) ;
#3964 = ORIENTED_EDGE ( 'NONE', *, *, #23229, .F. ) ;
#3965 = AXIS2_PLACEMENT_3D ( 'NONE', #13085, #24543, #35980 ) ;
#3966 = CARTESIAN_POINT ( 'NONE',  ( -90.00000337463090716, -1.040834085586084257E-14, 12.50000000000000000 ) ) ;
#3967 = ORIENTED_EDGE ( 'NONE', *, *, #16998, .T. ) ;
#3968 = DIRECTION ( 'NONE',  ( -1.000000000000000000, 0.000000000000000000, 0.000000000000000000 ) ) ;
#3969 = DIRECTION ( 'NONE',  ( 1.000000000000000000, 0.000000000000000000, 0.000000000000000000 ) ) ;
#3970 = LINE ( 'NONE', #6607, #19644 ) ;
#3971 = DIRECTION ( 'NONE',  ( 0.000000000000000000, 0.000000000000000000, 1.000000000000000000 ) ) ;
#3972 = CARTESIAN_POINT ( 'NONE',  ( 67.99999662536836809, -34.64101615137759183, -9.999999999999998224 ) ) ;
#3973 = EDGE_LOOP ( 'NONE', ( #10488, #18734 ) ) ;
#3974 = DIRECTION ( 'NONE',  ( 0.000000000000000000, 0.000000000000000000, -1.000000000000000000 ) ) ;
#3975 = LINE ( 'NONE', #12960, #588 ) ;
#3976 = DIRECTION ( 'NONE',  ( 0.000000000000000000, 0.000000000000000000, 1.000000000000000000 ) ) ;
#3977 = ORIENTED_EDGE ( 'NONE', *, *, #915, .F. ) ;
#3978 = CARTESIAN_POINT ( 'NONE',  ( 37.50000000000000000, 103.4105893997321743, -11.00000000000000355 ) ) ;
#3979 = AXIS2_PLACEMENT_3D ( 'NONE', #17391, #25832, #17008 ) ;
#3980 = CARTESIAN_POINT ( 'NONE',  ( -42.97377950131527058, 96.90768712682508124, 18.49999999999999645 ) ) ;
#3981 = CARTESIAN_POINT ( 'NONE',  ( -83.00000337463092137, -8.660254037844422825, -9.999999999999998224 ) ) ;
#3982 = AXIS2_PLACEMENT_3D ( 'NONE', #12822, #10395, #12649 ) ;
#3983 = AXIS2_PLACEMENT_3D ( 'NONE', #9317, #20752, #29552 ) ;
#3984 = AXIS2_PLACEMENT_3D ( 'NONE', #35961, #24135, #24878 ) ;
#3985 = EDGE_CURVE ( 'NONE', #9651, #7111, #5524, .T. ) ;
#3986 = ORIENTED_EDGE ( 'NONE', *, *, #22968, .F. ) ;
#3987 = AXIS2_PLACEMENT_3D ( 'NONE', #4916, #2286, #8290 ) ;
#3988 = ORIENTED_EDGE ( 'NONE', *, *, #22035, .T. ) ;
#3989 = CIRCLE ( 'NONE', #35745, 2.000000000000001776 ) ;
#3990 = PLANE ( 'NONE',  #30670 ) ;
#3991 = CARTESIAN_POINT ( 'NONE',  ( -68.00000337463099243, -2.428612866367529932E-14, -9.999999999999998224 ) ) ;
#3992 = DIRECTION ( 'NONE',  ( 0.000000000000000000, 0.000000000000000000, 1.000000000000000000 ) ) ;
#3993 = EDGE_LOOP ( 'NONE', ( #5322, #27054, #7552, #34599 ) ) ;
#3994 = ORIENTED_EDGE ( 'NONE', *, *, #11003, .T. ) ;
#3995 = ORIENTED_EDGE ( 'NONE', *, *, #28335, .F. ) ;
#3996 = AXIS2_PLACEMENT_3D ( 'NONE', #7199, #4563, #12786 ) ;
#3997 = LINE ( 'NONE', #19192, #21297 ) ;
#3998 = EDGE_LOOP ( 'NONE', ( #32582, #34625, #5229, #2926 ) ) ;
#3999 = ORIENTED_EDGE ( 'NONE', *, *, #10536, .T. ) ;
#4000 = CARTESIAN_POINT ( 'NONE',  ( -82.00000337463094979, -17.32050807568882078, -9.999999999999998224 ) ) ;
#4001 = VERTEX_POINT ( 'NONE', #28208 ) ;
#4002 = VECTOR ( 'NONE', #29085, 1000.000000000000000 ) ;
#4003 = ORIENTED_EDGE ( 'NONE', *, *, #37031, .T. ) ;
#4004 = CARTESIAN_POINT ( 'NONE',  ( -52.00000337463112032, -51.96152422706641971, -9.999999999999998224 ) ) ;
#4005 = AXIS2_PLACEMENT_3D ( 'NONE', #34878, #9169, #20601 ) ;
#4006 = LINE ( 'NONE', #13190, #27831 ) ;
#4007 = EDGE_CURVE ( 'NONE', #7029, #30130, #19726, .T. ) ;
#4008 = ORIENTED_EDGE ( 'NONE', *, *, #19655, .F. ) ;
#4009 = EDGE_LOOP ( 'NONE', ( #23883, #2603 ) ) ;
#4010 = CYLINDRICAL_SURFACE ( 'NONE', #20893, 2.000000000000001776 ) ;
#4011 = DIRECTION ( 'NONE',  ( -0.000000000000000000, 0.000000000000000000, -1.000000000000000000 ) ) ;
#4012 = AXIS2_PLACEMENT_3D ( 'NONE', #11342, #12050, #12221 ) ;
#4013 = AXIS2_PLACEMENT_3D ( 'NONE', #21973, #15012, #3384 ) ;
#4014 = DIRECTION ( 'NONE',  ( 1.000000000000000000, 0.000000000000000000, 0.000000000000000000 ) ) ;
#4015 = DIRECTION ( 'NONE',  ( -1.000000000000000000, 0.000000000000000000, 0.000000000000000000 ) ) ;
#4016 = AXIS2_PLACEMENT_3D ( 'NONE', #28129, #31127, #7891 ) ;
#4017 = VECTOR ( 'NONE', #17362, 1000.000000000000000 ) ;
#4018 = ORIENTED_EDGE ( 'NONE', *, *, #19551, .F. ) ;
#4019 = CYLINDRICAL_SURFACE ( 'NONE', #19534, 2.000000000000001776 ) ;
#4020 = LINE ( 'NONE', #18077, #15568 ) ;
#4021 = ORIENTED_EDGE ( 'NONE', *, *, #6713, .F. ) ;
#4022 = CARTESIAN_POINT ( 'NONE',  ( 0.000000000000000000, 0.000000000000000000, 12.49999999999999822 ) ) ;
#4023 = DIRECTION ( 'NONE',  ( 1.000000000000000000, 0.000000000000000000, 0.000000000000000000 ) ) ;
#4024 = FACE_OUTER_BOUND ( 'NONE', #12787, .T. ) ;
#4025 = CARTESIAN_POINT ( 'NONE',  ( -28.99999999999998934, 103.4105893997321886, 18.49999999999999645 ) ) ;
#4026 = AXIS2_PLACEMENT_3D ( 'NONE', #29668, #29873, #16194 ) ;
#4027 = CARTESIAN_POINT ( 'NONE',  ( 2.999996625368676728, -77.94228634059960825, -5.000000000000000000 ) ) ;
#4028 = CARTESIAN_POINT ( 'NONE',  ( -70.00000337463102085, -34.64101615137762025, -9.999999999999998224 ) ) ;
#4029 = ORIENTED_EDGE ( 'NONE', *, *, #21897, .T. ) ;
#4030 = CARTESIAN_POINT ( 'NONE',  ( -77.00000337463097821, 8.660254037844374864, 17.49999999999999645 ) ) ;
#4031 = AXIS2_PLACEMENT_3D ( 'NONE', #25209, #33813, #28355 ) ;
#4032 = CARTESIAN_POINT ( 'NONE',  ( -77.00000337463100664, -43.30127018922202353, -9.999999999999998224 ) ) ;
#4033 = DIRECTION ( 'NONE',  ( 0.000000000000000000, 0.000000000000000000, 1.000000000000000000 ) ) ;
#4034 = EDGE_CURVE ( 'NONE', #17256, #17808, #13702, .T. ) ;
#4035 = AXIS2_PLACEMENT_3D ( 'NONE', #1336, #32456, #4168 ) ;
#4036 = ORIENTED_EDGE ( 'NONE', *, *, #5338, .F. ) ;
#4037 = VERTEX_POINT ( 'NONE', #8349 ) ;
#4038 = VERTEX_POINT ( 'NONE', #25048 ) ;
#4039 = CIRCLE ( 'NONE', #33971, 2.000000000000001776 ) ;
#4040 = CARTESIAN_POINT ( 'NONE',  ( -65.00000337463102085, 43.30127018922198801, 12.50000000000000000 ) ) ;
#4041 = CYLINDRICAL_SURFACE ( 'NONE', #14840, 2.000000000000001776 ) ;
#4042 = EDGE_CURVE ( 'NONE', #36464, #12455, #11136, .T. ) ;
#4043 = DIRECTION ( 'NONE',  ( -0.000000000000000000, -0.000000000000000000, -1.000000000000000000 ) ) ;
#4044 = AXIS2_PLACEMENT_3D ( 'NONE', #2531, #22227, #19408 ) ;
#4045 = AXIS2_PLACEMENT_3D ( 'NONE', #10683, #5244, #4882 ) ;
#4046 = VECTOR ( 'NONE', #13956, 1000.000000000000000 ) ;
#4047 = CARTESIAN_POINT ( 'NONE',  ( -70.00000337463099243, 34.64101615137758472, -9.999999999999998224 ) ) ;
#4048 = ADVANCED_FACE ( 'NONE', ( #24848 ), #34039, .F. ) ;
#4049 = CYLINDRICAL_SURFACE ( 'NONE', #19513, 2.000000000000000000 ) ;
#4050 = VERTEX_POINT ( 'NONE', #5357 ) ;
#4051 = DIRECTION ( 'NONE',  ( 1.000000000000000000, 0.000000000000000000, 0.000000000000000000 ) ) ;
#4052 = VERTEX_POINT ( 'NONE', #31207 ) ;
#4053 = FACE_BOUND ( 'NONE', #15529, .T. ) ;
#4054 = CIRCLE ( 'NONE', #29174, 6.532899837730827386 ) ;
#4055 = DIRECTION ( 'NONE',  ( 1.000000000000000000, 0.000000000000000000, 0.000000000000000000 ) ) ;
#4056 = CARTESIAN_POINT ( 'NONE',  ( 34.99999662536855283, -77.94228634059960825, 12.50000000000000000 ) ) ;
#4057 = AXIS2_PLACEMENT_3D ( 'NONE', #18053, #3992, #12209 ) ;
#4058 = EDGE_CURVE ( 'NONE', #16958, #13946, #30472, .T. ) ;
#4059 = EDGE_LOOP ( 'NONE', ( #3988, #26248, #5156, #26968, #33262 ) ) ;
#4060 = DIRECTION ( 'NONE',  ( 0.000000000000000000, 0.000000000000000000, -1.000000000000000000 ) ) ;
#4061 = AXIS2_PLACEMENT_3D ( 'NONE', #8555, #20525, #25635 ) ;
#4062 = AXIS2_PLACEMENT_3D ( 'NONE', #14487, #22762, #17480 ) ;
#4063 = APPLICATION_PROTOCOL_DEFINITION ( 'draft international standard', 'automotive_design', 1998, #20687 ) ;
#4064 = AXIS2_PLACEMENT_3D ( 'NONE', #3606, #35992, #19121 ) ;
#4065 = DIRECTION ( 'NONE',  ( -1.000000000000000000, -0.000000000000000000, -0.000000000000000000 ) ) ;
#4066 = VECTOR ( 'NONE', #8336, 1000.000000000000000 ) ;
#4067 = CARTESIAN_POINT ( 'NONE',  ( 81.99999662536833966, 34.64101615137759183, -5.000000000000000000 ) ) ;
#4068 = CARTESIAN_POINT ( 'NONE',  ( -104.8061974404900241, -19.22934205794863516, 27.50000000000000000 ) ) ;
#4069 = ORIENTED_EDGE ( 'NONE', *, *, #29825, .T. ) ;
#4070 = CARTESIAN_POINT ( 'NONE',  ( 0.000000000000000000, 0.000000000000000000, -5.700000000000000178 ) ) ;
#4071 = CARTESIAN_POINT ( 'NONE',  ( 3.000000000000000000, 1.467624384280029615, 2.541999999999997151 ) ) ;
#4072 = DIRECTION ( 'NONE',  ( 0.000000000000000000, 0.000000000000000000, 1.000000000000000000 ) ) ;
#4073 = EDGE_CURVE ( 'NONE', #24141, #16030, #15523, .T. ) ;
#4074 = ORIENTED_EDGE ( 'NONE', *, *, #20665, .T. ) ;
#4075 = VECTOR ( 'NONE', #19744, 1000.000000000000000 ) ;
#4076 = ORIENTED_EDGE ( 'NONE', *, *, #35356, .T. ) ;
#4077 = EDGE_CURVE ( 'NONE', #3448, #10920, #10594, .T. ) ;
#4078 = ORIENTED_EDGE ( 'NONE', *, *, #19516, .T. ) ;
#4079 = FACE_OUTER_BOUND ( 'NONE', #13353, .T. ) ;
#4080 = AXIS2_PLACEMENT_3D ( 'NONE', #11523, #9262, #22977 ) ;
#4081 = CYLINDRICAL_SURFACE ( 'NONE', #20150, 25.00000000000000000 ) ;
#4082 = EDGE_CURVE ( 'NONE', #6394, #10047, #4746, .T. ) ;
#4083 = DIRECTION ( 'NONE',  ( 1.000000000000000000, 0.000000000000000000, 0.000000000000000000 ) ) ;
#4084 = VECTOR ( 'NONE', #35649, 1000.000000000000000 ) ;
#4085 = CARTESIAN_POINT ( 'NONE',  ( -62.00000337463104927, 51.96152422706639129, -5.000000000000000000 ) ) ;
#4086 = DIRECTION ( 'NONE',  ( -1.000000000000000000, 3.554796214472773777E-16, 0.000000000000000000 ) ) ;
#4087 = EDGE_CURVE ( 'NONE', #17344, #26458, #23911, .T. ) ;
#4088 = AXIS2_PLACEMENT_3D ( 'NONE', #27269, #9491, #30088 ) ;
#4089 = CIRCLE ( 'NONE', #22665, 2.000000000000001776 ) ;
#4090 = DIRECTION ( 'NONE',  ( 0.000000000000000000, 0.000000000000000000, 1.000000000000000000 ) ) ;
#4091 = ORIENTED_EDGE ( 'NONE', *, *, #3219, .T. ) ;
#4092 = CIRCLE ( 'NONE', #12451, 2.000000000000001776 ) ;
#4093 = EDGE_LOOP ( 'NONE', ( #26561, #1331, #11056, #6068 ) ) ;
#4094 = FILL_AREA_STYLE_COLOUR ( '', #11095 ) ;
#4095 = EDGE_CURVE ( 'NONE', #27467, #15817, #27484, .T. ) ;
#4096 = AXIS2_PLACEMENT_3D ( 'NONE', #31153, #25722, #11273 ) ;
#4097 = DIRECTION ( 'NONE',  ( 1.000000000000000000, 0.000000000000000000, 0.000000000000000000 ) ) ;
#4098 = ORIENTED_EDGE ( 'NONE', *, *, #20113, .T. ) ;
#4099 = DIRECTION ( 'NONE',  ( -0.000000000000000000, -0.000000000000000000, -1.000000000000000000 ) ) ;
#4100 = ORIENTED_EDGE ( 'NONE', *, *, #1961, .F. ) ;
#4101 = LINE ( 'NONE', #19904, #14693 ) ;
#4102 = VECTOR ( 'NONE', #19017, 1000.000000000000000 ) ;
#4103 = FACE_BOUND ( 'NONE', #9350, .T. ) ;
#4104 = ORIENTED_EDGE ( 'NONE', *, *, #30013, .F. ) ;
#4105 = VERTEX_POINT ( 'NONE', #1960 ) ;
#4106 = CARTESIAN_POINT ( 'NONE',  ( 0.000000000000000000, 0.000000000000000000, 12.49999999999999822 ) ) ;
#4107 = EDGE_LOOP ( 'NONE', ( #33160, #16781 ) ) ;
#4108 = AXIS2_PLACEMENT_3D ( 'NONE', #13451, #7293, #33149 ) ;
#4109 = PRODUCT_DEFINITION_SHAPE ( 'NONE', 'NONE',  #37115 ) ;
#4110 = CARTESIAN_POINT ( 'NONE',  ( 56.67878100130369035, -27.78182860042797131, 12.49999999999999822 ) ) ;
#4111 = EDGE_CURVE ( 'NONE', #18894, #22877, #24669, .T. ) ;
#4112 = DIRECTION ( 'NONE',  ( 0.000000000000000000, 0.000000000000000000, 1.000000000000000000 ) ) ;
#4113 = DIRECTION ( 'NONE',  ( 1.000000000000000000, 0.000000000000000000, 0.000000000000000000 ) ) ;
#4114 = ORIENTED_EDGE ( 'NONE', *, *, #35127, .T. ) ;
#4115 = ORIENTED_EDGE ( 'NONE', *, *, #24219, .F. ) ;
#4116 = VECTOR ( 'NONE', #646, 1000.000000000000000 ) ;
#4117 = EDGE_LOOP ( 'NONE', ( #2456, #10368 ) ) ;
#4118 = EDGE_CURVE ( 'NONE', #20117, #14572, #13114, .T. ) ;
#4119 = VERTEX_POINT ( 'NONE', #2147 ) ;
#4120 = AXIS2_PLACEMENT_3D ( 'NONE', #18135, #15135, #3149 ) ;
#4121 = ORIENTED_EDGE ( 'NONE', *, *, #8848, .T. ) ;
#4122 = CYLINDRICAL_SURFACE ( 'NONE', #11039, 2.000000000000001776 ) ;
#4123 = CIRCLE ( 'NONE', #5949, 2.000000000000001776 ) ;
#4124 = EDGE_CURVE ( 'NONE', #32298, #30643, #10735, .T. ) ;
#4125 = CYLINDRICAL_SURFACE ( 'NONE', #20374, 2.000000000000001776 ) ;
#4126 = ORIENTED_EDGE ( 'NONE', *, *, #697, .F. ) ;
#4127 = FACE_OUTER_BOUND ( 'NONE', #10182, .T. ) ;
#4128 = DIRECTION ( 'NONE',  ( 1.000000000000000000, 0.000000000000000000, 0.000000000000000000 ) ) ;
#4129 = CARTESIAN_POINT ( 'NONE',  ( 4.279621169095998212, -62.97617850287780072, 12.49999999999999822 ) ) ;
#4130 = VECTOR ( 'NONE', #31116, 1000.000000000000000 ) ;
#4131 = VERTEX_POINT ( 'NONE', #30645 ) ;
#4132 = FACE_OUTER_BOUND ( 'NONE', #5232, .T. ) ;
#4133 = AXIS2_PLACEMENT_3D ( 'NONE', #9406, #15208, #3417 ) ;
#4134 = DIRECTION ( 'NONE',  ( -0.000000000000000000, -0.000000000000000000, 1.000000000000000000 ) ) ;
#4135 = CARTESIAN_POINT ( 'NONE',  ( 89.99999662536828282, 0.000000000000000000, 12.50000000000000000 ) ) ;
#4136 = ORIENTED_EDGE ( 'NONE', *, *, #16973, .F. ) ;
#4137 = LINE ( 'NONE', #21179, #7117 ) ;
#4138 = DIRECTION ( 'NONE',  ( 0.000000000000000000, 0.000000000000000000, 1.000000000000000000 ) ) ;
#4139 = B_SPLINE_CURVE_WITH_KNOTS ( 'NONE', 3,
 ( #14370, #14723, #26166, #25813 ),
 .UNSPECIFIED., .F., .F.,
 ( 4, 4 ),
 ( 2.380735200821679637E-07, 0.002921158011986721599 ),
 .UNSPECIFIED. ) ;
#4140 = ORIENTED_EDGE ( 'NONE', *, *, #4319, .T. ) ;
#4141 = ORIENTED_EDGE ( 'NONE', *, *, #22583, .T. ) ;
#4142 = CARTESIAN_POINT ( 'NONE',  ( 3.000000000000000000, 2.935248768560057453, -3.903127820947815962E-15 ) ) ;
#4143 = EDGE_CURVE ( 'NONE', #7742, #14131, #27649, .T. ) ;
#4144 = AXIS2_PLACEMENT_3D ( 'NONE', #17594, #905, #7468 ) ;
#4145 = CARTESIAN_POINT ( 'NONE',  ( -35.19434990244938888, 52.39915983220783602, -4.999999999999997335 ) ) ;
#4146 = CARTESIAN_POINT ( 'NONE',  ( 3.000000000000000000, -1.467624384280027172, 2.542000000000001592 ) ) ;
#4147 = DIRECTION ( 'NONE',  ( 1.000000000000000000, 0.000000000000000000, 0.000000000000000000 ) ) ;
#4148 = ORIENTED_EDGE ( 'NONE', *, *, #1310, .F. ) ;
#4149 = AXIS2_PLACEMENT_3D ( 'NONE', #9549, #23990, #4472 ) ;
#4150 = DIRECTION ( 'NONE',  ( 0.000000000000000000, 0.000000000000000000, -1.000000000000000000 ) ) ;
#4151 = CARTESIAN_POINT ( 'NONE',  ( 19.31922176934805435, 76.99660315353983719, -19.99999999999999645 ) ) ;
#4152 = VERTEX_POINT ( 'NONE', #33658 ) ;
#4153 = VECTOR ( 'NONE', #5154, 1000.000000000000000 ) ;
#4154 = DIRECTION ( 'NONE',  ( 0.000000000000000000, 0.000000000000000000, 1.000000000000000000 ) ) ;
#4155 = ORIENTED_EDGE ( 'NONE', *, *, #5133, .T. ) ;
#4156 = CARTESIAN_POINT ( 'NONE',  ( -45.00000337463112743, -60.62177826491080168, -5.000000000000000000 ) ) ;
#4157 = DIRECTION ( 'NONE',  ( 0.000000000000000000, 0.000000000000000000, 1.000000000000000000 ) ) ;
#4158 = AXIS2_PLACEMENT_3D ( 'NONE', #14422, #31120, #11583 ) ;
#4159 = EDGE_CURVE ( 'NONE', #21363, #36216, #7737, .T. ) ;
#4160 = CARTESIAN_POINT ( 'NONE',  ( 4.651285141665000289, 3.088081963278261011, -1.686035282245264444 ) ) ;
#4161 = EDGE_LOOP ( 'NONE', ( #1708, #24531, #29476, #11004 ) ) ;
#4162 = CIRCLE ( 'NONE', #6538, 2.000000000000000000 ) ;
#4163 = ADVANCED_FACE ( 'NONE', ( #20134 ), #11504, .F. ) ;
#4164 = ORIENTED_EDGE ( 'NONE', *, *, #15491, .F. ) ;
#4165 = EDGE_CURVE ( 'NONE', #22817, #32397, #17903, .T. ) ;
#4166 = VECTOR ( 'NONE', #36030, 1000.000000000000000 ) ;
#4167 = ORIENTED_EDGE ( 'NONE', *, *, #23423, .F. ) ;
#4168 = DIRECTION ( 'NONE',  ( 1.000000000000000000, 0.000000000000000000, 0.000000000000000000 ) ) ;
#4169 = CIRCLE ( 'NONE', #27530, 2.000000000000001776 ) ;
#4170 = DIRECTION ( 'NONE',  ( 0.000000000000000000, 0.000000000000000000, -1.000000000000000000 ) ) ;
#4171 = EDGE_CURVE ( 'NONE', #12033, #8275, #5344, .T. ) ;
#4172 = CYLINDRICAL_SURFACE ( 'NONE', #31011, 2.000000000000001776 ) ;
#4173 = CARTESIAN_POINT ( 'NONE',  ( -35.19434990244938888, 52.39915983220783602, -4.999999999999997335 ) ) ;
#4174 = FACE_OUTER_BOUND ( 'NONE', #6718, .T. ) ;
#4175 = EDGE_CURVE ( 'NONE', #5373, #13276, #26278, .T. ) ;
#4176 = ORIENTED_EDGE ( 'NONE', *, *, #238, .T. ) ;
#4177 = CARTESIAN_POINT ( 'NONE',  ( 69.99999662536838230, -51.96152422706639840, 12.50000000000000000 ) ) ;
#4178 = CARTESIAN_POINT ( 'NONE',  ( -43.00000337463111322, 77.94228634059959404, -9.999999999999998224 ) ) ;
#4179 = SURFACE_SIDE_STYLE ('',( #32085 ) ) ;
#4180 = VERTEX_POINT ( 'NONE', #17682 ) ;
#4181 = CARTESIAN_POINT ( 'NONE',  ( 3.000000000000000000, 1.467624384280024730, -2.542000000000001592 ) ) ;
#4182 = CARTESIAN_POINT ( 'NONE',  ( -35.00000337463116296, -60.62177826491080168, -9.999999999999998224 ) ) ;
#4183 = DIRECTION ( 'NONE',  ( -1.000000000000000000, 8.737866397512802015E-15, 0.000000000000000000 ) ) ;
#4184 = VECTOR ( 'NONE', #21104, 1000.000000000000000 ) ;
#4185 = EDGE_CURVE ( 'NONE', #25427, #11646, #25588, .T. ) ;
#4186 = ORIENTED_EDGE ( 'NONE', *, *, #17058, .T. ) ;
#4187 = ADVANCED_FACE ( 'NONE', ( #17499 ), #32105, .F. ) ;
#4188 = ORIENTED_EDGE ( 'NONE', *, *, #23547, .F. ) ;
#4189 = AXIS2_PLACEMENT_3D ( 'NONE', #36663, #20143, #23142 ) ;
#4190 = EDGE_CURVE ( 'NONE', #32632, #3470, #32262, .T. ) ;
#4191 = ADVANCED_FACE ( 'NONE', ( #28926 ), #9062, .T. ) ;
#4192 = DIRECTION ( 'NONE',  ( 0.000000000000000000, 0.000000000000000000, -1.000000000000000000 ) ) ;
#4193 = AXIS2_PLACEMENT_3D ( 'NONE', #26858, #10176, #21213 ) ;
#4194 = DIRECTION ( 'NONE',  ( 0.000000000000000000, 0.000000000000000000, 1.000000000000000000 ) ) ;
#4195 = CARTESIAN_POINT ( 'NONE',  ( 0.000000000000000000, 0.000000000000000000, -5.000000000000000000 ) ) ;
#4196 = VERTEX_POINT ( 'NONE', #8518 ) ;
#4197 = ORIENTED_EDGE ( 'NONE', *, *, #30648, .T. ) ;
#4198 = CIRCLE ( 'NONE', #6592, 5.000000000000000888 ) ;
#4199 = ORIENTED_EDGE ( 'NONE', *, *, #31119, .F. ) ;
#4200 = DIRECTION ( 'NONE',  ( 0.000000000000000000, 0.000000000000000000, -1.000000000000000000 ) ) ;
#4201 = AXIS2_PLACEMENT_3D ( 'NONE', #17519, #26153, #34241 ) ;
#4202 = EDGE_LOOP ( 'NONE', ( #25482, #5938, #4975, #24808, #36574 ) ) ;
#4203 = ORIENTED_EDGE ( 'NONE', *, *, #11586, .F. ) ;
#4204 = CIRCLE ( 'NONE', #35378, 27.00000000000001421 ) ;
#4205 = DIRECTION ( 'NONE',  ( -1.000000000000000000, 0.000000000000000000, 0.000000000000000000 ) ) ;
#4206 = ORIENTED_EDGE ( 'NONE', *, *, #36000, .T. ) ;
#4207 = ORIENTED_EDGE ( 'NONE', *, *, #21309, .F. ) ;
#4208 = CARTESIAN_POINT ( 'NONE',  ( 89.99999662536828282, 0.000000000000000000, -5.000000000000000000 ) ) ;
#4209 = CARTESIAN_POINT ( 'NONE',  ( -18.00000337463123756, -69.28203230275522628, -9.999999999999998224 ) ) ;
#4210 = ORIENTED_EDGE ( 'NONE', *, *, #27786, .T. ) ;
#4211 = EDGE_LOOP ( 'NONE', ( #23698, #1469, #4926, #31837, #5298, #11673 ) ) ;
#4212 = DIRECTION ( 'NONE',  ( 0.000000000000000000, 0.000000000000000000, 1.000000000000000000 ) ) ;
#4213 = CARTESIAN_POINT ( 'NONE',  ( 35.44550000000001688, 0.000000000000000000, 0.000000000000000000 ) ) ;
#4214 = AXIS2_PLACEMENT_3D ( 'NONE', #6445, #17885, #23688 ) ;
#4215 = DIRECTION ( 'NONE',  ( 1.000000000000000000, 0.000000000000000000, 0.000000000000000000 ) ) ;
#4216 = CARTESIAN_POINT ( 'NONE',  ( -5.244721985554689603, -2.047016837486758778, -4.175706277538008493 ) ) ;
#4217 = VERTEX_POINT ( 'NONE', #12041 ) ;
#4218 = CYLINDRICAL_SURFACE ( 'NONE', #15343, 2.000000000000001776 ) ;
#4219 = ORIENTED_EDGE ( 'NONE', *, *, #851, .T. ) ;
#4220 = AXIS2_PLACEMENT_3D ( 'NONE', #28699, #9174, #743 ) ;
#4221 = DIRECTION ( 'NONE',  ( -0.000000000000000000, 0.000000000000000000, -1.000000000000000000 ) ) ;
#4222 = FACE_OUTER_BOUND ( 'NONE', #17842, .T. ) ;
#4223 = CIRCLE ( 'NONE', #34762, 150.0000000000000284 ) ;
#4224 = CARTESIAN_POINT ( 'NONE',  ( 69.99999662536838230, -34.64101615137759183, 12.50000000000000000 ) ) ;
#4225 = DIRECTION ( 'NONE',  ( 0.000000000000000000, 0.000000000000000000, -1.000000000000000000 ) ) ;
#4226 = LINE ( 'NONE', #10576, #1484 ) ;
#4227 = DIRECTION ( 'NONE',  ( -0.000000000000000000, 0.000000000000000000, -1.000000000000000000 ) ) ;
#4228 = AXIS2_PLACEMENT_3D ( 'NONE', #26769, #1085, #11957 ) ;
#4229 = DIRECTION ( 'NONE',  ( -0.000000000000000000, -0.000000000000000000, -1.000000000000000000 ) ) ;
#4230 = ORIENTED_EDGE ( 'NONE', *, *, #10722, .F. ) ;
#4231 = DIRECTION ( 'NONE',  ( 1.000000000000000000, 0.000000000000000000, 0.000000000000000000 ) ) ;
#4232 = CYLINDRICAL_SURFACE ( 'NONE', #354, 2.000000000000001776 ) ;
#4233 = CYLINDRICAL_SURFACE ( 'NONE', #13387, 25.00000000000000000 ) ;
#4234 = EDGE_LOOP ( 'NONE', ( #22115, #32877 ) ) ;
#4235 = VERTEX_POINT ( 'NONE', #5702 ) ;
#4236 = ORIENTED_EDGE ( 'NONE', *, *, #7965, .T. ) ;
#4237 = ADVANCED_FACE ( 'NONE', ( #3253 ), #37078, .F. ) ;
#4238 = DIRECTION ( 'NONE',  ( -1.000000000000000000, -0.000000000000000000, -0.000000000000000000 ) ) ;
#4239 = DIRECTION ( 'NONE',  ( 1.000000000000000000, 0.000000000000000000, 0.000000000000000000 ) ) ;
#4240 = CYLINDRICAL_SURFACE ( 'NONE', #35229, 3.500000000000003109 ) ;
#4241 = AXIS2_PLACEMENT_3D ( 'NONE', #23876, #14871, #18218 ) ;
#4242 = ORIENTED_EDGE ( 'NONE', *, *, #4384, .T. ) ;
#4243 = CARTESIAN_POINT ( 'NONE',  ( -55.88972745734202618, -33.99999999999965894, -4.999999999999997335 ) ) ;
#4244 = CARTESIAN_POINT ( 'NONE',  ( -10.00000337463125000, -86.60254037844400443, 12.50000000000000000 ) ) ;
#4245 = VERTEX_POINT ( 'NONE', #20674 ) ;
#4246 = CARTESIAN_POINT ( 'NONE',  ( -62.33939050065184517, 13.89091430021398565, 12.49999999999999822 ) ) ;
#4247 = ORIENTED_EDGE ( 'NONE', *, *, #1221, .F. ) ;
#4248 = DIRECTION ( 'NONE',  ( -1.000000000000000000, 0.000000000000000000, 0.000000000000000000 ) ) ;
#4249 = CARTESIAN_POINT ( 'NONE',  ( 0.3000000000000016542, 0.000000000000000000, 5.000000000000000000 ) ) ;
#4250 = DIRECTION ( 'NONE',  ( 1.000000000000000000, 0.000000000000000000, 0.000000000000000000 ) ) ;
#4251 = DIRECTION ( 'NONE',  ( -0.000000000000000000, -0.000000000000000000, -1.000000000000000000 ) ) ;
#4252 = ORIENTED_EDGE ( 'NONE', *, *, #18480, .T. ) ;
#4253 = PLANE ( 'NONE',  #22465 ) ;
#4254 = EDGE_CURVE ( 'NONE', #16375, #21830, #9237, .T. ) ;
#4255 = ITEM_DEFINED_TRANSFORMATION ( 'NONE', 'NONE', #11753,  #21385 ) ;
#4256 = EDGE_CURVE ( 'NONE', #34663, #13150, #4123, .T. ) ;
#4257 = CARTESIAN_POINT ( 'NONE',  ( 0.000000000000000000, 85.61789592134881843, -27.49999999999990408 ) ) ;
#4258 = DIRECTION ( 'NONE',  ( 1.000000000000000000, 0.000000000000000000, 0.000000000000000000 ) ) ;
#4259 = FACE_OUTER_BOUND ( 'NONE', #232, .T. ) ;
#4260 = ORIENTED_EDGE ( 'NONE', *, *, #3843, .F. ) ;
#4261 = CARTESIAN_POINT ( 'NONE',  ( 0.000000000000000000, 0.000000000000000000, -5.700000000000001066 ) ) ;
#4262 = FACE_OUTER_BOUND ( 'NONE', #21189, .T. ) ;
#4263 = DIRECTION ( 'NONE',  ( 0.000000000000000000, 0.000000000000000000, 1.000000000000000000 ) ) ;
#4264 = EDGE_CURVE ( 'NONE', #30055, #3619, #14335, .T. ) ;
#4265 = ORIENTED_EDGE ( 'NONE', *, *, #34788, .F. ) ;
#4266 = AXIS2_PLACEMENT_3D ( 'NONE', #15566, #24007, #6740 ) ;
#4267 = ORIENTED_EDGE ( 'NONE', *, *, #17535, .T. ) ;
#4268 = CARTESIAN_POINT ( 'NONE',  ( -55.00000337463109901, -60.62177826491083010, -9.999999999999998224 ) ) ;
#4269 = CARTESIAN_POINT ( 'NONE',  ( 27.99999662536857414, -69.28203230275519786, -9.999999999999998224 ) ) ;
#4270 = CARTESIAN_POINT ( 'NONE',  ( 67.30619744048945563, -84.18124734178287838, 32.50000000000000000 ) ) ;
#4271 = EDGE_LOOP ( 'NONE', ( #9312, #31055, #8524, #234 ) ) ;
#4272 = ADVANCED_FACE ( 'NONE', ( #8693 ), #31559, .T. ) ;
#4273 = CYLINDRICAL_SURFACE ( 'NONE', #8610, 33.00000000000001421 ) ;
#4274 = DIRECTION ( 'NONE',  ( -0.000000000000000000, 0.000000000000000000, -1.000000000000000000 ) ) ;
#4275 = DIRECTION ( 'NONE',  ( 1.000000000000000000, 0.000000000000000000, 0.000000000000000000 ) ) ;
#4276 = CARTESIAN_POINT ( 'NONE',  ( -104.1069301565558050, 59.68452040699722261, 32.50000000000000000 ) ) ;
#4277 = ORIENTED_EDGE ( 'NONE', *, *, #595, .T. ) ;
#4278 = ORIENTED_EDGE ( 'NONE', *, *, #30046, .T. ) ;
#4279 = FACE_OUTER_BOUND ( 'NONE', #26180, .T. ) ;
#4280 = CARTESIAN_POINT ( 'NONE',  ( 21.99999662536862033, -69.28203230275519786, 12.50000000000000000 ) ) ;
#4281 = EDGE_LOOP ( 'NONE', ( #11633, #25273, #21587, #13740 ) ) ;
#4282 = DIRECTION ( 'NONE',  ( 0.000000000000000000, 0.000000000000000000, -1.000000000000000000 ) ) ;
#4283 = ORIENTED_EDGE ( 'NONE', *, *, #18796, .F. ) ;
#4284 = DIRECTION ( 'NONE',  ( 0.000000000000000000, 0.000000000000000000, 1.000000000000000000 ) ) ;
#4285 = FACE_BOUND ( 'NONE', #25163, .T. ) ;
#4286 = ORIENTED_EDGE ( 'NONE', *, *, #19810, .T. ) ;
#4287 = EDGE_LOOP ( 'NONE', ( #14624, #18513 ) ) ;
#4288 = EDGE_CURVE ( 'NONE', #36402, #12408, #16124, .T. ) ;
#4289 = CYLINDRICAL_SURFACE ( 'NONE', #28418, 2.000000000000001776 ) ;
#4290 = VERTEX_POINT ( 'NONE', #28377 ) ;
#4291 =( LENGTH_UNIT ( ) NAMED_UNIT ( * ) SI_UNIT ( .MILLI., .METRE. ) );
#4292 = CARTESIAN_POINT ( 'NONE',  ( -2.714587707229022318, 4.206234748388728129, -1.833826330805560234E-16 ) ) ;
#4293 = CARTESIAN_POINT ( 'NONE',  ( 74.99999662536835388, -25.98076211353319565, -9.999999999999998224 ) ) ;
#4294 = DIRECTION ( 'NONE',  ( 0.000000000000000000, 0.000000000000000000, 1.000000000000000000 ) ) ;
#4295 = ORIENTED_EDGE ( 'NONE', *, *, #14257, .F. ) ;
#4296 = DIRECTION ( 'NONE',  ( 0.000000000000000000, 0.000000000000000000, 1.000000000000000000 ) ) ;
#4297 = EDGE_CURVE ( 'NONE', #17677, #6217, #37030, .T. ) ;
#4298 = DIRECTION ( 'NONE',  ( 0.000000000000000000, 0.000000000000000000, 1.000000000000000000 ) ) ;
#4299 = ORIENTED_EDGE ( 'NONE', *, *, #24390, .F. ) ;
#4300 = ORIENTED_EDGE ( 'NONE', *, *, #4474, .T. ) ;
#4301 = ADVANCED_FACE ( 'NONE', ( #11871 ), #23328, .F. ) ;
#4302 = ORIENTED_EDGE ( 'NONE', *, *, #21889, .T. ) ;
#4303 = CARTESIAN_POINT ( 'NONE',  ( -18.03953374218250971, 86.20686523360116382, -5.000000000000000000 ) ) ;
#4304 = AXIS2_PLACEMENT_3D ( 'NONE', #19370, #22552, #36630 ) ;
#4305 = CARTESIAN_POINT ( 'NONE',  ( 0.000000000000000000, 1.467624384280024730, -2.542000000000001592 ) ) ;
#4306 = ORIENTED_EDGE ( 'NONE', *, *, #19034, .F. ) ;
#4307 = AXIS2_PLACEMENT_3D ( 'NONE', #23274, #190, #22901 ) ;
#4308 = DIRECTION ( 'NONE',  ( 0.000000000000000000, 0.000000000000000000, -1.000000000000000000 ) ) ;
#4309 = CARTESIAN_POINT ( 'NONE',  ( -80.00000337463094979, 17.32050807568878525, -9.999999999999998224 ) ) ;
#4310 = VERTEX_POINT ( 'NONE', #35686 ) ;
#4311 = PLANE ( 'NONE',  #33829 ) ;
#4312 = CYLINDRICAL_SURFACE ( 'NONE', #1258, 2.000000000000001776 ) ;
#4313 = DIRECTION ( 'NONE',  ( 0.000000000000000000, 0.000000000000000000, 1.000000000000000000 ) ) ;
#4314 = DIRECTION ( 'NONE',  ( 0.000000000000000000, 0.000000000000000000, -1.000000000000000000 ) ) ;
#4315 = DIRECTION ( 'NONE',  ( 0.000000000000000000, 0.000000000000000000, 1.000000000000000000 ) ) ;
#4316 = CARTESIAN_POINT ( 'NONE',  ( 62.99999662536839651, 60.62177826491078747, -5.000000000000000000 ) ) ;
#4317 = ORIENTED_EDGE ( 'NONE', *, *, #14862, .F. ) ;
#4318 = VERTEX_POINT ( 'NONE', #12781 ) ;
#4319 = EDGE_CURVE ( 'NONE', #25810, #12047, #34672, .T. ) ;
#4320 = CARTESIAN_POINT ( 'NONE',  ( -52.00000337463110611, -69.28203230275519786, -9.999999999999998224 ) ) ;
#4321 = DIRECTION ( 'NONE',  ( 0.000000000000000000, 0.000000000000000000, 1.000000000000000000 ) ) ;
#4322 = FACE_OUTER_BOUND ( 'NONE', #15200, .T. ) ;
#4323 = CARTESIAN_POINT ( 'NONE',  ( 22.99999662536859901, -77.94228634059960825, 12.50000000000000000 ) ) ;
#4324 = ORIENTED_EDGE ( 'NONE', *, *, #734, .F. ) ;
#4325 = UNCERTAINTY_MEASURE_WITH_UNIT (LENGTH_MEASURE( 1.000000000000000082E-05 ), #7421, 'distance_accuracy_value', 'NONE');
#4326 = EDGE_CURVE ( 'NONE', #20492, #27413, #25099, .T. ) ;
#4327 = CARTESIAN_POINT ( 'NONE',  ( 0.000000000000000000, 0.000000000000000000, 0.000000000000000000 ) ) ;
#4328 = CARTESIAN_POINT ( 'NONE',  ( 7.999996625368656744, -86.60254037844400443, 17.49999999999999645 ) ) ;
#4329 = ORIENTED_EDGE ( 'NONE', *, *, #11175, .F. ) ;
#4330 = CIRCLE ( 'NONE', #21692, 27.00000000000001421 ) ;
#4331 = ADVANCED_FACE ( 'NONE', ( #32482 ), #21232, .F. ) ;
#4332 = CARTESIAN_POINT ( 'NONE',  ( 0.000000000000000000, 0.000000000000000000, -5.000000000000000000 ) ) ;
#4333 = EDGE_LOOP ( 'NONE', ( #24062, #32598 ) ) ;
#4334 = LINE ( 'NONE', #18402, #6126 ) ;
#4335 = DIRECTION ( 'NONE',  ( 1.000000000000000000, 0.000000000000000000, 0.000000000000000000 ) ) ;
#4336 = CARTESIAN_POINT ( 'NONE',  ( -3.000003374631269981, -77.94228634059960825, 17.49999999999999645 ) ) ;
#4337 = ORIENTED_EDGE ( 'NONE', *, *, #2751, .T. ) ;
#4338 = ORIENTED_EDGE ( 'NONE', *, *, #13797, .T. ) ;
#4339 = AXIS2_PLACEMENT_3D ( 'NONE', #27390, #27014, #7509 ) ;
#4340 = AXIS2_PLACEMENT_3D ( 'NONE', #14828, #3754, #32041 ) ;
#4341 = EDGE_CURVE ( 'NONE', #27983, #10548, #6525, .T. ) ;
#4342 = EDGE_LOOP ( 'NONE', ( #28730, #27086, #8884, #32843, #32594 ) ) ;
#4343 = CARTESIAN_POINT ( 'NONE',  ( 0.000000000000000000, 98.60827697811544112, 27.49999999999999645 ) ) ;
#4344 = FACE_BOUND ( 'NONE', #14014, .T. ) ;
#4345 = CARTESIAN_POINT ( 'NONE',  ( -75.00000337463097821, 8.660254037844374864, -5.000000000000000000 ) ) ;
#4346 = FACE_OUTER_BOUND ( 'NONE', #21165, .T. ) ;
#4347 = DIRECTION ( 'NONE',  ( 0.000000000000000000, 0.000000000000000000, 1.000000000000000000 ) ) ;
#4348 = ORIENTED_EDGE ( 'NONE', *, *, #16881, .F. ) ;
#4349 = DIRECTION ( 'NONE',  ( 0.000000000000000000, 0.000000000000000000, 1.000000000000000000 ) ) ;
#4350 = DIRECTION ( 'NONE',  ( 0.000000000000000000, 0.000000000000000000, 1.000000000000000000 ) ) ;
#4351 = DIRECTION ( 'NONE',  ( 0.000000000000000000, 0.000000000000000000, -1.000000000000000000 ) ) ;
#4352 = EDGE_LOOP ( 'NONE', ( #26010, #33318 ) ) ;
#4353 = CARTESIAN_POINT ( 'NONE',  ( 84.99999662536831124, -8.660254037844397956, -9.999999999999998224 ) ) ;
#4354 = CARTESIAN_POINT ( 'NONE',  ( -82.00000337463094979, 34.64101615137757051, -9.999999999999998224 ) ) ;
#4355 = VERTEX_POINT ( 'NONE', #32875 ) ;
#4356 = ORIENTED_EDGE ( 'NONE', *, *, #14523, .F. ) ;
#4357 = EDGE_CURVE ( 'NONE', #29261, #36951, #802, .T. ) ;
#4358 = CARTESIAN_POINT ( 'NONE',  ( -23.00000337463120559, 77.94228634059957983, -9.999999999999998224 ) ) ;
#4359 = CARTESIAN_POINT ( 'NONE',  ( -57.00000337463111322, -43.30127018922202353, -5.000000000000000000 ) ) ;
#4360 = EDGE_CURVE ( 'NONE', #14063, #26676, #8333, .T. ) ;
#4361 = DIRECTION ( 'NONE',  ( 1.000000000000000000, 0.000000000000000000, 0.000000000000000000 ) ) ;
#4362 = ORIENTED_EDGE ( 'NONE', *, *, #34337, .F. ) ;
#4363 = ORIENTED_EDGE ( 'NONE', *, *, #23423, .T. ) ;
#4364 = ORIENTED_EDGE ( 'NONE', *, *, #23902, .T. ) ;
#4365 = EDGE_CURVE ( 'NONE', #5993, #12630, #14318, .T. ) ;
#4366 = DIRECTION ( 'NONE',  ( 0.000000000000000000, 0.000000000000000000, 1.000000000000000000 ) ) ;
#4367 = AXIS2_PLACEMENT_3D ( 'NONE', #29257, #31860, #20441 ) ;
#4368 = ORIENTED_EDGE ( 'NONE', *, *, #10515, .T. ) ;
#4370 = ADVANCED_FACE ( 'NONE', ( #6629 ), #26087, .T. ) ;
#4369 = ORIENTED_EDGE ( 'NONE', *, *, #6651, .F. ) ;
#4371 = FACE_BOUND ( 'NONE', #13107, .T. ) ;
#4372 = ORIENTED_EDGE ( 'NONE', *, *, #19297, .T. ) ;
#4373 = EDGE_CURVE ( 'NONE', #6775, #29382, #8107, .T. ) ;
#4374 = ORIENTED_EDGE ( 'NONE', *, *, #27980, .F. ) ;
#4375 = DIRECTION ( 'NONE',  ( -1.000000000000000000, 0.000000000000000000, 0.000000000000000000 ) ) ;
#4376 = CIRCLE ( 'NONE', #16953, 2.000000000000001776 ) ;
#4377 = DIRECTION ( 'NONE',  ( 1.000000000000000000, 0.000000000000000000, 0.000000000000000000 ) ) ;
#4378 = ORIENTED_EDGE ( 'NONE', *, *, #12635, .F. ) ;
#4379 = ORIENTED_EDGE ( 'NONE', *, *, #2258, .T. ) ;
#4380 = DIRECTION ( 'NONE',  ( 0.000000000000000000, 0.000000000000000000, 1.000000000000000000 ) ) ;
#4381 = CARTESIAN_POINT ( 'NONE',  ( -68.00000337463099243, 17.32050807568877460, 12.50000000000000000 ) ) ;
#4382 = ADVANCED_FACE ( 'NONE', ( #33051 ), #12213, .F. ) ;
#4383 = CYLINDRICAL_SURFACE ( 'NONE', #11462, 25.00000000000000000 ) ;
#4384 = EDGE_CURVE ( 'NONE', #10733, #13581, #27262, .T. ) ;
#4385 = CARTESIAN_POINT ( 'NONE',  ( 69.99999662536839651, 34.64101615137758472, -9.999999999999998224 ) ) ;
#4386 = ADVANCED_FACE ( 'NONE', ( #996 ), #21434, .F. ) ;
#4387 = EDGE_LOOP ( 'NONE', ( #20606, #16740, #34539, #1841, #12519, #27487, #21851, #31216, #21093, #3175, #33503, #28793, #8810, #16944, #10907, #34125, #10500, #894, #6028, #24981, #2421, #4699, #6332, #30781 ) ) ;
#4388 = CARTESIAN_POINT ( 'NONE',  ( 102.5304832720488832, -102.5304832720499633, 27.50000000000000000 ) ) ;
#4389 = ADVANCED_FACE ( 'NONE', ( #29310 ), #32669, .F. ) ;
#4390 = VERTEX_POINT ( 'NONE', #6995 ) ;
#4391 = FACE_OUTER_BOUND ( 'NONE', #2022, .T. ) ;
#4392 = ADVANCED_FACE ( 'NONE', ( #18058 ), #9632, .F. ) ;
#4393 = CARTESIAN_POINT ( 'NONE',  ( -56.67878100130369035, 27.78182860042797131, -4.999999999999997335 ) ) ;
#4394 = CYLINDRICAL_SURFACE ( 'NONE', #6420, 2.000000000000001776 ) ;
#4395 = CARTESIAN_POINT ( 'NONE',  ( -70.00000337463099243, 34.64101615137758472, -5.000000000000000000 ) ) ;
#4396 = CARTESIAN_POINT ( 'NONE',  ( 0.000000000000000000, 0.000000000000000000, 32.50000000000000000 ) ) ;
#4397 = CIRCLE ( 'NONE', #9160, 33.00000000000001421 ) ;
#4398 = DIRECTION ( 'NONE',  ( 0.000000000000000000, 0.000000000000000000, 1.000000000000000000 ) ) ;
#4399 = CARTESIAN_POINT ( 'NONE',  ( -13.00000337463125710, -77.94228634059960825, -9.999999999999998224 ) ) ;
#4400 = VERTEX_POINT ( 'NONE', #18230 ) ;
#4401 = CARTESIAN_POINT ( 'NONE',  ( -5.000000000000000000, 0.000000000000000000, -6.000000000000000000 ) ) ;
#4402 = CARTESIAN_POINT ( 'NONE',  ( -3.050000000000000711, 3.735172737399428132E-16, 2.266666666666999674 ) ) ;
#4403 = DIRECTION ( 'NONE',  ( -1.000000000000000000, 0.000000000000000000, 0.000000000000000000 ) ) ;
#4404 = CIRCLE ( 'NONE', #33136, 2.000000000000001776 ) ;
#4405 = ORIENTED_EDGE ( 'NONE', *, *, #12561, .T. ) ;
#4406 = ORIENTED_EDGE ( 'NONE', *, *, #11948, .T. ) ;
#4407 = VERTEX_POINT ( 'NONE', #29665 ) ;
#4408 = AXIS2_PLACEMENT_3D ( 'NONE', #21823, #33261, #16774 ) ;
#4409 = CARTESIAN_POINT ( 'NONE',  ( 3.000000000000000000, 2.201436576420041202, -1.271000000000003460 ) ) ;
#4410 = CARTESIAN_POINT ( 'NONE',  ( 37.50000000000000000, 103.4105893997321743, 27.49999999999999645 ) ) ;
#4411 = DIRECTION ( 'NONE',  ( -0.000000000000000000, -0.000000000000000000, 1.000000000000000000 ) ) ;
#4412 = ORIENTED_EDGE ( 'NONE', *, *, #9782, .F. ) ;
#4413 = CIRCLE ( 'NONE', #34948, 1.999999999999998224 ) ;
#4414 = DIRECTION ( 'NONE',  ( 0.000000000000000000, 0.000000000000000000, 1.000000000000000000 ) ) ;
#4415 = DIRECTION ( 'NONE',  ( 0.000000000000000000, 0.000000000000000000, -1.000000000000000000 ) ) ;
#4416 = ORIENTED_EDGE ( 'NONE', *, *, #7937, .F. ) ;
#4417 = CARTESIAN_POINT ( 'NONE',  ( -32.49191361593891969, -89.27079897466117586, -5.000000000000000000 ) ) ;
#4418 = EDGE_LOOP ( 'NONE', ( #36820, #36692 ) ) ;
#4419 = DIRECTION ( 'NONE',  ( 1.000000000000000000, 0.000000000000000000, 0.000000000000000000 ) ) ;
#4420 = CIRCLE ( 'NONE', #33151, 3.500000000000003109 ) ;
#4421 = CIRCLE ( 'NONE', #24193, 2.000000000000000000 ) ;
#4422 = CYLINDRICAL_SURFACE ( 'NONE', #21353, 25.00000000000000711 ) ;
#4423 = CARTESIAN_POINT ( 'NONE',  ( 4.654160418576254177E-15, -6.066067634115602125, -4.359491423763670603 ) ) ;
#4424 = DIRECTION ( 'NONE',  ( 0.000000000000000000, 0.000000000000000000, 1.000000000000000000 ) ) ;
#4425 = ORIENTED_EDGE ( 'NONE', *, *, #13336, .F. ) ;
#4426 = FACE_OUTER_BOUND ( 'NONE', #31737, .T. ) ;
#4427 = APPLICATION_PROTOCOL_DEFINITION ( 'draft international standard', 'automotive_design', 1998, #11816 ) ;
#4428 = AXIS2_PLACEMENT_3D ( 'NONE', #6090, #36844, #19968 ) ;
#4429 = DIRECTION ( 'NONE',  ( -1.000000000000000000, 0.000000000000000000, 0.000000000000000000 ) ) ;
#4430 = B_SPLINE_CURVE_WITH_KNOTS ( 'NONE', 3,
 ( #30594, #31687, #34511, #11802, #28503, #9010, #6022, #17610, #31313, #34327 ),
 .UNSPECIFIED., .F., .F.,
 ( 4, 2, 2, 2, 4 ),
 ( 0.000000000000000000, 0.001528561485809837566, 0.003057122971619675132, 0.004585684457429513132, 0.006114245943239348530 ),
 .UNSPECIFIED. ) ;
#4431 = EDGE_CURVE ( 'NONE', #33934, #8519, #3997, .T. ) ;
#4432 = CARTESIAN_POINT ( 'NONE',  ( 47.63139720814418610, 27.49999999999988987, -15.00000000000000000 ) ) ;
#4433 = EDGE_CURVE ( 'NONE', #15350, #36079, #30777, .T. ) ;
#4434 = DIRECTION ( 'NONE',  ( -1.000000000000000000, 0.000000000000000000, 0.000000000000000000 ) ) ;
#4435 = DIRECTION ( 'NONE',  ( 1.000000000000000000, 0.000000000000000000, 0.000000000000000000 ) ) ;
#4436 = EDGE_CURVE ( 'NONE', #28556, #16244, #25191, .T. ) ;
#4437 = ORIENTED_EDGE ( 'NONE', *, *, #26850, .F. ) ;
#4438 = DIRECTION ( 'NONE',  ( 0.000000000000000000, 0.000000000000000000, 1.000000000000000000 ) ) ;
#4439 = DIRECTION ( 'NONE',  ( 0.000000000000000000, 0.000000000000000000, 1.000000000000000000 ) ) ;
#4440 = CARTESIAN_POINT ( 'NONE',  ( 3.500000000000000888, -55.00000000000000000, -15.00000000000000000 ) ) ;
#4441 = ORIENTED_EDGE ( 'NONE', *, *, #21818, .T. ) ;
#4442 = VERTEX_POINT ( 'NONE', #2302 ) ;
#4443 = DIRECTION ( 'NONE',  ( -0.000000000000000000, 0.000000000000000000, -1.000000000000000000 ) ) ;
#4444 = CYLINDRICAL_SURFACE ( 'NONE', #3983, 2.000000000000001776 ) ;
#4445 = AXIS2_PLACEMENT_3D ( 'NONE', #30967, #8096, #25528 ) ;
#4446 = CARTESIAN_POINT ( 'NONE',  ( -145.0000000000000568, 1.518182058997189877E-12, 32.50000000000000000 ) ) ;
#4447 = ORIENTED_EDGE ( 'NONE', *, *, #16696, .T. ) ;
#4448 = DIRECTION ( 'NONE',  ( -0.000000000000000000, -0.000000000000000000, 1.000000000000000000 ) ) ;
#4449 = DIRECTION ( 'NONE',  ( 0.000000000000000000, -0.000000000000000000, 1.000000000000000000 ) ) ;
#4450 = DIRECTION ( 'NONE',  ( -0.000000000000000000, -0.000000000000000000, -1.000000000000000000 ) ) ;
#4451 = CARTESIAN_POINT ( 'NONE',  ( -86.97117154665588146, 72.12339944410946657, 32.50000000000000711 ) ) ;
#4452 = ADVANCED_FACE ( 'NONE', ( #4755 ), #7745, .F. ) ;
#4453 = VERTEX_POINT ( 'NONE', #24806 ) ;
#4454 = AXIS2_PLACEMENT_3D ( 'NONE', #8067, #8261, #36398 ) ;
#4455 = ORIENTED_EDGE ( 'NONE', *, *, #17155, .T. ) ;
#4456 = CARTESIAN_POINT ( 'NONE',  ( -85.00000337463092137, 8.660254037844389075, 17.49999999999999645 ) ) ;
#4457 = CIRCLE ( 'NONE', #34995, 3.500000000000003109 ) ;
#4458 = DIRECTION ( 'NONE',  ( -0.000000000000000000, -0.000000000000000000, -1.000000000000000000 ) ) ;
#4459 = ORIENTED_EDGE ( 'NONE', *, *, #4431, .T. ) ;
#4460 = DIRECTION ( 'NONE',  ( 0.000000000000000000, 0.000000000000000000, 1.000000000000000000 ) ) ;
#4461 = VERTEX_POINT ( 'NONE', #5308 ) ;
#4462 = CARTESIAN_POINT ( 'NONE',  ( 49.99999662536846756, -69.28203230275519786, 12.50000000000000000 ) ) ;
#4463 = EDGE_CURVE ( 'NONE', #6532, #21999, #8101, .T. ) ;
#4464 = FACE_OUTER_BOUND ( 'NONE', #34578, .T. ) ;
#4465 = EDGE_LOOP ( 'NONE', ( #2968, #15473 ) ) ;
#4466 = ORIENTED_EDGE ( 'NONE', *, *, #3237, .T. ) ;
#4467 = AXIS2_PLACEMENT_3D ( 'NONE', #11600, #8620, #34701 ) ;
#4468 = DIRECTION ( 'NONE',  ( 0.000000000000000000, 0.000000000000000000, 1.000000000000000000 ) ) ;
#4469 = ORIENTED_EDGE ( 'NONE', *, *, #22483, .T. ) ;
#4470 = DIRECTION ( 'NONE',  ( 0.000000000000000000, 0.000000000000000000, 1.000000000000000000 ) ) ;
#4471 = DIRECTION ( 'NONE',  ( -1.000000000000000000, 0.000000000000000000, 0.000000000000000000 ) ) ;
#4472 = DIRECTION ( 'NONE',  ( 1.000000000000000000, 0.000000000000000000, 0.000000000000000000 ) ) ;
#4473 = DIRECTION ( 'NONE',  ( 0.000000000000000000, 0.000000000000000000, 1.000000000000000000 ) ) ;
#4474 = EDGE_CURVE ( 'NONE', #3626, #30390, #25477, .T. ) ;
#4475 = ORIENTED_EDGE ( 'NONE', *, *, #30097, .T. ) ;
#4476 = LINE ( 'NONE', #24913, #29222 ) ;
#4477 = FACE_OUTER_BOUND ( 'NONE', #5518, .T. ) ;
#4478 = VERTEX_POINT ( 'NONE', #22181 ) ;
#4479 = VECTOR ( 'NONE', #26592, 1000.000000000000000 ) ;
#4480 = CIRCLE ( 'NONE', #6850, 2.000000000000001776 ) ;
#4481 = ORIENTED_EDGE ( 'NONE', *, *, #12721, .T. ) ;
#4482 = ORIENTED_EDGE ( 'NONE', *, *, #29871, .T. ) ;
#4483 = CARTESIAN_POINT ( 'NONE',  ( -70.00000337463099243, 34.64101615137758472, -9.999999999999998224 ) ) ;
#4484 = CIRCLE ( 'NONE', #30135, 3.000000000000002665 ) ;
#4485 = CYLINDRICAL_SURFACE ( 'NONE', #35395, 33.00000000000001421 ) ;
#4486 = EDGE_LOOP ( 'NONE', ( #32721, #6364 ) ) ;
#4487 = DIRECTION ( 'NONE',  ( 1.000000000000000000, 0.000000000000000000, 0.000000000000000000 ) ) ;
#4488 = FACE_OUTER_BOUND ( 'NONE', #18027, .T. ) ;
#4489 = DIRECTION ( 'NONE',  ( -1.000000000000000000, 0.000000000000000000, 0.000000000000000000 ) ) ;
#4490 = CARTESIAN_POINT ( 'NONE',  ( 19.99999662536861678, -69.28203230275519786, -9.999999999999998224 ) ) ;
#4491 = AXIS2_PLACEMENT_3D ( 'NONE', #29042, #31491, #565 ) ;
#4492 = EDGE_CURVE ( 'NONE', #26329, #20328, #36277, .T. ) ;
#4493 = CARTESIAN_POINT ( 'NONE',  ( -18.00000337463123756, -69.28203230275522628, 17.49999999999999645 ) ) ;
#4494 = FACE_OUTER_BOUND ( 'NONE', #21338, .T. ) ;
#4495 = CIRCLE ( 'NONE', #2724, 2.000000000000001776 ) ;
#4496 = DIRECTION ( 'NONE',  ( -0.000000000000000000, -0.000000000000000000, 1.000000000000000000 ) ) ;
#4497 = EDGE_CURVE ( 'NONE', #32590, #22230, #20091, .T. ) ;
#4498 = LINE ( 'NONE', #13678, #23232 ) ;
#4499 = ORIENTED_EDGE ( 'NONE', *, *, #7872, .T. ) ;
#4500 = CIRCLE ( 'NONE', #20064, 3.500000000000000888 ) ;
#4501 = ORIENTED_EDGE ( 'NONE', *, *, #11952, .F. ) ;
#4502 = FACE_OUTER_BOUND ( 'NONE', #10821, .T. ) ;
#4503 = DIRECTION ( 'NONE',  ( 1.000000000000000000, 0.000000000000000000, 0.000000000000000000 ) ) ;
#4504 = DIRECTION ( 'NONE',  ( 1.000000000000000000, 0.000000000000000000, 0.000000000000000000 ) ) ;
#4505 = LINE ( 'NONE', #15943, #20910 ) ;
#4506 = EDGE_CURVE ( 'NONE', #16313, #10822, #22472, .T. ) ;
#4507 = ORIENTED_EDGE ( 'NONE', *, *, #11193, .T. ) ;
#4508 = AXIS2_PLACEMENT_3D ( 'NONE', #12488, #18509, #13237 ) ;
#4509 = DIRECTION ( 'NONE',  ( -0.5000000000000101030, -0.8660254037844328234, 0.000000000000000000 ) ) ;
#4510 = AXIS2_PLACEMENT_3D ( 'NONE', #14346, #16109, #34403 ) ;
#4511 = CARTESIAN_POINT ( 'NONE',  ( 14.99999662536859901, 77.94228634059957983, -9.999999999999998224 ) ) ;
#4512 = ADVANCED_FACE ( 'NONE', ( #19357, #22348, #7921, #30427, #16550, #15997, #33792, #21988, #27428 ), #16744, .F. ) ;
#4513 = LINE ( 'NONE', #16322, #19791 ) ;
#4514 = EDGE_LOOP ( 'NONE', ( #5305, #3608, #4752, #1408 ) ) ;
#4515 = DIRECTION ( 'NONE',  ( 0.000000000000000000, 0.000000000000000000, -1.000000000000000000 ) ) ;
#4516 = ORIENTED_EDGE ( 'NONE', *, *, #19956, .F. ) ;
#4517 =( LENGTH_UNIT ( ) NAMED_UNIT ( * ) SI_UNIT ( .MILLI., .METRE. ) );
#4518 = DIRECTION ( 'NONE',  ( 0.000000000000000000, 0.000000000000000000, -1.000000000000000000 ) ) ;
#4519 = DIRECTION ( 'NONE',  ( 0.000000000000000000, 0.000000000000000000, 1.000000000000000000 ) ) ;
#4520 = CIRCLE ( 'NONE', #14083, 65.00000000000000000 ) ;
#4521 = CARTESIAN_POINT ( 'NONE',  ( -20.00000337463122690, 86.60254037844397601, 17.49999999999999645 ) ) ;
#4522 = EDGE_CURVE ( 'NONE', #6764, #23686, #17679, .T. ) ;
#4523 = ORIENTED_EDGE ( 'NONE', *, *, #19403, .F. ) ;
#4524 = AXIS2_PLACEMENT_3D ( 'NONE', #7221, #24469, #35910 ) ;
#4525 = ORIENTED_EDGE ( 'NONE', *, *, #9686, .T. ) ;
#4526 = CIRCLE ( 'NONE', #30874, 2.541999999999999815 ) ;
#4527 = AXIS2_PLACEMENT_3D ( 'NONE', #7093, #20968, #6711 ) ;
#4528 = VECTOR ( 'NONE', #24534, 1000.000000000000000 ) ;
#4529 = ORIENTED_EDGE ( 'NONE', *, *, #27213, .T. ) ;
#4530 = DIRECTION ( 'NONE',  ( -0.000000000000000000, -0.8660254037844414832, 0.4999999999999953371 ) ) ;
#4531 = FACE_BOUND ( 'NONE', #26683, .T. ) ;
#4532 = DIRECTION ( 'NONE',  ( -0.000000000000000000, -0.000000000000000000, 1.000000000000000000 ) ) ;
#4533 = DIRECTION ( 'NONE',  ( 0.000000000000000000, 0.000000000000000000, -1.000000000000000000 ) ) ;
#4534 = DIRECTION ( 'NONE',  ( 1.000000000000000000, 0.000000000000000000, 0.000000000000000000 ) ) ;
#4535 = ORIENTED_EDGE ( 'NONE', *, *, #381, .F. ) ;
#4536 = CARTESIAN_POINT ( 'NONE',  ( -2.374207310413330682E-13, -68.00000000000000000, -4.999999999999997335 ) ) ;
#4537 = EDGE_CURVE ( 'NONE', #9991, #23102, #15301, .T. ) ;
#4538 = AXIS2_PLACEMENT_3D ( 'NONE', #9318, #9879, #15134 ) ;
#4539 = CARTESIAN_POINT ( 'NONE',  ( 11.99999662536865763, -86.60254037844400443, 12.50000000000000000 ) ) ;
#4540 = EDGE_CURVE ( 'NONE', #29798, #21959, #24900, .T. ) ;
#4541 = FILL_AREA_STYLE_COLOUR ( '', #36762 ) ;
#4542 = EDGE_LOOP ( 'NONE', ( #27961, #15819, #17588, #23536, #15718 ) ) ;
#4543 = DIRECTION ( 'NONE',  ( 0.000000000000000000, 0.000000000000000000, 1.000000000000000000 ) ) ;
#4544 = DIRECTION ( 'NONE',  ( 1.000000000000000000, 0.000000000000000000, 0.000000000000000000 ) ) ;
#4545 = EDGE_LOOP ( 'NONE', ( #25726, #15749 ) ) ;
#4546 = ORIENTED_EDGE ( 'NONE', *, *, #35788, .T. ) ;
#4547 = VECTOR ( 'NONE', #19572, 1000.000000000000000 ) ;
#4548 = FACE_OUTER_BOUND ( 'NONE', #26012, .T. ) ;
#4549 = CARTESIAN_POINT ( 'NONE',  ( 7.041719095097282852E-16, 78.41276890242659192, -25.02035392823930593 ) ) ;
#4550 = AXIS2_PLACEMENT_3D ( 'NONE', #19886, #15, #8284 ) ;
#4551 = CARTESIAN_POINT ( 'NONE',  ( 62.99999662536841072, 25.98076211353318854, -5.000000000000000000 ) ) ;
#4552 = ADVANCED_FACE ( 'NONE', ( #7363 ), #36436, .F. ) ;
#4553 = ORIENTED_EDGE ( 'NONE', *, *, #23539, .F. ) ;
#4554 = EDGE_LOOP ( 'NONE', ( #24738, #8548 ) ) ;
#4555 = AXIS2_PLACEMENT_3D ( 'NONE', #34122, #25132, #28109 ) ;
#4556 = VERTEX_POINT ( 'NONE', #4560 ) ;
#4557 = CIRCLE ( 'NONE', #18925, 2.000000000000001776 ) ;
#4558 = AXIS2_PLACEMENT_3D ( 'NONE', #4244, #6495, #20929 ) ;
#4559 = CIRCLE ( 'NONE', #33296, 3.000000000000002665 ) ;
#4560 = CARTESIAN_POINT ( 'NONE',  ( -7.041719095097282852E-16, 78.44802294027068967, 32.49999999999999289 ) ) ;
#4561 = EDGE_CURVE ( 'NONE', #25776, #5222, #16511, .T. ) ;
#4562 = ORIENTED_EDGE ( 'NONE', *, *, #32948, .F. ) ;
#4563 = DIRECTION ( 'NONE',  ( 0.000000000000000000, 0.000000000000000000, 1.000000000000000000 ) ) ;
#4564 = AXIS2_PLACEMENT_3D ( 'NONE', #30674, #7993, #36684 ) ;
#4565 = ORIENTED_EDGE ( 'NONE', *, *, #18622, .F. ) ;
#4566 = VERTEX_POINT ( 'NONE', #7550 ) ;
#4567 = CIRCLE ( 'NONE', #35102, 3.000000000000002665 ) ;
#4568 = CARTESIAN_POINT ( 'NONE',  ( -48.00000337463109190, 69.28203230275518365, -5.000000000000000000 ) ) ;
#4569 = CARTESIAN_POINT ( 'NONE',  ( -58.00000337463104216, 51.96152422706639129, -5.000000000000000000 ) ) ;
#4570 = VERTEX_POINT ( 'NONE', #14636 ) ;
#4571 = ORIENTED_EDGE ( 'NONE', *, *, #11658, .F. ) ;
#4572 = DIRECTION ( 'NONE',  ( 0.000000000000000000, 0.000000000000000000, 1.000000000000000000 ) ) ;
#4573 = DIRECTION ( 'NONE',  ( 0.000000000000000000, 0.000000000000000000, -1.000000000000000000 ) ) ;
#4574 = CARTESIAN_POINT ( 'NONE',  ( 6.249999999999998224, 0.000000000000000000, 0.000000000000000000 ) ) ;
#4575 = DIRECTION ( 'NONE',  ( 0.000000000000000000, 0.000000000000000000, -1.000000000000000000 ) ) ;
#4576 = EDGE_CURVE ( 'NONE', #8984, #34090, #4526, .T. ) ;
#4577 = ORIENTED_EDGE ( 'NONE', *, *, #14913, .F. ) ;
#4578 = CARTESIAN_POINT ( 'NONE',  ( -85.00000337463092137, -25.98076211353322051, 17.49999999999999645 ) ) ;
#4579 = ORIENTED_EDGE ( 'NONE', *, *, #29895, .F. ) ;
#4580 = FACE_BOUND ( 'NONE', #4234, .T. ) ;
#4581 = DIRECTION ( 'NONE',  ( 0.000000000000000000, 0.000000000000000000, -1.000000000000000000 ) ) ;
#4582 = FACE_BOUND ( 'NONE', #31237, .T. ) ;
#4583 = AXIS2_PLACEMENT_3D ( 'NONE', #25778, #34035, #11500 ) ;
#4584 = CIRCLE ( 'NONE', #2192, 3.000000000000002665 ) ;
#4585 = LINE ( 'NONE', #24827, #34492 ) ;
#4586 = AXIS2_PLACEMENT_3D ( 'NONE', #9701, #30508, #27675 ) ;
#4587 = CARTESIAN_POINT ( 'NONE',  ( -30.00000337463119848, -69.28203230275522628, 12.50000000000000000 ) ) ;
#4588 = ADVANCED_FACE ( 'NONE', ( #25540 ), #198, .F. ) ;
#4589 = AXIS2_PLACEMENT_3D ( 'NONE', #16178, #7354, #35496 ) ;
#4590 = AXIS2_PLACEMENT_3D ( 'NONE', #25840, #17015, #129 ) ;
#4591 = CARTESIAN_POINT ( 'NONE',  ( -70.00000337463099243, 51.96152422706637708, -5.000000000000000000 ) ) ;
#4592 = EDGE_CURVE ( 'NONE', #11580, #23569, #23280, .T. ) ;
#4593 = CARTESIAN_POINT ( 'NONE',  ( 3.000000000000000000, 4.131365146527188963E-15, 2.541999999999999371 ) ) ;
#4594 = ORIENTED_EDGE ( 'NONE', *, *, #4165, .T. ) ;
#4595 = DIRECTION ( 'NONE',  ( -1.000000000000000000, 0.000000000000000000, 0.000000000000000000 ) ) ;
#4596 = EDGE_CURVE ( 'NONE', #34855, #18201, #32666, .T. ) ;
#4597 = DIRECTION ( 'NONE',  ( 0.000000000000000000, 0.000000000000000000, 1.000000000000000000 ) ) ;
#4598 = DIRECTION ( 'NONE',  ( 0.000000000000000000, 0.000000000000000000, 1.000000000000000000 ) ) ;
#4599 = ORIENTED_EDGE ( 'NONE', *, *, #25860, .T. ) ;
#4600 = CIRCLE ( 'NONE', #25546, 27.00000000000001421 ) ;
#4601 = EDGE_LOOP ( 'NONE', ( #22253, #28291, #24183, #9520 ) ) ;
#4602 = ORIENTED_EDGE ( 'NONE', *, *, #13796, .T. ) ;
#4603 = DIRECTION ( 'NONE',  ( -1.000000000000000000, 0.000000000000000000, 0.000000000000000000 ) ) ;
#4604 = CARTESIAN_POINT ( 'NONE',  ( 59.99999662536843914, -34.64101615137759893, -9.999999999999998224 ) ) ;
#4605 = ORIENTED_EDGE ( 'NONE', *, *, #19753, .T. ) ;
#4606 = CARTESIAN_POINT ( 'NONE',  ( -52.39915983220772233, -35.19434990244957362, -4.999999999999997335 ) ) ;
#4607 = EDGE_CURVE ( 'NONE', #4052, #8893, #15898, .T. ) ;
#4608 = CIRCLE ( 'NONE', #4005, 2.000000000000001776 ) ;
#4609 = DIRECTION ( 'NONE',  ( 0.000000000000000000, 0.000000000000000000, 1.000000000000000000 ) ) ;
#4610 = VERTEX_POINT ( 'NONE', #20447 ) ;
#4611 = DIRECTION ( 'NONE',  ( 1.000000000000000000, -0.000000000000000000, 0.000000000000000000 ) ) ;
#4612 = VERTEX_POINT ( 'NONE', #23081 ) ;
#4613 =( GEOMETRIC_REPRESENTATION_CONTEXT ( 3 ) GLOBAL_UNCERTAINTY_ASSIGNED_CONTEXT ( ( #33935 ) ) GLOBAL_UNIT_ASSIGNED_CONTEXT ( ( #21900, #30699, #18724 ) ) REPRESENTATION_CONTEXT ( 'NONE', 'WORKASPACE' ) );
#4614 = FACE_BOUND ( 'NONE', #7088, .T. ) ;
#4615 = VECTOR ( 'NONE', #12014, 1000.000000000000000 ) ;
#4616 = AXIS2_PLACEMENT_3D ( 'NONE', #371, #26262, #34717 ) ;
#4617 = VECTOR ( 'NONE', #35577, 1000.000000000000000 ) ;
#4618 = DIRECTION ( 'NONE',  ( 1.000000000000000000, 0.000000000000000000, 0.000000000000000000 ) ) ;
#4619 = DIRECTION ( 'NONE',  ( 1.000000000000000000, 0.000000000000000000, 0.000000000000000000 ) ) ;
#4620 = DIRECTION ( 'NONE',  ( 0.000000000000000000, 0.000000000000000000, 1.000000000000000000 ) ) ;
#4621 = VERTEX_POINT ( 'NONE', #31868 ) ;
#4622 = DIRECTION ( 'NONE',  ( 0.000000000000000000, 0.000000000000000000, 1.000000000000000000 ) ) ;
#4623 = CIRCLE ( 'NONE', #19584, 2.000000000000001776 ) ;
#4624 = FACE_OUTER_BOUND ( 'NONE', #10553, .T. ) ;
#4625 = CYLINDRICAL_SURFACE ( 'NONE', #5598, 2.000000000000000000 ) ;
#4626 = ADVANCED_FACE ( 'NONE', ( #28524, #28718, #3049 ), #28332, .F. ) ;
#4627 = CARTESIAN_POINT ( 'NONE',  ( 0.000000000000000000, 82.16276890242660613, -31.51554445662266346 ) ) ;
#4628 = CARTESIAN_POINT ( 'NONE',  ( -2.000003374631303732, -86.60254037844400443, -5.000000000000000000 ) ) ;
#4629 = ORIENTED_EDGE ( 'NONE', *, *, #32560, .F. ) ;
#4630 = EDGE_CURVE ( 'NONE', #7478, #3872, #921, .T. ) ;
#4631 = DIRECTION ( 'NONE',  ( 1.000000000000000000, 0.000000000000000000, 0.000000000000000000 ) ) ;
#4632 = AXIS2_PLACEMENT_3D ( 'NONE', #23357, #20349, #28949 ) ;
#4633 = CARTESIAN_POINT ( 'NONE',  ( 0.000000000000000000, 81.28776890242660613, -29.99999999999987566 ) ) ;
#4634 = CARTESIAN_POINT ( 'NONE',  ( -3.000003374631308173, 77.94228634059957983, 12.50000000000000000 ) ) ;
#4635 = VECTOR ( 'NONE', #19266, 1000.000000000000000 ) ;
#4636 = ORIENTED_EDGE ( 'NONE', *, *, #25707, .F. ) ;
#4637 = AXIS2_PLACEMENT_3D ( 'NONE', #34215, #25771, #17126 ) ;
#4638 = ORIENTED_EDGE ( 'NONE', *, *, #12629, .F. ) ;
#4639 = EDGE_CURVE ( 'NONE', #2266, #126, #35061, .T. ) ;
#4640 = DIRECTION ( 'NONE',  ( 0.000000000000000000, 0.000000000000000000, 1.000000000000000000 ) ) ;
#4641 = FACE_OUTER_BOUND ( 'NONE', #30345, .T. ) ;
#4642 = CARTESIAN_POINT ( 'NONE',  ( -73.00000337463100664, -43.30127018922202353, -5.000000000000000000 ) ) ;
#4643 = AXIS2_PLACEMENT_3D ( 'NONE', #25026, #18832, #15822 ) ;
#4644 = ORIENTED_EDGE ( 'NONE', *, *, #31404, .T. ) ;
#4645 = CARTESIAN_POINT ( 'NONE',  ( 21.99999662536862033, -69.28203230275519786, -5.000000000000000000 ) ) ;
#4646 = CARTESIAN_POINT ( 'NONE',  ( 72.28378166042060116, 61.53067111003190348, -4.999999999999997335 ) ) ;
#4647 = DIRECTION ( 'NONE',  ( 1.000000000000000000, 0.000000000000000000, 0.000000000000000000 ) ) ;
#4648 = AXIS2_PLACEMENT_3D ( 'NONE', #18308, #24127, #35406 ) ;
#4649 = CARTESIAN_POINT ( 'NONE',  ( -78.83845375417729429, 72.26717041423300714, 32.50000000000000000 ) ) ;
#4650 = EDGE_CURVE ( 'NONE', #31750, #8057, #22740, .T. ) ;
#4651 = ORIENTED_EDGE ( 'NONE', *, *, #21027, .F. ) ;
#4653 = VERTEX_POINT ( 'NONE', #28881 ) ;
#4652 = EDGE_CURVE ( 'NONE', #12600, #15693, #19484, .T. ) ;
#4654 = CARTESIAN_POINT ( 'NONE',  ( -75.00000337463097821, 43.30127018922197379, -9.999999999999998224 ) ) ;
#4655 = EDGE_CURVE ( 'NONE', #35263, #28959, #33712, .T. ) ;
#4656 = CIRCLE ( 'NONE', #35197, 2.000000000000001776 ) ;
#4657 = DIRECTION ( 'NONE',  ( 1.000000000000000000, 0.000000000000000000, 0.000000000000000000 ) ) ;
#4659 = EDGE_CURVE ( 'NONE', #36154, #31806, #26677, .T. ) ;
#4658 = ORIENTED_EDGE ( 'NONE', *, *, #55, .T. ) ;
#4660 = CARTESIAN_POINT ( 'NONE',  ( -3.514986608498314347, -4.017641317389597511, -4.057689166958359905 ) ) ;
#4661 = VERTEX_POINT ( 'NONE', #3204 ) ;
#4662 = CIRCLE ( 'NONE', #22641, 3.500000000000003109 ) ;
#4663 = CIRCLE ( 'NONE', #33997, 2.000000000000001776 ) ;
#4664 = CARTESIAN_POINT ( 'NONE',  ( -47.00000337463111322, -77.94228634059960825, -9.999999999999998224 ) ) ;
#4665 = CIRCLE ( 'NONE', #12420, 27.00000000000001066 ) ;
#4666 = CIRCLE ( 'NONE', #24411, 20.00000000000001066 ) ;
#4667 = DIRECTION ( 'NONE',  ( 0.000000000000000000, 0.000000000000000000, 1.000000000000000000 ) ) ;
#4668 = ORIENTED_EDGE ( 'NONE', *, *, #17737, .F. ) ;
#4669 = CARTESIAN_POINT ( 'NONE',  ( 54.99999662536844625, -60.62177826491080168, -9.999999999999998224 ) ) ;
#4670 = ORIENTED_EDGE ( 'NONE', *, *, #18379, .T. ) ;
#4671 = SURFACE_STYLE_FILL_AREA ( #13096 ) ;
#4672 = CIRCLE ( 'NONE', #10631, 2.000000000000001776 ) ;
#4673 = CARTESIAN_POINT ( 'NONE',  ( -98.28784258493107018, -106.7731239591678474, 32.55002500000000509 ) ) ;
#4674 = CIRCLE ( 'NONE', #32790, 2.000000000000001776 ) ;
#4675 = CARTESIAN_POINT ( 'NONE',  ( 84.99999662536832545, 25.98076211353319565, -9.999999999999998224 ) ) ;
#4676 = DIRECTION ( 'NONE',  ( 0.000000000000000000, 0.000000000000000000, 1.000000000000000000 ) ) ;
#4677 = EDGE_LOOP ( 'NONE', ( #13548, #3195 ) ) ;
#4678 = CYLINDRICAL_SURFACE ( 'NONE', #16080, 2.000000000000001776 ) ;
#4679 = CARTESIAN_POINT ( 'NONE',  ( -52.39915983220772233, -35.19434990244957362, 12.49999999999999822 ) ) ;
#4680 = AXIS2_PLACEMENT_3D ( 'NONE', #6820, #30245, #10213 ) ;
#4681 = CARTESIAN_POINT ( 'NONE',  ( -3.556264818047238485, -3.720292241887096285, -5.918341802876226687 ) ) ;
#4682 = VERTEX_POINT ( 'NONE', #37 ) ;
#4683 = ADVANCED_FACE ( 'NONE', ( #33992 ), #31453, .F. ) ;
#4684 = VERTEX_POINT ( 'NONE', #2654 ) ;
#4685 = EDGE_LOOP ( 'NONE', ( #12320, #20407, #6996, #21912, #1930 ) ) ;
#4686 = DIRECTION ( 'NONE',  ( -0.000000000000000000, -0.000000000000000000, -1.000000000000000000 ) ) ;
#4687 = EDGE_LOOP ( 'NONE', ( #14212, #31202 ) ) ;
#4688 = CIRCLE ( 'NONE', #25617, 2.000000000000001776 ) ;
#4689 = AXIS2_PLACEMENT_3D ( 'NONE', #7170, #35857, #35658 ) ;
#4690 = CARTESIAN_POINT ( 'NONE',  ( -6.532899837730827386, 8.000494875427320504E-16, -5.132899837730832360 ) ) ;
#4691 = CARTESIAN_POINT ( 'NONE',  ( 84.99999662536832545, 8.660254037844394404, -9.999999999999998224 ) ) ;
#4692 = CIRCLE ( 'NONE', #8271, 2.000000000000001776 ) ;
#4693 = DIRECTION ( 'NONE',  ( 0.000000000000000000, -0.000000000000000000, -1.000000000000000000 ) ) ;
#4694 = CIRCLE ( 'NONE', #28627, 2.000000000000001776 ) ;
#4695 = CARTESIAN_POINT ( 'NONE',  ( -23.00000337463121980, -77.94228634059963667, 17.49999999999999645 ) ) ;
#4696 = LINE ( 'NONE', #24377, #14292 ) ;
#4697 = CARTESIAN_POINT ( 'NONE',  ( -5.826918817341602493E-15, 5.807445019730648639, -4.151004066889659505 ) ) ;
#4698 = DIRECTION ( 'NONE',  ( 0.000000000000000000, 0.000000000000000000, 1.000000000000000000 ) ) ;
#4699 = ORIENTED_EDGE ( 'NONE', *, *, #16412, .T. ) ;
#4700 = VERTEX_POINT ( 'NONE', #19905 ) ;
#4701 = VECTOR ( 'NONE', #5047, 1000.000000000000000 ) ;
#4702 = DIRECTION ( 'NONE',  ( -1.000000000000000000, 0.000000000000000000, 0.000000000000000000 ) ) ;
#4703 = DIRECTION ( 'NONE',  ( 1.000000000000000000, 0.000000000000000000, 0.000000000000000000 ) ) ;
#4704 = EDGE_CURVE ( 'NONE', #22301, #6746, #10512, .T. ) ;
#4705 = DIRECTION ( 'NONE',  ( 1.000000000000000000, 0.000000000000000000, 0.000000000000000000 ) ) ;
#4706 = DIRECTION ( 'NONE',  ( 1.000000000000000000, 0.000000000000000000, 0.000000000000000000 ) ) ;
#4707 = ORIENTED_EDGE ( 'NONE', *, *, #17502, .T. ) ;
#4708 = UNCERTAINTY_MEASURE_WITH_UNIT (LENGTH_MEASURE( 1.000000000000000082E-05 ), #33345, 'distance_accuracy_value', 'NONE');
#4709 = CIRCLE ( 'NONE', #9493, 33.00000000000001421 ) ;
#4710 = CARTESIAN_POINT ( 'NONE',  ( -68.00000000000000000, 0.000000000000000000, -49.86348611802629449 ) ) ;
#4711 = DIRECTION ( 'NONE',  ( 0.000000000000000000, 0.000000000000000000, -1.000000000000000000 ) ) ;
#4712 = DIRECTION ( 'NONE',  ( -0.000000000000000000, -0.000000000000000000, 1.000000000000000000 ) ) ;
#4713 = AXIS2_PLACEMENT_3D ( 'NONE', #12136, #28844, #32011 ) ;
#4714 = EDGE_LOOP ( 'NONE', ( #23125, #19838, #13363, #8521 ) ) ;
#4715 = VECTOR ( 'NONE', #26429, 1000.000000000000000 ) ;
#4716 = CARTESIAN_POINT ( 'NONE',  ( -55.00000337463107059, 60.62177826491078747, -9.999999999999998224 ) ) ;
#4717 = ORIENTED_EDGE ( 'NONE', *, *, #12027, .T. ) ;
#4718 = CIRCLE ( 'NONE', #29233, 2.000000000000001776 ) ;
#4719 = CARTESIAN_POINT ( 'NONE',  ( -55.00000337463109901, -60.62177826491083010, 12.50000000000000000 ) ) ;
#4720 = LINE ( 'NONE', #16331, #36784 ) ;
#4721 = CIRCLE ( 'NONE', #22088, 2.000000000000001776 ) ;
#4722 = CARTESIAN_POINT ( 'NONE',  ( -87.00000337463093558, 8.660254037844389075, 12.50000000000000000 ) ) ;
#4723 = EDGE_LOOP ( 'NONE', ( #4368, #32539 ) ) ;
#4724 = VERTEX_POINT ( 'NONE', #8838 ) ;
#4725 = ADVANCED_FACE ( 'NONE', ( #6038 ), #17461, .T. ) ;
#4726 = ADVANCED_FACE ( 'NONE', ( #20825 ), #32443, .F. ) ;
#4727 = FACE_OUTER_BOUND ( 'NONE', #11369, .T. ) ;
#4728 = ORIENTED_EDGE ( 'NONE', *, *, #12498, .T. ) ;
#4729 = DIRECTION ( 'NONE',  ( -0.5000000000000098810, -0.8660254037844328234, 0.000000000000000000 ) ) ;
#4730 = DIRECTION ( 'NONE',  ( 0.000000000000000000, 0.000000000000000000, 1.000000000000000000 ) ) ;
#4731 = PLANE ( 'NONE',  #5856 ) ;
#4732 = CARTESIAN_POINT ( 'NONE',  ( -58.00000337463104216, 34.64101615137757051, -9.999999999999998224 ) ) ;
#4733 = LINE ( 'NONE', #21964, #32719 ) ;
#4734 = ORIENTED_EDGE ( 'NONE', *, *, #30255, .T. ) ;
#4735 = CARTESIAN_POINT ( 'NONE',  ( -70.00000337463099243, -2.428612866367529932E-14, 17.49999999999999645 ) ) ;
#4736 = PRODUCT_DEFINITION_SHAPE ( 'NONE', 'NONE',  #37131 ) ;
#4737 = CARTESIAN_POINT ( 'NONE',  ( 6.078523336270777024E-16, 5.773502691896261751, -6.000000000000000000 ) ) ;
#4738 = EDGE_CURVE ( 'NONE', #5973, #35680, #6390, .T. ) ;
#4739 = AXIS2_PLACEMENT_3D ( 'NONE', #9550, #23991, #30148 ) ;
#4740 = CARTESIAN_POINT ( 'NONE',  ( 3.000000000000000000, -2.629050547790028157E-15, -2.541999999999999815 ) ) ;
#4741 = EDGE_LOOP ( 'NONE', ( #2665, #32761, #3413, #33240 ) ) ;
#4742 = DIRECTION ( 'NONE',  ( 0.000000000000000000, 0.000000000000000000, 1.000000000000000000 ) ) ;
#4743 = FACE_OUTER_BOUND ( 'NONE', #12767, .T. ) ;
#4744 = VERTEX_POINT ( 'NONE', #9944 ) ;
#4745 = EDGE_LOOP ( 'NONE', ( #29743, #33940, #13619, #32481, #7404 ) ) ;
#4746 = CIRCLE ( 'NONE', #29266, 33.00000000000001421 ) ;
#4747 = DIRECTION ( 'NONE',  ( 0.000000000000000000, 0.000000000000000000, 1.000000000000000000 ) ) ;
#4748 = EDGE_CURVE ( 'NONE', #14472, #33302, #19543, .T. ) ;
#4749 = CARTESIAN_POINT ( 'NONE',  ( 3.000000000000000000, 0.000000000000000000, 0.000000000000000000 ) ) ;
#4750 = PLANE ( 'NONE',  #29789 ) ;
#4751 = ORIENTED_EDGE ( 'NONE', *, *, #29260, .T. ) ;
#4752 = ORIENTED_EDGE ( 'NONE', *, *, #35183, .T. ) ;
#4753 = VERTEX_POINT ( 'NONE', #9587 ) ;
#4754 = CIRCLE ( 'NONE', #28686, 2.000000000000001776 ) ;
#4755 = FACE_OUTER_BOUND ( 'NONE', #26288, .T. ) ;
#4756 = AXIS2_PLACEMENT_3D ( 'NONE', #11001, #31078, #22441 ) ;
#4757 = ORIENTED_EDGE ( 'NONE', *, *, #10532, .T. ) ;
#4758 = AXIS2_PLACEMENT_3D ( 'NONE', #7222, #4227, #35533 ) ;
#4759 = CARTESIAN_POINT ( 'NONE',  ( 4.279621169095998212, -62.97617850287780072, -4.999999999999997335 ) ) ;
#4760 = VERTEX_POINT ( 'NONE', #35081 ) ;
#4761 = ORIENTED_EDGE ( 'NONE', *, *, #25041, .T. ) ;
#4762 = DIRECTION ( 'NONE',  ( -1.000000000000000000, 0.000000000000000000, 0.000000000000000000 ) ) ;
#4763 = AXIS2_PLACEMENT_3D ( 'NONE', #24125, #18689, #7068 ) ;
#4764 = EDGE_CURVE ( 'NONE', #3013, #16096, #12738, .T. ) ;
#4765 = FACE_OUTER_BOUND ( 'NONE', #4997, .T. ) ;
#4766 = ORIENTED_EDGE ( 'NONE', *, *, #10549, .T. ) ;
#4767 = ORIENTED_EDGE ( 'NONE', *, *, #4576, .F. ) ;
#4768 = CARTESIAN_POINT ( 'NONE',  ( 54.99999662536846046, -43.30127018922200222, -9.999999999999998224 ) ) ;
#4769 = AXIS2_PLACEMENT_3D ( 'NONE', #27991, #7760, #16371 ) ;
#4770 = CYLINDRICAL_SURFACE ( 'NONE', #6980, 1.999999999999998224 ) ;
#4771 = CARTESIAN_POINT ( 'NONE',  ( -88.00000337463090716, -1.040834085586084257E-14, -5.000000000000000000 ) ) ;
#4772 = DIRECTION ( 'NONE',  ( -0.000000000000000000, 0.000000000000000000, -1.000000000000000000 ) ) ;
#4773 = EDGE_LOOP ( 'NONE', ( #591, #11084, #19226, #3528 ) ) ;
#4774 = CARTESIAN_POINT ( 'NONE',  ( -72.00000337463100664, 34.64101615137758472, 12.50000000000000000 ) ) ;
#4775 = FACE_BOUND ( 'NONE', #31293, .T. ) ;
#4776 = EDGE_CURVE ( 'NONE', #24912, #12365, #32056, .T. ) ;
#4777 = DIRECTION ( 'NONE',  ( 0.000000000000000000, -0.5000000000000011102, -0.8660254037844379305 ) ) ;
#4778 = DIRECTION ( 'NONE',  ( 0.5000000000000039968, 0.8660254037844363761, 0.000000000000000000 ) ) ;
#4779 = CARTESIAN_POINT ( 'NONE',  ( 66.99999662536839651, -60.62177826491080168, -5.000000000000000000 ) ) ;
#4780 = AXIS2_PLACEMENT_3D ( 'NONE', #8394, #31426, #5565 ) ;
#4781 = DIRECTION ( 'NONE',  ( 0.000000000000000000, 0.000000000000000000, 1.000000000000000000 ) ) ;
#4782 = CYLINDRICAL_SURFACE ( 'NONE', #9536, 2.000000000000001776 ) ;
#4783 = EDGE_CURVE ( 'NONE', #30464, #18023, #13532, .T. ) ;
#4784 = LINE ( 'NONE', #27810, #8597 ) ;
#4785 = ORIENTED_EDGE ( 'NONE', *, *, #6664, .T. ) ;
#4786 = DIRECTION ( 'NONE',  ( 1.000000000000000000, 0.000000000000000000, 0.000000000000000000 ) ) ;
#4787 = DIRECTION ( 'NONE',  ( 0.000000000000000000, 0.000000000000000000, 1.000000000000000000 ) ) ;
#4788 = AXIS2_PLACEMENT_3D ( 'NONE', #9652, #29688, #35707 ) ;
#4789 = DIRECTION ( 'NONE',  ( -0.000000000000000000, -0.000000000000000000, -1.000000000000000000 ) ) ;
#4790 = ORIENTED_EDGE ( 'NONE', *, *, #17334, .F. ) ;
#4791 = EDGE_LOOP ( 'NONE', ( #28617, #35683, #34393, #624 ) ) ;
#4792 = ORIENTED_EDGE ( 'NONE', *, *, #32232, .T. ) ;
#4793 = AXIS2_PLACEMENT_3D ( 'NONE', #4820, #13609, #33108 ) ;
#4794 = CYLINDRICAL_SURFACE ( 'NONE', #26734, 2.000000000000000000 ) ;
#4795 = DIRECTION ( 'NONE',  ( -1.000000000000000000, 0.000000000000000000, 0.000000000000000000 ) ) ;
#4796 = AXIS2_PLACEMENT_3D ( 'NONE', #34273, #28635, #34100 ) ;
#4797 = VERTEX_POINT ( 'NONE', #3591 ) ;
#4798 = DIRECTION ( 'NONE',  ( 0.000000000000000000, 0.000000000000000000, -1.000000000000000000 ) ) ;
#4799 = EDGE_CURVE ( 'NONE', #7714, #25889, #21319, .T. ) ;
#4800 = FACE_OUTER_BOUND ( 'NONE', #19182, .T. ) ;
#4801 = ORIENTED_EDGE ( 'NONE', *, *, #6912, .F. ) ;
#4802 = DIRECTION ( 'NONE',  ( 0.000000000000000000, 0.000000000000000000, 1.000000000000000000 ) ) ;
#4803 = EDGE_LOOP ( 'NONE', ( #24203, #34220, #35381, #10075 ) ) ;
#4804 = PLANE ( 'NONE',  #336 ) ;
#4805 = AXIS2_PLACEMENT_3D ( 'NONE', #22223, #33662, #13788 ) ;
#4806 = EDGE_CURVE ( 'NONE', #20017, #2812, #30292, .T. ) ;
#4807 = CARTESIAN_POINT ( 'NONE',  ( 19.99999662536857770, 86.60254037844397601, -9.999999999999998224 ) ) ;
#4808 = FACE_OUTER_BOUND ( 'NONE', #24142, .T. ) ;
#4809 = EDGE_CURVE ( 'NONE', #23895, #34851, #21919, .T. ) ;
#4810 = DIRECTION ( 'NONE',  ( 1.000000000000000000, 0.000000000000000000, 0.000000000000000000 ) ) ;
#4811 = CIRCLE ( 'NONE', #21554, 2.000000000000001776 ) ;
#4812 = ORIENTED_EDGE ( 'NONE', *, *, #35492, .T. ) ;
#4813 = CARTESIAN_POINT ( 'NONE',  ( -15.00000337463126066, 77.94228634059957983, 17.49999999999999645 ) ) ;
#4814 = AXIS2_PLACEMENT_3D ( 'NONE', #35445, #9362, #9731 ) ;
#4815 = ITEM_DEFINED_TRANSFORMATION ( 'NONE', 'NONE', #9974,  #21385 ) ;
#4816 = CYLINDRICAL_SURFACE ( 'NONE', #6906, 1.999999999999998224 ) ;
#4817 = DIRECTION ( 'NONE',  ( 1.000000000000000000, 0.000000000000000000, 0.000000000000000000 ) ) ;
#4818 = EDGE_LOOP ( 'NONE', ( #7556, #26983, #27021, #34137 ) ) ;
#4819 = LINE ( 'NONE', #21500, #28144 ) ;
#4820 = CARTESIAN_POINT ( 'NONE',  ( -65.00000337463104927, -25.98076211353322051, 12.50000000000000000 ) ) ;
#4821 = EDGE_LOOP ( 'NONE', ( #21628, #3865, #32039, #35325 ) ) ;
#4822 = CARTESIAN_POINT ( 'NONE',  ( -37.00000337463116296, 77.94228634059957983, -9.999999999999998224 ) ) ;
#4823 = VECTOR ( 'NONE', #33504, 1000.000000000000000 ) ;
#4824 = DIRECTION ( 'NONE',  ( -0.000000000000000000, -0.000000000000000000, 1.000000000000000000 ) ) ;
#4825 = CARTESIAN_POINT ( 'NONE',  ( -47.04203867989546950, 43.19957991610416315, 12.49999999999999822 ) ) ;
#4826 = ORIENTED_EDGE ( 'NONE', *, *, #31749, .T. ) ;
#4827 = EDGE_CURVE ( 'NONE', #22247, #15238, #15196, .T. ) ;
#4828 = ORIENTED_EDGE ( 'NONE', *, *, #7003, .F. ) ;
#4829 = VECTOR ( 'NONE', #16479, 1000.000000000000000 ) ;
#4830 = FACE_OUTER_BOUND ( 'NONE', #339, .T. ) ;
#4831 = DIRECTION ( 'NONE',  ( 1.000000000000000000, 0.000000000000000000, 0.000000000000000000 ) ) ;
#4832 = DIRECTION ( 'NONE',  ( 0.000000000000000000, 0.000000000000000000, 1.000000000000000000 ) ) ;
#4833 = ORIENTED_EDGE ( 'NONE', *, *, #36204, .F. ) ;
#4834 = ORIENTED_EDGE ( 'NONE', *, *, #26069, .T. ) ;
#4835 = CIRCLE ( 'NONE', #17987, 2.000000000000000000 ) ;
#4836 = DIRECTION ( 'NONE',  ( 0.000000000000000000, 0.000000000000000000, -1.000000000000000000 ) ) ;
#4837 = CARTESIAN_POINT ( 'NONE',  ( 0.000000000000000000, 0.000000000000000000, 17.49999999999999645 ) ) ;
#4838 = LINE ( 'NONE', #25091, #4635 ) ;
#4839 = AXIS2_PLACEMENT_3D ( 'NONE', #1220, #12639, #35912 ) ;
#4840 = CARTESIAN_POINT ( 'NONE',  ( -106.4311476201816618, 54.27652618157941333, 32.50000000000000000 ) ) ;
#4841 = VERTEX_POINT ( 'NONE', #4328 ) ;
#4842 = ORIENTED_EDGE ( 'NONE', *, *, #33937, .T. ) ;
#4843 = DIRECTION ( 'NONE',  ( 0.000000000000000000, 0.000000000000000000, -1.000000000000000000 ) ) ;
#4844 = EDGE_CURVE ( 'NONE', #25741, #19087, #35088, .T. ) ;
#4845 = CARTESIAN_POINT ( 'NONE',  ( -75.00000337463097821, 25.98076211353318854, 17.49999999999999645 ) ) ;
#4846 = EDGE_LOOP ( 'NONE', ( #3809, #15910, #17879, #17988 ) ) ;
#4847 = ADVANCED_FACE ( 'NONE', ( #18592 ), #21191, .T. ) ;
#4848 = FACE_BOUND ( 'NONE', #18275, .T. ) ;
#4849 = ORIENTED_EDGE ( 'NONE', *, *, #9612, .F. ) ;
#4850 = DIRECTION ( 'NONE',  ( 0.000000000000000000, 0.000000000000000000, 1.000000000000000000 ) ) ;
#4851 = ADVANCED_FACE ( 'NONE', ( #12368, #6946 ), #23837, .T. ) ;
#4852 = CARTESIAN_POINT ( 'NONE',  ( 59.99999662536842493, -51.96152422706639840, 17.49999999999999645 ) ) ;
#4853 = ADVANCED_FACE ( 'NONE', ( #1499 ), #6756, .F. ) ;
#4854 = FACE_OUTER_BOUND ( 'NONE', #17749, .T. ) ;
#4855 = VERTEX_POINT ( 'NONE', #3945 ) ;
#4856 = EDGE_CURVE ( 'NONE', #35263, #10511, #22100, .T. ) ;
#4857 = DIRECTION ( 'NONE',  ( 0.000000000000000000, 0.000000000000000000, 1.000000000000000000 ) ) ;
#4858 = DIRECTION ( 'NONE',  ( 0.000000000000000000, 0.000000000000000000, -1.000000000000000000 ) ) ;
#4859 = CARTESIAN_POINT ( 'NONE',  ( 29.99999662536857770, -69.28203230275519786, 17.49999999999999645 ) ) ;
#4860 = AXIS2_PLACEMENT_3D ( 'NONE', #14407, #26015, #135 ) ;
#4861 = ORIENTED_EDGE ( 'NONE', *, *, #31721, .F. ) ;
#4862 = CARTESIAN_POINT ( 'NONE',  ( -80.00000337463094979, -17.32050807568882078, 12.50000000000000000 ) ) ;
#4863 = DIRECTION ( 'NONE',  ( 0.000000000000000000, 0.000000000000000000, 1.000000000000000000 ) ) ;
#4864 = DIRECTION ( 'NONE',  ( 0.000000000000000000, 0.000000000000000000, 1.000000000000000000 ) ) ;
#4865 = ADVANCED_FACE ( 'NONE', ( #23461 ), #36191, .F. ) ;
#4866 = ORIENTED_EDGE ( 'NONE', *, *, #17737, .T. ) ;
#4867 = EDGE_CURVE ( 'NONE', #21984, #22983, #20122, .T. ) ;
#4868 = ORIENTED_EDGE ( 'NONE', *, *, #4341, .F. ) ;
#4869 = VERTEX_POINT ( 'NONE', #35840 ) ;
#4870 = EDGE_CURVE ( 'NONE', #29683, #21341, #8163, .T. ) ;
#4871 = EDGE_CURVE ( 'NONE', #36051, #17344, #351, .T. ) ;
#4872 = CARTESIAN_POINT ( 'NONE',  ( -50.00000337463110611, -69.28203230275519786, -9.999999999999998224 ) ) ;
#4874 = EDGE_CURVE ( 'NONE', #26842, #35523, #9323, .T. ) ;
#4873 = ORIENTED_EDGE ( 'NONE', *, *, #22376, .T. ) ;
#4875 = CARTESIAN_POINT ( 'NONE',  ( 64.99999662536839651, -43.30127018922199511, -5.000000000000000000 ) ) ;
#4876 = DIRECTION ( 'NONE',  ( 1.000000000000000000, 0.000000000000000000, 0.000000000000000000 ) ) ;
#4877 = CARTESIAN_POINT ( 'NONE',  ( -20.00000337463124112, 69.28203230275516944, -9.999999999999998224 ) ) ;
#4878 = CYLINDRICAL_SURFACE ( 'NONE', #28974, 33.00000000000001421 ) ;
#4879 = DIRECTION ( 'NONE',  ( -0.000000000000000000, -0.000000000000000000, 1.000000000000000000 ) ) ;
#4880 = DIRECTION ( 'NONE',  ( 0.000000000000000000, 0.000000000000000000, 1.000000000000000000 ) ) ;
#4881 = CIRCLE ( 'NONE', #1275, 95.00000000000000000 ) ;
#4882 = DIRECTION ( 'NONE',  ( 1.000000000000000000, 0.000000000000000000, 0.000000000000000000 ) ) ;
#4883 = DIRECTION ( 'NONE',  ( 0.000000000000000000, 0.000000000000000000, 1.000000000000000000 ) ) ;
#4884 = ORIENTED_EDGE ( 'NONE', *, *, #26797, .T. ) ;
#4885 = ORIENTED_EDGE ( 'NONE', *, *, #27225, .T. ) ;
#4886 = DIRECTION ( 'NONE',  ( 0.000000000000000000, 0.000000000000000000, 1.000000000000000000 ) ) ;
#4887 = DIRECTION ( 'NONE',  ( 1.000000000000000000, 0.000000000000000000, 0.000000000000000000 ) ) ;
#4888 = DIRECTION ( 'NONE',  ( 0.000000000000000000, 0.000000000000000000, 1.000000000000000000 ) ) ;
#4889 = ORIENTED_EDGE ( 'NONE', *, *, #12721, .F. ) ;
#4890 = CARTESIAN_POINT ( 'NONE',  ( 69.99999662536839651, 17.32050807568879236, -9.999999999999998224 ) ) ;
#4891 = FACE_OUTER_BOUND ( 'NONE', #17722, .T. ) ;
#4892 = VERTEX_POINT ( 'NONE', #24950 ) ;
#4893 = APPLICATION_CONTEXT ( 'automotive_design' ) ;
#4894 = CARTESIAN_POINT ( 'NONE',  ( -80.00000337463096400, -34.64101615137762025, -9.999999999999998224 ) ) ;
#4895 = ORIENTED_EDGE ( 'NONE', *, *, #20162, .T. ) ;
#4896 = FILL_AREA_STYLE_COLOUR ( '', #3427 ) ;
#4897 = DIRECTION ( 'NONE',  ( -1.000000000000000000, 0.000000000000000000, 0.000000000000000000 ) ) ;
#4898 = DIRECTION ( 'NONE',  ( 0.000000000000000000, 0.000000000000000000, 1.000000000000000000 ) ) ;
#4899 = AXIS2_PLACEMENT_3D ( 'NONE', #32498, #12795, #10208 ) ;
#4900 = VERTEX_POINT ( 'NONE', #13486 ) ;
#4901 = VERTEX_POINT ( 'NONE', #24592 ) ;
#4902 = CIRCLE ( 'NONE', #9085, 1.999999999999998224 ) ;
#4903 = ORIENTED_EDGE ( 'NONE', *, *, #1074, .T. ) ;
#4904 = CARTESIAN_POINT ( 'NONE',  ( 0.000000000000000000, 0.000000000000000000, 12.49999999999999822 ) ) ;
#4905 = EDGE_CURVE ( 'NONE', #8144, #31157, #7548, .T. ) ;
#4906 = CARTESIAN_POINT ( 'NONE',  ( 45.00000000000000711, 0.000000000000000000, -10.00000000000000000 ) ) ;
#4907 = DIRECTION ( 'NONE',  ( 1.000000000000000000, 0.000000000000000000, 0.000000000000000000 ) ) ;
#4908 = DIRECTION ( 'NONE',  ( 1.000000000000000000, 0.000000000000000000, 0.000000000000000000 ) ) ;
#4909 = FACE_OUTER_BOUND ( 'NONE', #20654, .T. ) ;
#4910 = VERTEX_POINT ( 'NONE', #27576 ) ;
#4911 = CYLINDRICAL_SURFACE ( 'NONE', #23117, 2.000000000000001776 ) ;
#4912 = CARTESIAN_POINT ( 'NONE',  ( 6.249999999999998224, 0.000000000000000000, 0.000000000000000000 ) ) ;
#4913 = FILL_AREA_STYLE ('',( #4541 ) ) ;
#4914 = ORIENTED_EDGE ( 'NONE', *, *, #31721, .T. ) ;
#4915 = DIRECTION ( 'NONE',  ( 1.000000000000000000, 0.000000000000000000, 0.000000000000000000 ) ) ;
#4916 = CARTESIAN_POINT ( 'NONE',  ( 66.00000000000000000, 0.000000000000000000, 0.000000000000000000 ) ) ;
#4917 = EDGE_LOOP ( 'NONE', ( #28268, #7454, #871, #1290, #348, #6131 ) ) ;
#4918 = ORIENTED_EDGE ( 'NONE', *, *, #27403, .F. ) ;
#4919 = DIRECTION ( 'NONE',  ( 0.000000000000000000, 0.000000000000000000, 1.000000000000000000 ) ) ;
#4920 = CARTESIAN_POINT ( 'NONE',  ( 0.6806757771967111292, -5.380514348700923932, -3.838711833385402006 ) ) ;
#4921 = DIRECTION ( 'NONE',  ( 1.000000000000000000, 0.000000000000000000, 0.000000000000000000 ) ) ;
#4922 = ORIENTED_EDGE ( 'NONE', *, *, #23505, .T. ) ;
#4923 = EDGE_LOOP ( 'NONE', ( #26480, #25783 ) ) ;
#4924 = EDGE_CURVE ( 'NONE', #15155, #13152, #13308, .T. ) ;
#4925 = CARTESIAN_POINT ( 'NONE',  ( -33.99999999999945288, 58.88972745734214698, -4.999999999999997335 ) ) ;
#4926 = ORIENTED_EDGE ( 'NONE', *, *, #26252, .T. ) ;
#4927 = FACE_OUTER_BOUND ( 'NONE', #30989, .T. ) ;
#4928 = ORIENTED_EDGE ( 'NONE', *, *, #6135, .F. ) ;
#4929 = EDGE_LOOP ( 'NONE', ( #15844, #32999 ) ) ;
#4930 = DIRECTION ( 'NONE',  ( 0.000000000000000000, 0.000000000000000000, 1.000000000000000000 ) ) ;
#4931 = FACE_BOUND ( 'NONE', #5382, .T. ) ;
#4932 = ORIENTED_EDGE ( 'NONE', *, *, #34337, .T. ) ;
#4933 = ORIENTED_EDGE ( 'NONE', *, *, #18131, .F. ) ;
#4934 = DIRECTION ( 'NONE',  ( 0.000000000000000000, -0.8660254037844419273, 0.4999999999999945044 ) ) ;
#4935 = CARTESIAN_POINT ( 'NONE',  ( -107.2724133595221190, -47.49999999999924682, 27.50000000000000000 ) ) ;
#4936 = CARTESIAN_POINT ( 'NONE',  ( -68.00000337463099243, 17.32050807568877460, -9.999999999999998224 ) ) ;
#4937 = DIRECTION ( 'NONE',  ( 0.000000000000000000, 0.000000000000000000, 1.000000000000000000 ) ) ;
#4938 = ORIENTED_EDGE ( 'NONE', *, *, #8184, .F. ) ;
#4939 = DIRECTION ( 'NONE',  ( 0.000000000000000000, 0.000000000000000000, 1.000000000000000000 ) ) ;
#4940 = VECTOR ( 'NONE', #26607, 1000.000000000000000 ) ;
#4941 = EDGE_CURVE ( 'NONE', #23803, #22301, #21747, .T. ) ;
#4942 = FACE_BOUND ( 'NONE', #7434, .T. ) ;
#4943 = CARTESIAN_POINT ( 'NONE',  ( -47.63139720814380951, 27.50000000000055422, -10.00000000000000178 ) ) ;
#4944 = DIRECTION ( 'NONE',  ( 0.000000000000000000, 0.000000000000000000, 1.000000000000000000 ) ) ;
#4945 = CYLINDRICAL_SURFACE ( 'NONE', #7538, 2.000000000000001776 ) ;
#4946 = DIRECTION ( 'NONE',  ( -0.000000000000000000, -0.000000000000000000, 1.000000000000000000 ) ) ;
#4947 = DIRECTION ( 'NONE',  ( 0.000000000000000000, 0.000000000000000000, 1.000000000000000000 ) ) ;
#4948 = DIRECTION ( 'NONE',  ( -0.5000000000000051070, 0.000000000000000000, 0.8660254037844355990 ) ) ;
#4949 = ORIENTED_EDGE ( 'NONE', *, *, #9627, .T. ) ;
#4950 = DIRECTION ( 'NONE',  ( 0.000000000000000000, 0.000000000000000000, -1.000000000000000000 ) ) ;
#4951 = LINE ( 'NONE', #10776, #27909 ) ;
#4952 = FACE_OUTER_BOUND ( 'NONE', #15032, .T. ) ;
#4953 = VERTEX_POINT ( 'NONE', #10697 ) ;
#4954 = VECTOR ( 'NONE', #29654, 1000.000000000000000 ) ;
#4955 = ORIENTED_EDGE ( 'NONE', *, *, #27259, .T. ) ;
#4956 = ORIENTED_EDGE ( 'NONE', *, *, #10827, .F. ) ;
#4957 = EDGE_CURVE ( 'NONE', #23321, #7276, #8751, .T. ) ;
#4958 = DIRECTION ( 'NONE',  ( -1.000000000000000000, 0.000000000000000000, 0.000000000000000000 ) ) ;
#4959 = FACE_OUTER_BOUND ( 'NONE', #23586, .T. ) ;
#4960 = ORIENTED_EDGE ( 'NONE', *, *, #33626, .T. ) ;
#4961 = EDGE_CURVE ( 'NONE', #15953, #16595, #4557, .T. ) ;
#4962 = DIRECTION ( 'NONE',  ( 1.000000000000000000, 0.000000000000000000, 0.000000000000000000 ) ) ;
#4963 = AXIS2_PLACEMENT_3D ( 'NONE', #16473, #27905, #2785 ) ;
#4964 = CARTESIAN_POINT ( 'NONE',  ( 0.000000000000000000, 89.94802294027088863, 27.49999999999999645 ) ) ;
#4965 = ORIENTED_EDGE ( 'NONE', *, *, #28529, .F. ) ;
#4966 = AXIS2_PLACEMENT_3D ( 'NONE', #22381, #7401, #10778 ) ;
#4967 = CARTESIAN_POINT ( 'NONE',  ( 1.999996625368665182, 69.28203230275516944, -9.999999999999998224 ) ) ;
#4968 = ADVANCED_BREP_SHAPE_REPRESENTATION ( '', ( #19278, #21385 ), #2159 ) ;
#4969 = EDGE_CURVE ( 'NONE', #15313, #15633, #30180, .T. ) ;
#4970 = ORIENTED_EDGE ( 'NONE', *, *, #4905, .F. ) ;
#4971 = DIRECTION ( 'NONE',  ( 1.000000000000000000, 0.000000000000000000, 0.000000000000000000 ) ) ;
#4972 = EDGE_CURVE ( 'NONE', #4038, #32213, #33891, .T. ) ;
#4973 = CARTESIAN_POINT ( 'NONE',  ( -45.00000337463112743, -60.62177826491080168, -9.999999999999998224 ) ) ;
#4974 = CARTESIAN_POINT ( 'NONE',  ( 0.4318028594007650156, -5.811705888749012949, -4.266911319714234985 ) ) ;
#4975 = ORIENTED_EDGE ( 'NONE', *, *, #12138, .T. ) ;
#4976 = LINE ( 'NONE', #37044, #34468 ) ;
#4977 = CIRCLE ( 'NONE', #27125, 2.000000000000000000 ) ;
#4978 = CONTEXT_DEPENDENT_SHAPE_REPRESENTATION ( #15673, #2017 ) ;
#4979 = FACE_OUTER_BOUND ( 'NONE', #11173, .T. ) ;
#4980 = DIRECTION ( 'NONE',  ( 0.000000000000000000, 0.000000000000000000, -1.000000000000000000 ) ) ;
#4981 = CIRCLE ( 'NONE', #6149, 2.000000000000001776 ) ;
#4982 = VERTEX_POINT ( 'NONE', #18760 ) ;
#4983 = LINE ( 'NONE', #35571, #25167 ) ;
#4984 = DIRECTION ( 'NONE',  ( 0.000000000000000000, 0.000000000000000000, 1.000000000000000000 ) ) ;
#4985 = ORIENTED_EDGE ( 'NONE', *, *, #5511, .T. ) ;
#4986 = LINE ( 'NONE', #2723, #15454 ) ;
#4987 = CARTESIAN_POINT ( 'NONE',  ( -93.36492675454779544, -17.14523346298311779, -4.999999999999997335 ) ) ;
#4988 = CARTESIAN_POINT ( 'NONE',  ( 0.000000000000000000, 0.000000000000000000, -5.000000000000000000 ) ) ;
#4989 = EDGE_CURVE ( 'NONE', #13923, #24391, #22503, .T. ) ;
#4990 = ORIENTED_EDGE ( 'NONE', *, *, #16986, .F. ) ;
#4991 = AXIS2_PLACEMENT_3D ( 'NONE', #20472, #28555, #8677 ) ;
#4992 = ORIENTED_EDGE ( 'NONE', *, *, #4799, .F. ) ;
#4993 = CARTESIAN_POINT ( 'NONE',  ( -73.00000337463097821, 25.98076211353318854, -9.999999999999998224 ) ) ;
#4994 = DIRECTION ( 'NONE',  ( 1.000000000000000000, 0.000000000000000000, 0.000000000000000000 ) ) ;
#4995 = EDGE_CURVE ( 'NONE', #36127, #792, #26704, .T. ) ;
#4996 = DIRECTION ( 'NONE',  ( -0.000000000000000000, -0.000000000000000000, -1.000000000000000000 ) ) ;
#4997 = EDGE_LOOP ( 'NONE', ( #31009, #30211, #12672, #1591 ) ) ;
#4998 = ORIENTED_EDGE ( 'NONE', *, *, #3172, .T. ) ;
#4999 = EDGE_CURVE ( 'NONE', #18775, #4152, #32754, .T. ) ;
#5000 = DIRECTION ( 'NONE',  ( 1.000000000000000000, 0.000000000000000000, 0.000000000000000000 ) ) ;
#5001 = CARTESIAN_POINT ( 'NONE',  ( -0.9154378789997292820, 5.244974386029388036, -1.156968425231163167 ) ) ;
#5002 = FACE_OUTER_BOUND ( 'NONE', #35247, .T. ) ;
#5003 = CIRCLE ( 'NONE', #3201, 27.00000000000001066 ) ;
#5004 = CARTESIAN_POINT ( 'NONE',  ( 81.99999662536832545, -34.64101615137759183, 17.49999999999999645 ) ) ;
#5005 = EDGE_LOOP ( 'NONE', ( #11292, #20253 ) ) ;
#5006 = ORIENTED_EDGE ( 'NONE', *, *, #16403, .T. ) ;
#5007 = CIRCLE ( 'NONE', #3790, 2.000000000000001776 ) ;
#5008 = DIRECTION ( 'NONE',  ( 3.491481338843135327E-15, 1.000000000000000000, 0.000000000000000000 ) ) ;
#5009 = DIRECTION ( 'NONE',  ( 1.000000000000000000, 0.000000000000000000, 0.000000000000000000 ) ) ;
#5010 = ORIENTED_EDGE ( 'NONE', *, *, #241, .T. ) ;
#5011 = DIRECTION ( 'NONE',  ( 0.000000000000000000, -0.000000000000000000, -1.000000000000000000 ) ) ;
#5012 = EDGE_LOOP ( 'NONE', ( #14358, #15048, #21632, #33214 ) ) ;
#5013 = CARTESIAN_POINT ( 'NONE',  ( -28.00000337463118427, 69.28203230275516944, 12.50000000000000000 ) ) ;
#5014 = CIRCLE ( 'NONE', #22382, 3.499999999999989342 ) ;
#5015 = EDGE_CURVE ( 'NONE', #4869, #17775, #27119, .T. ) ;
#5016 = DIRECTION ( 'NONE',  ( 0.000000000000000000, 0.000000000000000000, 1.000000000000000000 ) ) ;
#5017 = CIRCLE ( 'NONE', #25975, 3.000000000000002665 ) ;
#5018 = VERTEX_POINT ( 'NONE', #1434 ) ;
#5019 = AXIS2_PLACEMENT_3D ( 'NONE', #11531, #22985, #22815 ) ;
#5020 = FACE_OUTER_BOUND ( 'NONE', #23353, .T. ) ;
#5021 = CARTESIAN_POINT ( 'NONE',  ( 77.99999662536832545, -34.64101615137759183, -9.999999999999998224 ) ) ;
#5022 = CARTESIAN_POINT ( 'NONE',  ( -94.40806000769299544, 12.15049814296761888, 32.50002500000000083 ) ) ;
#5023 = VERTEX_POINT ( 'NONE', #27306 ) ;
#5024 = CARTESIAN_POINT ( 'NONE',  ( 57.99999662536844625, 34.64101615137759893, -9.999999999999998224 ) ) ;
#5025 = CARTESIAN_POINT ( 'NONE',  ( -70.00000337463102085, -34.64101615137762025, -9.999999999999998224 ) ) ;
#5026 = CARTESIAN_POINT ( 'NONE',  ( -110.2237710830522559, 101.7384897088162745, 32.50000000000000000 ) ) ;
#5027 = ORIENTED_EDGE ( 'NONE', *, *, #21083, .T. ) ;
#5028 = CIRCLE ( 'NONE', #28360, 2.000000000000001776 ) ;
#5029 = EDGE_CURVE ( 'NONE', #13276, #29025, #5168, .T. ) ;
#5030 = ORIENTED_EDGE ( 'NONE', *, *, #28678, .F. ) ;
#5031 = FACE_OUTER_BOUND ( 'NONE', #9432, .T. ) ;
#5032 = EDGE_CURVE ( 'NONE', #17931, #32624, #1628, .T. ) ;
#5033 = ORIENTED_EDGE ( 'NONE', *, *, #12828, .T. ) ;
#5034 = DIRECTION ( 'NONE',  ( -0.8660254037844379305, 0.5000000000000012212, 0.000000000000000000 ) ) ;
#5035 = CARTESIAN_POINT ( 'NONE',  ( 36.99999662536853862, 77.94228634059959404, -9.999999999999998224 ) ) ;
#5036 = CIRCLE ( 'NONE', #8617, 2.000000000000001776 ) ;
#5037 = ADVANCED_FACE ( 'NONE', ( #23771 ), #6523, .F. ) ;
#5038 = DIRECTION ( 'NONE',  ( 0.5000000000000038858, 0.8660254037844362651, 0.000000000000000000 ) ) ;
#5039 = AXIS2_PLACEMENT_3D ( 'NONE', #23447, #1130, #3577 ) ;
#5040 = CARTESIAN_POINT ( 'NONE',  ( 7.999996625368656744, -69.28203230275519786, -9.999999999999998224 ) ) ;
#5041 = EDGE_CURVE ( 'NONE', #16004, #34714, #15926, .T. ) ;
#5042 = CARTESIAN_POINT ( 'NONE',  ( 100.6561618467704022, -64.69993787454495759, 32.50000000000000711 ) ) ;
#5043 = CARTESIAN_POINT ( 'NONE',  ( -81.11569332658579867, -72.50431249219097651, 32.50000000000000000 ) ) ;
#5044 = EDGE_CURVE ( 'NONE', #26423, #13225, #29071, .T. ) ;
#5045 = DIRECTION ( 'NONE',  ( 0.7071067811865489050, 0.7071067811865461294, -0.000000000000000000 ) ) ;
#5046 = EDGE_CURVE ( 'NONE', #13221, #11018, #18325, .T. ) ;
#5047 = DIRECTION ( 'NONE',  ( 0.000000000000000000, 0.000000000000000000, 1.000000000000000000 ) ) ;
#5048 = ORIENTED_EDGE ( 'NONE', *, *, #31424, .T. ) ;
#5049 = ORIENTED_EDGE ( 'NONE', *, *, #26843, .T. ) ;
#5050 = CARTESIAN_POINT ( 'NONE',  ( -65.00000337463102085, 43.30127018922198801, -5.000000000000000000 ) ) ;
#5051 = CARTESIAN_POINT ( 'NONE',  ( -92.00000337463090716, -1.016341149603137227E-14, -9.999999999999998224 ) ) ;
#5052 = CARTESIAN_POINT ( 'NONE',  ( -31.02796211690907668, 59.29837256189569672, -4.999999999999997335 ) ) ;
#5053 = FACE_OUTER_BOUND ( 'NONE', #15014, .T. ) ;
#5054 = ORIENTED_EDGE ( 'NONE', *, *, #36343, .F. ) ;
#5055 = PRODUCT_DEFINITION_CONTEXT ( 'detailed design', #3678, 'design' ) ;
#5056 = EDGE_CURVE ( 'NONE', #36279, #12950, #6952, .T. ) ;
#5057 = EDGE_CURVE ( 'NONE', #29611, #716, #26145, .T. ) ;
#5058 = CIRCLE ( 'NONE', #21807, 2.000000000000001776 ) ;
#5059 = EDGE_CURVE ( 'NONE', #13060, #10748, #18129, .T. ) ;
#5060 = DIRECTION ( 'NONE',  ( -0.000000000000000000, -0.000000000000000000, 1.000000000000000000 ) ) ;
#5061 = ORIENTED_EDGE ( 'NONE', *, *, #9337, .T. ) ;
#5062 = ORIENTED_EDGE ( 'NONE', *, *, #11553, .F. ) ;
#5063 = CARTESIAN_POINT ( 'NONE',  ( -56.67878100130369035, 27.78182860042797131, -4.999999999999997335 ) ) ;
#5064 = ORIENTED_EDGE ( 'NONE', *, *, #12536, .T. ) ;
#5065 = SHAPE_REPRESENTATION_RELATIONSHIP ( 'NONE' , 'NONE' ,  #33474, #17045 ) ;
#5066 = CARTESIAN_POINT ( 'NONE',  ( -41.00000000000000000, 103.4105893997321886, -19.99999999999999645 ) ) ;
#5067 = AXIS2_PLACEMENT_3D ( 'NONE', #14599, #20417, #344 ) ;
#5068 = PLANE ( 'NONE',  #12202 ) ;
#5069 = CIRCLE ( 'NONE', #30214, 33.00000000000001421 ) ;
#5070 = DIRECTION ( 'NONE',  ( 0.000000000000000000, 0.000000000000000000, -1.000000000000000000 ) ) ;
#5071 = VERTEX_POINT ( 'NONE', #24521 ) ;
#5072 = VERTEX_POINT ( 'NONE', #18524 ) ;
#5073 = ADVANCED_FACE ( 'NONE', ( #26564 ), #4444, .F. ) ;
#5074 = ORIENTED_EDGE ( 'NONE', *, *, #29724, .F. ) ;
#5076 = PLANE ( 'NONE',  #20773 ) ;
#5075 = CIRCLE ( 'NONE', #25446, 2.000000000000001776 ) ;
#5077 = DIRECTION ( 'NONE',  ( -1.000000000000000000, 0.000000000000000000, 0.000000000000000000 ) ) ;
#5078 = EDGE_CURVE ( 'NONE', #15625, #19893, #26735, .T. ) ;
#5079 = AXIS2_PLACEMENT_3D ( 'NONE', #358, #17266, #17434 ) ;
#5080 = CARTESIAN_POINT ( 'NONE',  ( -47.63139720814380951, 27.50000000000055422, -5.000000000000000000 ) ) ;
#5081 = CARTESIAN_POINT ( 'NONE',  ( 56.99999662536846046, -43.30127018922200222, 12.50000000000000000 ) ) ;
#5082 = DIRECTION ( 'NONE',  ( -1.000000000000000000, 0.000000000000000000, 0.000000000000000000 ) ) ;
#5083 = ORIENTED_EDGE ( 'NONE', *, *, #29965, .T. ) ;
#5084 = CARTESIAN_POINT ( 'NONE',  ( -70.00000337463099243, 34.64101615137758472, -5.000000000000000000 ) ) ;
#5085 = VECTOR ( 'NONE', #17620, 1000.000000000000000 ) ;
#5086 = CARTESIAN_POINT ( 'NONE',  ( 25.00000000000000000, 3.061616997868383043E-15, 15.00000000000000000 ) ) ;
#5087 = CYLINDRICAL_SURFACE ( 'NONE', #3215, 2.000000000000000000 ) ;
#5088 = ORIENTED_EDGE ( 'NONE', *, *, #18488, .T. ) ;
#5089 = CYLINDRICAL_SURFACE ( 'NONE', #25068, 95.00000000000000000 ) ;
#5090 = ADVANCED_FACE ( 'NONE', ( #32190 ), #3875, .F. ) ;
#5091 = CARTESIAN_POINT ( 'NONE',  ( -111.8061974404900241, -19.22934205794863516, 32.50000000000000000 ) ) ;
#5092 = AXIS2_PLACEMENT_3D ( 'NONE', #688, #12095, #17554 ) ;
#5093 = VERTEX_POINT ( 'NONE', #23964 ) ;
#5094 = AXIS2_PLACEMENT_3D ( 'NONE', #13648, #7658, #33141 ) ;
#5095 = VERTEX_POINT ( 'NONE', #35414 ) ;
#5096 = DIRECTION ( 'NONE',  ( -1.000000000000000000, 0.000000000000000000, 0.000000000000000000 ) ) ;
#5097 = CARTESIAN_POINT ( 'NONE',  ( 81.99999662536832545, -34.64101615137759183, 12.50000000000000000 ) ) ;
#5098 = CARTESIAN_POINT ( 'NONE',  ( 3.401922400366974131, -3.809401878282419940, -3.971474537231029611 ) ) ;
#5099 = APPLICATION_CONTEXT ( 'automotive_design' ) ;
#5100 = CARTESIAN_POINT ( 'NONE',  ( -102.3447678185619765, -32.57924816083560415, 32.50000000000000711 ) ) ;
#5101 = VERTEX_POINT ( 'NONE', #18316 ) ;
#5102 = ORIENTED_EDGE ( 'NONE', *, *, #2186, .F. ) ;
#5103 = ADVANCED_FACE ( 'NONE', ( #29745 ), #4081, .F. ) ;
#5104 = EDGE_CURVE ( 'NONE', #21168, #14334, #19571, .T. ) ;
#5105 = CARTESIAN_POINT ( 'NONE',  ( 1.999996625368665182, 69.28203230275516944, -9.999999999999998224 ) ) ;
#5106 = ADVANCED_FACE ( 'NONE', ( #35519 ), #7207, .F. ) ;
#5107 = CIRCLE ( 'NONE', #26048, 3.000000000000002665 ) ;
#5108 = ORIENTED_EDGE ( 'NONE', *, *, #5986, .F. ) ;
#5109 = EDGE_CURVE ( 'NONE', #2284, #902, #29721, .T. ) ;
#5110 = CARTESIAN_POINT ( 'NONE',  ( -28.00000337463118427, 69.28203230275516944, -9.999999999999998224 ) ) ;
#5111 = ORIENTED_EDGE ( 'NONE', *, *, #31864, .T. ) ;
#5112 = CIRCLE ( 'NONE', #31435, 3.000000000000000888 ) ;
#5113 = VERTEX_POINT ( 'NONE', #9811 ) ;
#5114 = AXIS2_PLACEMENT_3D ( 'NONE', #34847, #8975, #12309 ) ;
#5115 = DIRECTION ( 'NONE',  ( 0.000000000000000000, 0.000000000000000000, 1.000000000000000000 ) ) ;
#5116 = LINE ( 'NONE', #19746, #23839 ) ;
#5117 = VERTEX_POINT ( 'NONE', #24456 ) ;
#5118 = EDGE_LOOP ( 'NONE', ( #7955, #6356, #14327, #8441, #11510 ) ) ;
#5119 = DIRECTION ( 'NONE',  ( -1.000000000000000000, 1.224646799147353700E-16, 0.000000000000000000 ) ) ;
#5120 = AXIS2_PLACEMENT_3D ( 'NONE', #23375, #4043, #32524 ) ;
#5121 = CARTESIAN_POINT ( 'NONE',  ( 98.28784258493033121, 106.7731239591685437, 32.55002500000000509 ) ) ;
#5122 = B_SPLINE_CURVE_WITH_KNOTS ( 'NONE', 3,
 ( #15384, #20821, #9382, #21011, #15192, #754, #23456, #30004, #580, #15020 ),
 .UNSPECIFIED., .F., .F.,
 ( 4, 2, 2, 2, 4 ),
 ( 0.01815567983891738443, 0.01899359644517026671, 0.01983151305142314552, 0.02066942965767602780, 0.02150734626392890661 ),
 .UNSPECIFIED. ) ;
#5123 = AXIS2_PLACEMENT_3D ( 'NONE', #19064, #30660, #7977 ) ;
#5124 = DIRECTION ( 'NONE',  ( 0.000000000000000000, 0.000000000000000000, 1.000000000000000000 ) ) ;
#5125 = AXIS2_PLACEMENT_3D ( 'NONE', #20620, #6895, #26966 ) ;
#5126 = CARTESIAN_POINT ( 'NONE',  ( -13.00000337463125710, -77.94228634059960825, -9.999999999999998224 ) ) ;
#5127 = VERTEX_POINT ( 'NONE', #9645 ) ;
#5128 = CARTESIAN_POINT ( 'NONE',  ( -70.00000337463099243, 17.32050807568877460, 17.49999999999999645 ) ) ;
#5129 = FACE_BOUND ( 'NONE', #25098, .T. ) ;
#5130 = LINE ( 'NONE', #28001, #33372 ) ;
#5131 = DIRECTION ( 'NONE',  ( 1.000000000000000000, 0.000000000000000000, 0.000000000000000000 ) ) ;
#5132 = DIRECTION ( 'NONE',  ( 1.000000000000000000, 0.000000000000000000, 0.000000000000000000 ) ) ;
#5133 = EDGE_CURVE ( 'NONE', #30504, #8840, #25537, .T. ) ;
#5134 = CARTESIAN_POINT ( 'NONE',  ( -58.88972745734155723, 34.00000000000049027, -49.22241343995295892 ) ) ;
#5135 = CARTESIAN_POINT ( 'NONE',  ( 12.25360715556858082, 116.9391558507879409, 27.49998799999999477 ) ) ;
#5136 = VECTOR ( 'NONE', #19379, 1000.000000000000000 ) ;
#5137 = CARTESIAN_POINT ( 'NONE',  ( 14.99999662536863632, -77.94228634059960825, -9.999999999999998224 ) ) ;
#5138 = ORIENTED_EDGE ( 'NONE', *, *, #19930, .T. ) ;
#5140 = AXIS2_PLACEMENT_3D ( 'NONE', #19575, #34207, #19764 ) ;
#5139 = DIRECTION ( 'NONE',  ( 1.000000000000000000, 0.000000000000000000, 0.000000000000000000 ) ) ;
#5141 = CARTESIAN_POINT ( 'NONE',  ( -70.80619744048887299, 84.18124734178336155, 32.50000000000000000 ) ) ;
#5142 = CARTESIAN_POINT ( 'NONE',  ( -65.00000337463102085, 25.98076211353317433, -5.000000000000000000 ) ) ;
#5143 = VECTOR ( 'NONE', #17765, 1000.000000000000000 ) ;
#5144 = VECTOR ( 'NONE', #10909, 1000.000000000000000 ) ;
#5145 = AXIS2_PLACEMENT_3D ( 'NONE', #15489, #30092, #35389 ) ;
#5146 = ORIENTED_EDGE ( 'NONE', *, *, #18566, .F. ) ;
#5147 = CIRCLE ( 'NONE', #30876, 3.000000000000008882 ) ;
#5148 = VERTEX_POINT ( 'NONE', #15455 ) ;
#5149 = ORIENTED_EDGE ( 'NONE', *, *, #31933, .T. ) ;
#5150 = CARTESIAN_POINT ( 'NONE',  ( 12.99999662536859901, 77.94228634059957983, -9.999999999999998224 ) ) ;
#5151 = CARTESIAN_POINT ( 'NONE',  ( 4.999996625368645198, 77.94228634059957983, 17.49999999999999645 ) ) ;
#5152 = ORIENTED_EDGE ( 'NONE', *, *, #17840, .F. ) ;
#5153 = VECTOR ( 'NONE', #36108, 1000.000000000000000 ) ;
#5154 = DIRECTION ( 'NONE',  ( -0.7650473262243666639, 0.6439740589782693148, -0.000000000000000000 ) ) ;
#5155 = DIRECTION ( 'NONE',  ( 1.000000000000000000, 0.000000000000000000, 0.000000000000000000 ) ) ;
#5156 = ORIENTED_EDGE ( 'NONE', *, *, #727, .F. ) ;
#5157 = EDGE_CURVE ( 'NONE', #21984, #10822, #27060, .T. ) ;
#5158 = CARTESIAN_POINT ( 'NONE',  ( -56.67878100130369035, 27.78182860042797131, -4.999999999999997335 ) ) ;
#5159 = ORIENTED_EDGE ( 'NONE', *, *, #27853, .F. ) ;
#5160 = PLANE ( 'NONE',  #24343 ) ;
#5161 = VECTOR ( 'NONE', #26343, 1000.000000000000000 ) ;
#5162 = DIRECTION ( 'NONE',  ( 0.000000000000000000, 0.000000000000000000, 1.000000000000000000 ) ) ;
#5163 = CARTESIAN_POINT ( 'NONE',  ( -29.97040610772328861, 71.28181329121154874, 12.50000000000000000 ) ) ;
#5164 = VECTOR ( 'NONE', #15215, 1000.000000000000114 ) ;
#5165 = ORIENTED_EDGE ( 'NONE', *, *, #800, .F. ) ;
#5166 = MECHANICAL_DESIGN_GEOMETRIC_PRESENTATION_REPRESENTATION (  '', ( #27994 ), #35709 ) ;
#5167 = CARTESIAN_POINT ( 'NONE',  ( -58.88972745734155723, 34.00000000000049027, -4.999999999999997335 ) ) ;
#5168 = CIRCLE ( 'NONE', #10542, 30.00000000000000000 ) ;
#5169 = CIRCLE ( 'NONE', #3364, 2.000000000000001776 ) ;
#5170 = CIRCLE ( 'NONE', #5757, 2.000000000000001776 ) ;
#5171 = DIRECTION ( 'NONE',  ( 1.000000000000000000, 0.000000000000000000, 0.000000000000000000 ) ) ;
#5172 = FACE_OUTER_BOUND ( 'NONE', #19366, .T. ) ;
#5173 = CIRCLE ( 'NONE', #23126, 2.000000000000001776 ) ;
#5174 = ORIENTED_EDGE ( 'NONE', *, *, #33991, .F. ) ;
#5175 = DIRECTION ( 'NONE',  ( 0.000000000000000000, 0.000000000000000000, -1.000000000000000000 ) ) ;
#5176 = CARTESIAN_POINT ( 'NONE',  ( 62.99999662536839651, -60.62177826491080168, 17.49999999999999645 ) ) ;
#5177 = ORIENTED_EDGE ( 'NONE', *, *, #26667, .T. ) ;
#5178 = DIRECTION ( 'NONE',  ( 1.000000000000000000, 0.000000000000000000, 0.000000000000000000 ) ) ;
#5179 = CARTESIAN_POINT ( 'NONE',  ( 17.99999662536858125, 86.60254037844397601, -5.000000000000000000 ) ) ;
#5180 = DIRECTION ( 'NONE',  ( 1.000000000000000000, 0.000000000000000000, 0.000000000000000000 ) ) ;
#5181 = ADVANCED_FACE ( 'NONE', ( #32325 ), #28520, .T. ) ;
#5182 = DIRECTION ( 'NONE',  ( -1.000000000000000000, 0.000000000000000000, 0.000000000000000000 ) ) ;
#5183 = CIRCLE ( 'NONE', #33340, 2.000000000000001776 ) ;
#5184 = ORIENTED_EDGE ( 'NONE', *, *, #29825, .F. ) ;
#5185 = VERTEX_POINT ( 'NONE', #6643 ) ;
#5186 = EDGE_CURVE ( 'NONE', #32494, #5564, #9976, .T. ) ;
#5187 = DIRECTION ( 'NONE',  ( 0.000000000000000000, 0.000000000000000000, 1.000000000000000000 ) ) ;
#5188 = CYLINDRICAL_SURFACE ( 'NONE', #14132, 2.000000000000001776 ) ;
#5189 = AXIS2_PLACEMENT_3D ( 'NONE', #31720, #23476, #6053 ) ;
#5190 = DIRECTION ( 'NONE',  ( 0.000000000000000000, 0.000000000000000000, 1.000000000000000000 ) ) ;
#5192 = ORIENTED_EDGE ( 'NONE', *, *, #2949, .T. ) ;
#5191 = EDGE_CURVE ( 'NONE', #34395, #35595, #12968, .T. ) ;
#5193 = VERTEX_POINT ( 'NONE', #4381 ) ;
#5194 = CARTESIAN_POINT ( 'NONE',  ( 4.999999999999999112, -0.4954705650270037065, -1.356946781501389143E-15 ) ) ;
#5195 = DIRECTION ( 'NONE',  ( -0.000000000000000000, -0.000000000000000000, -1.000000000000000000 ) ) ;
#5196 = CARTESIAN_POINT ( 'NONE',  ( -73.00000337463097821, 25.98076211353318854, -9.999999999999998224 ) ) ;
#5197 = VECTOR ( 'NONE', #24818, 1000.000000000000000 ) ;
#5198 = ORIENTED_EDGE ( 'NONE', *, *, #15391, .F. ) ;
#5199 = CIRCLE ( 'NONE', #26737, 2.000000000000001776 ) ;
#5200 = ORIENTED_EDGE ( 'NONE', *, *, #23436, .F. ) ;
#5201 = CARTESIAN_POINT ( 'NONE',  ( -65.00000000000000000, 0.000000000000000000, 12.49999999999999822 ) ) ;
#5202 = AXIS2_PLACEMENT_3D ( 'NONE', #870, #12287, #23762 ) ;
#5203 = DIRECTION ( 'NONE',  ( 0.000000000000000000, 0.000000000000000000, 1.000000000000000000 ) ) ;
#5204 = ORIENTED_EDGE ( 'NONE', *, *, #28086, .F. ) ;
#5205 = EDGE_CURVE ( 'NONE', #30153, #35680, #8773, .T. ) ;
#5206 = CARTESIAN_POINT ( 'NONE',  ( 0.000000000000000000, 101.4480229402710592, -24.99999999999999645 ) ) ;
#5207 = ORIENTED_EDGE ( 'NONE', *, *, #12798, .T. ) ;
#5208 = FACE_BOUND ( 'NONE', #25050, .T. ) ;
#5209 = AXIS2_PLACEMENT_3D ( 'NONE', #31707, #6040, #14842 ) ;
#5210 = CARTESIAN_POINT ( 'NONE',  ( 0.000000000000000000, 0.000000000000000000, 5.000000000000000000 ) ) ;
#5211 = CARTESIAN_POINT ( 'NONE',  ( 4.296971609539972370, 3.292644976428022119, -4.096693167834859928 ) ) ;
#5212 = ORIENTED_EDGE ( 'NONE', *, *, #8159, .T. ) ;
#5213 = CARTESIAN_POINT ( 'NONE',  ( 0.000000000000000000, 55.00000000000000000, 10.70000000000000107 ) ) ;
#5214 = AXIS2_PLACEMENT_3D ( 'NONE', #32848, #15966, #13153 ) ;
#5215 = EDGE_CURVE ( 'NONE', #18101, #31393, #7012, .T. ) ;
#5216 = CARTESIAN_POINT ( 'NONE',  ( 0.000000000000000000, 81.28776890242656350, -29.99999999999985434 ) ) ;
#5217 = AXIS2_PLACEMENT_3D ( 'NONE', #21560, #24571, #32991 ) ;
#5218 = FACE_OUTER_BOUND ( 'NONE', #16123, .T. ) ;
#5219 = DIRECTION ( 'NONE',  ( 1.000000000000000000, 0.000000000000000000, 0.000000000000000000 ) ) ;
#5220 = CIRCLE ( 'NONE', #7520, 33.00000000000001421 ) ;
#5221 = EDGE_CURVE ( 'NONE', #5127, #18549, #14150, .T. ) ;
#5222 = VERTEX_POINT ( 'NONE', #26891 ) ;
#5223 = FACE_OUTER_BOUND ( 'NONE', #15709, .T. ) ;
#5224 = ADVANCED_FACE ( 'NONE', ( #35147 ), #14344, .F. ) ;
#5225 = CARTESIAN_POINT ( 'NONE',  ( 5.999999999999998224, 145.0000000000000568, 32.55002500000000509 ) ) ;
#5226 = DIRECTION ( 'NONE',  ( 1.000000000000000000, 0.000000000000000000, 0.000000000000000000 ) ) ;
#5227 = VECTOR ( 'NONE', #23511, 1000.000000000000000 ) ;
#5228 = VECTOR ( 'NONE', #4138, 1000.000000000000000 ) ;
#5229 = ORIENTED_EDGE ( 'NONE', *, *, #22616, .F. ) ;
#5230 = VECTOR ( 'NONE', #7010, 1000.000000000000000 ) ;
#5231 = AXIS2_PLACEMENT_3D ( 'NONE', #16381, #19378, #10572 ) ;
#5232 = EDGE_LOOP ( 'NONE', ( #24060, #23051 ) ) ;
#5233 = DIRECTION ( 'NONE',  ( 0.000000000000000000, 0.000000000000000000, 1.000000000000000000 ) ) ;
#5234 = EDGE_LOOP ( 'NONE', ( #20249, #28405, #5656, #36141 ) ) ;
#5235 = EDGE_CURVE ( 'NONE', #31695, #203, #29101, .T. ) ;
#5236 = DIRECTION ( 'NONE',  ( -1.000000000000000000, 0.000000000000000000, 0.000000000000000000 ) ) ;
#5237 = CYLINDRICAL_SURFACE ( 'NONE', #14784, 2.000000000000001776 ) ;
#5238 = AXIS2_PLACEMENT_3D ( 'NONE', #21591, #18192, #9591 ) ;
#5239 = DIRECTION ( 'NONE',  ( 0.000000000000000000, 0.000000000000000000, 1.000000000000000000 ) ) ;
#5240 = EDGE_CURVE ( 'NONE', #14355, #7880, #24358, .T. ) ;
#5241 = DIRECTION ( 'NONE',  ( 0.000000000000000000, 0.000000000000000000, 1.000000000000000000 ) ) ;
#5242 = CARTESIAN_POINT ( 'NONE',  ( 17.99999662536858835, 69.28203230275516944, 12.50000000000000000 ) ) ;
#5243 = DIRECTION ( 'NONE',  ( -0.5000000000000098810, -0.8660254037844328234, 0.000000000000000000 ) ) ;
#5244 = DIRECTION ( 'NONE',  ( 0.000000000000000000, 0.000000000000000000, 1.000000000000000000 ) ) ;
#5245 = CIRCLE ( 'NONE', #6439, 8.500000000000000000 ) ;
#5246 = CYLINDRICAL_SURFACE ( 'NONE', #19077, 2.000000000000001776 ) ;
#5247 = VERTEX_POINT ( 'NONE', #21635 ) ;
#5248 = VECTOR ( 'NONE', #16463, 1000.000000000000000 ) ;
#5249 = ORIENTED_EDGE ( 'NONE', *, *, #34389, .T. ) ;
#5250 = DIRECTION ( 'NONE',  ( 0.000000000000000000, 0.000000000000000000, 1.000000000000000000 ) ) ;
#5251 = CIRCLE ( 'NONE', #26171, 2.000000000000001776 ) ;
#5252 = CYLINDRICAL_SURFACE ( 'NONE', #10967, 2.000000000000001776 ) ;
#5253 = LINE ( 'NONE', #22306, #16858 ) ;
#5254 = CARTESIAN_POINT ( 'NONE',  ( -31.83425564451526668, -89.42901512340343118, -5.000000000000011546 ) ) ;
#5255 = ORIENTED_EDGE ( 'NONE', *, *, #18796, .T. ) ;
#5256 = STYLED_ITEM ( 'NONE', ( #28128 ), #1854 ) ;
#5257 = AXIS2_PLACEMENT_3D ( 'NONE', #23023, #5982, #17411 ) ;
#5258 = VECTOR ( 'NONE', #30231, 1000.000000000000000 ) ;
#5259 = EDGE_CURVE ( 'NONE', #10522, #31822, #7379, .T. ) ;
#5260 = CARTESIAN_POINT ( 'NONE',  ( 4.999996625368676284, -77.94228634059960825, 12.50000000000000000 ) ) ;
#5261 = VERTEX_POINT ( 'NONE', #23905 ) ;
#5262 = EDGE_LOOP ( 'NONE', ( #29125, #22914 ) ) ;
#5263 = CARTESIAN_POINT ( 'NONE',  ( 0.000000000000000000, -1.467624384280027172, 2.542000000000001592 ) ) ;
#5264 = ORIENTED_EDGE ( 'NONE', *, *, #9126, .F. ) ;
#5265 = CIRCLE ( 'NONE', #19055, 6.000000000000005329 ) ;
#5266 = FILL_AREA_STYLE ('',( #5811 ) ) ;
#5267 = DIRECTION ( 'NONE',  ( 0.000000000000000000, 0.000000000000000000, 1.000000000000000000 ) ) ;
#5268 = EDGE_CURVE ( 'NONE', #1000, #35211, #7751, .T. ) ;
#5269 = PRODUCT_DEFINITION_SHAPE ( 'NONE', 'NONE',  #22359 ) ;
#5270 = FACE_OUTER_BOUND ( 'NONE', #36473, .T. ) ;
#5271 = CIRCLE ( 'NONE', #11220, 2.500000000000000000 ) ;
#5272 = LINE ( 'NONE', #16707, #22079 ) ;
#5273 = EDGE_CURVE ( 'NONE', #13581, #14423, #4584, .T. ) ;
#5274 = ORIENTED_EDGE ( 'NONE', *, *, #22868, .F. ) ;
#5275 = ORIENTED_EDGE ( 'NONE', *, *, #12604, .T. ) ;
#5276 = AXIS2_PLACEMENT_3D ( 'NONE', #18096, #29354, #15483 ) ;
#5277 = VECTOR ( 'NONE', #33202, 1000.000000000000000 ) ;
#5278 = ORIENTED_EDGE ( 'NONE', *, *, #5323, .T. ) ;
#5279 = VECTOR ( 'NONE', #23564, 1000.000000000000000 ) ;
#5280 = ORIENTED_EDGE ( 'NONE', *, *, #31373, .F. ) ;
#5281 = CIRCLE ( 'NONE', #11233, 2.000000000000001776 ) ;
#5282 = ORIENTED_EDGE ( 'NONE', *, *, #36128, .F. ) ;
#5283 = CARTESIAN_POINT ( 'NONE',  ( -55.88972745734155012, 34.00000000000049027, 12.49999999999999822 ) ) ;
#5284 = LINE ( 'NONE', #27950, #32752 ) ;
#5285 = CARTESIAN_POINT ( 'NONE',  ( -32.00000337463119848, -69.28203230275522628, 12.50000000000000000 ) ) ;
#5286 = CARTESIAN_POINT ( 'NONE',  ( 0.3000000000000016542, 0.000000000000000000, 0.000000000000000000 ) ) ;
#5287 = CARTESIAN_POINT ( 'NONE',  ( -80.00000337463096400, -34.64101615137762025, -5.000000000000000000 ) ) ;
#5288 = EDGE_LOOP ( 'NONE', ( #10397, #15064, #18152, #32149 ) ) ;
#5289 = DIRECTION ( 'NONE',  ( 0.000000000000000000, 0.000000000000000000, 1.000000000000000000 ) ) ;
#5290 = AXIS2_PLACEMENT_3D ( 'NONE', #13545, #10136, #33169 ) ;
#5291 = EDGE_CURVE ( 'NONE', #31944, #11785, #16372, .T. ) ;
#5292 = DIRECTION ( 'NONE',  ( 0.000000000000000000, 0.000000000000000000, -1.000000000000000000 ) ) ;
#5293 = VERTEX_POINT ( 'NONE', #25013 ) ;
#5294 = DIRECTION ( 'NONE',  ( 0.000000000000000000, 0.000000000000000000, 1.000000000000000000 ) ) ;
#5295 = FACE_OUTER_BOUND ( 'NONE', #32949, .T. ) ;
#5296 = VECTOR ( 'NONE', #4296, 1000.000000000000000 ) ;
#5297 = ORIENTED_EDGE ( 'NONE', *, *, #26934, .F. ) ;
#5298 = ORIENTED_EDGE ( 'NONE', *, *, #23183, .F. ) ;
#5299 = DIRECTION ( 'NONE',  ( 0.000000000000000000, 0.000000000000000000, 1.000000000000000000 ) ) ;
#5300 = CIRCLE ( 'NONE', #30417, 2.000000000000001776 ) ;
#5301 = CARTESIAN_POINT ( 'NONE',  ( -0.6806757771964039305, 5.380514348701066041, -3.838711833385082262 ) ) ;
#5302 = CARTESIAN_POINT ( 'NONE',  ( 3.417629563432208251, -3.800333343458275781, -3.719399823475529665 ) ) ;
#5303 = CARTESIAN_POINT ( 'NONE',  ( -92.00000337463090716, -1.016341149603137227E-14, -5.000000000000000000 ) ) ;
#5304 = ORIENTED_EDGE ( 'NONE', *, *, #33888, .T. ) ;
#5305 = ORIENTED_EDGE ( 'NONE', *, *, #26190, .F. ) ;
#5306 = AXIS2_PLACEMENT_3D ( 'NONE', #31793, #23388, #3304 ) ;
#5307 = CIRCLE ( 'NONE', #35174, 2.000000000000001776 ) ;
#5308 = CARTESIAN_POINT ( 'NONE',  ( -40.99999999999999289, -103.4105893997321743, 27.50000000000000000 ) ) ;
#5309 = ADVANCED_FACE ( 'NONE', ( #16204 ), #4770, .F. ) ;
#5310 = AXIS2_PLACEMENT_3D ( 'NONE', #35277, #9374, #20811 ) ;
#5311 = ORIENTED_EDGE ( 'NONE', *, *, #28365, .F. ) ;
#5312 = ADVANCED_FACE ( 'NONE', ( #19561 ), #33243, .F. ) ;
#5313 = DIRECTION ( 'NONE',  ( -1.000000000000000000, 0.000000000000000000, 0.000000000000000000 ) ) ;
#5314 = ORIENTED_EDGE ( 'NONE', *, *, #33427, .F. ) ;
#5315 = AXIS2_PLACEMENT_3D ( 'NONE', #3199, #380, #31324 ) ;
#5316 = DIRECTION ( 'NONE',  ( 1.000000000000000000, 0.000000000000000000, 0.000000000000000000 ) ) ;
#5317 = ADVANCED_FACE ( 'NONE', ( #27795 ), #36448, .F. ) ;
#5318 = AXIS2_PLACEMENT_3D ( 'NONE', #9465, #26340, #6464 ) ;
#5319 = CARTESIAN_POINT ( 'NONE',  ( -48.00000337463110611, -69.28203230275519786, 17.49999999999999645 ) ) ;
#5320 = DIRECTION ( 'NONE',  ( 0.000000000000000000, 0.000000000000000000, 1.000000000000000000 ) ) ;
#5321 = ORIENTED_EDGE ( 'NONE', *, *, #15546, .T. ) ;
#5322 = ORIENTED_EDGE ( 'NONE', *, *, #32012, .F. ) ;
#5323 = EDGE_CURVE ( 'NONE', #9159, #12004, #30991, .T. ) ;
#5324 = DIRECTION ( 'NONE',  ( 1.224646799147353207E-16, 1.000000000000000000, 0.000000000000000000 ) ) ;
#5325 = FACE_OUTER_BOUND ( 'NONE', #26325, .T. ) ;
#5326 = ADVANCED_FACE ( 'NONE', ( #5325 ), #16922, .F. ) ;
#5327 = CYLINDRICAL_SURFACE ( 'NONE', #24678, 2.000000000000001776 ) ;
#5328 = CARTESIAN_POINT ( 'NONE',  ( -70.00000337463099243, 34.64101615137758472, -9.999999999999998224 ) ) ;
#5329 = ORIENTED_EDGE ( 'NONE', *, *, #24410, .F. ) ;
#5330 = DIRECTION ( 'NONE',  ( 0.000000000000000000, 0.000000000000000000, -1.000000000000000000 ) ) ;
#5331 = CONICAL_SURFACE ( 'NONE', #25087, 2.445500000000000007, 0.7853981633974749244 ) ;
#5332 = FACE_BOUND ( 'NONE', #18711, .T. ) ;
#5333 = EDGE_CURVE ( 'NONE', #20237, #26555, #25366, .T. ) ;
#5334 = CIRCLE ( 'NONE', #13694, 3.500000000000003109 ) ;
#5335 = DIRECTION ( 'NONE',  ( 0.000000000000000000, 0.000000000000000000, 1.000000000000000000 ) ) ;
#5336 = FACE_OUTER_BOUND ( 'NONE', #34082, .T. ) ;
#5337 = LINE ( 'NONE', #8127, #320 ) ;
#5338 = EDGE_CURVE ( 'NONE', #1224, #7201, #2497, .T. ) ;
#5339 = CARTESIAN_POINT ( 'NONE',  ( 19.99999662536861678, -86.60254037844400443, -9.999999999999998224 ) ) ;
#5340 = EDGE_CURVE ( 'NONE', #2614, #18383, #36798, .T. ) ;
#5341 = FACE_OUTER_BOUND ( 'NONE', #18621, .T. ) ;
#5342 = EDGE_CURVE ( 'NONE', #27334, #28791, #10922, .T. ) ;
#5343 = ADVANCED_FACE ( 'NONE', ( #27992 ), #36252, .F. ) ;
#5344 = CIRCLE ( 'NONE', #20306, 3.000000000000002665 ) ;
#5345 = CARTESIAN_POINT ( 'NONE',  ( 69.99999662536839651, 34.64101615137758472, -9.999999999999998224 ) ) ;
#5346 = ORIENTED_EDGE ( 'NONE', *, *, #24733, .T. ) ;
#5347 = DIRECTION ( 'NONE',  ( -1.000000000000000000, 0.000000000000000000, 0.000000000000000000 ) ) ;
#5348 = DIRECTION ( 'NONE',  ( -1.000000000000000000, 0.000000000000000000, 0.000000000000000000 ) ) ;
#5349 = PLANE ( 'NONE',  #17981 ) ;
#5350 = ORIENTED_EDGE ( 'NONE', *, *, #949, .F. ) ;
#5351 = EDGE_LOOP ( 'NONE', ( #20713, #34438, #30276, #15553 ) ) ;
#5352 = AXIS2_PLACEMENT_3D ( 'NONE', #33543, #28082, #19280 ) ;
#5353 = VERTEX_POINT ( 'NONE', #2318 ) ;
#5354 = CARTESIAN_POINT ( 'NONE',  ( 24.99999662536859546, -77.94228634059960825, -5.000000000000000000 ) ) ;
#5355 = FACE_OUTER_BOUND ( 'NONE', #29675, .T. ) ;
#5356 = ORIENTED_EDGE ( 'NONE', *, *, #3035, .T. ) ;
#5357 = CARTESIAN_POINT ( 'NONE',  ( 40.98360655737705827, 111.1639425680974540, -11.00000000000000355 ) ) ;
#5358 = AXIS2_PLACEMENT_3D ( 'NONE', #29580, #3908, #26792 ) ;
#5359 = ORIENTED_EDGE ( 'NONE', *, *, #14597, .F. ) ;
#5360 = CARTESIAN_POINT ( 'NONE',  ( -66.98486643701050980, 43.54686869003479899, 12.50000000000000000 ) ) ;
#5361 = ORIENTED_EDGE ( 'NONE', *, *, #31654, .F. ) ;
#5362 = DIRECTION ( 'NONE',  ( 0.000000000000000000, 0.000000000000000000, 1.000000000000000000 ) ) ;
#5363 = ORIENTED_EDGE ( 'NONE', *, *, #23431, .F. ) ;
#5364 = CARTESIAN_POINT ( 'NONE',  ( -43.00000337463111322, -77.94228634059960825, 17.49999999999999645 ) ) ;
#5365 = CYLINDRICAL_SURFACE ( 'NONE', #22147, 2.000000000000001776 ) ;
#5366 = VECTOR ( 'NONE', #7047, 1000.000000000000000 ) ;
#5367 = ORIENTED_EDGE ( 'NONE', *, *, #20817, .T. ) ;
#5368 = CARTESIAN_POINT ( 'NONE',  ( 72.99999662536836809, -8.660254037844401509, -9.999999999999998224 ) ) ;
#5369 = CONTEXT_DEPENDENT_SHAPE_REPRESENTATION ( #14462, #13388 ) ;
#5370 = CARTESIAN_POINT ( 'NONE',  ( 11.99999662536865763, -69.28203230275519786, -9.999999999999998224 ) ) ;
#5371 = DIRECTION ( 'NONE',  ( 1.000000000000000000, 0.000000000000000000, 0.000000000000000000 ) ) ;
#5372 = VECTOR ( 'NONE', #12269, 1000.000000000000000 ) ;
#5373 = VERTEX_POINT ( 'NONE', #4935 ) ;
#5374 = DIRECTION ( 'NONE',  ( 1.000000000000000000, 0.000000000000000000, 0.000000000000000000 ) ) ;
#5375 = CARTESIAN_POINT ( 'NONE',  ( 51.68138994340220904, -113.8157894736842053, 32.50000000000000000 ) ) ;
#5376 = EDGE_LOOP ( 'NONE', ( #29401, #5304 ) ) ;
#5377 = CIRCLE ( 'NONE', #1158, 33.00000000000001421 ) ;
#5378 = CARTESIAN_POINT ( 'NONE',  ( -80.00000337463094979, 34.64101615137757051, -9.999999999999998224 ) ) ;
#5379 = LINE ( 'NONE', #16815, #6501 ) ;
#5380 = FACE_OUTER_BOUND ( 'NONE', #11142, .T. ) ;
#5381 = CARTESIAN_POINT ( 'NONE',  ( 37.50000000000000000, 103.4105893997321743, 32.50000000000000000 ) ) ;
#5382 = EDGE_LOOP ( 'NONE', ( #12370, #2552 ) ) ;
#5383 = CIRCLE ( 'NONE', #15540, 2.000000000000001776 ) ;
#5384 = EDGE_CURVE ( 'NONE', #17212, #23321, #2113, .T. ) ;
#5385 = ORIENTED_EDGE ( 'NONE', *, *, #29396, .T. ) ;
#5386 = CARTESIAN_POINT ( 'NONE',  ( 9.999996625368655856, -86.60254037844400443, 17.49999999999999645 ) ) ;
#5387 = DIRECTION ( 'NONE',  ( 0.000000000000000000, 0.000000000000000000, 1.000000000000000000 ) ) ;
#5388 = VERTEX_POINT ( 'NONE', #30441 ) ;
#5389 = ORIENTED_EDGE ( 'NONE', *, *, #33729, .T. ) ;
#5390 = CARTESIAN_POINT ( 'NONE',  ( 4.999999999999999112, -2.426004080355343095, -0.4213009713786298738 ) ) ;
#5391 = DIRECTION ( 'NONE',  ( 0.000000000000000000, 0.000000000000000000, -1.000000000000000000 ) ) ;
#5392 = CARTESIAN_POINT ( 'NONE',  ( -5.000000000000000000, 30.00000000000000355, -15.00000000000000000 ) ) ;
#5393 = AXIS2_PLACEMENT_3D ( 'NONE', #10598, #28029, #13592 ) ;
#5394 = ORIENTED_EDGE ( 'NONE', *, *, #30263, .F. ) ;
#5395 = EDGE_LOOP ( 'NONE', ( #19397, #34925 ) ) ;
#5396 = DIRECTION ( 'NONE',  ( -1.000000000000000000, 0.000000000000000000, 0.000000000000000000 ) ) ;
#5397 = AXIS2_PLACEMENT_3D ( 'NONE', #19317, #30176, #16317 ) ;
#5398 = DIRECTION ( 'NONE',  ( -0.000000000000000000, -0.000000000000000000, 1.000000000000000000 ) ) ;
#5399 = ORIENTED_EDGE ( 'NONE', *, *, #4497, .T. ) ;
#5400 = DIRECTION ( 'NONE',  ( -0.000000000000000000, 0.000000000000000000, -1.000000000000000000 ) ) ;
#5401 = ORIENTED_EDGE ( 'NONE', *, *, #729, .F. ) ;
#5403 = CIRCLE ( 'NONE', #13772, 2.000000000000001776 ) ;
#5402 = FACE_BOUND ( 'NONE', #21764, .T. ) ;
#5404 = ADVANCED_FACE ( 'NONE', ( #33631 ), #7934, .F. ) ;
#5405 = EDGE_CURVE ( 'NONE', #3127, #22150, #31510, .T. ) ;
#5406 = DIRECTION ( 'NONE',  ( 1.000000000000000000, 0.000000000000000000, 0.000000000000000000 ) ) ;
#5407 = AXIS2_PLACEMENT_3D ( 'NONE', #27495, #19419, #30838 ) ;
#5408 = CIRCLE ( 'NONE', #16193, 2.000000000000001776 ) ;
#5409 = ORIENTED_EDGE ( 'NONE', *, *, #461, .T. ) ;
#5410 = DIRECTION ( 'NONE',  ( 0.6793089147426122354, -0.7338524363598003530, -2.706694063014921639E-17 ) ) ;
#5411 = CYLINDRICAL_SURFACE ( 'NONE', #14661, 2.000000000000001776 ) ;
#5412 = ADVANCED_FACE ( 'NONE', ( #8118 ), #31181, .F. ) ;
#5413 = CARTESIAN_POINT ( 'NONE',  ( 3.000000000000000000, -2.201436576420042979, 1.271000000000003682 ) ) ;
#5414 = DIRECTION ( 'NONE',  ( 0.000000000000000000, 0.000000000000000000, 1.000000000000000000 ) ) ;
#5415 = VERTEX_POINT ( 'NONE', #25553 ) ;
#5416 = AXIS2_PLACEMENT_3D ( 'NONE', #229, #23120, #28913 ) ;
#5417 = DIRECTION ( 'NONE',  ( 1.000000000000000000, 0.000000000000000000, 0.000000000000000000 ) ) ;
#5418 = CARTESIAN_POINT ( 'NONE',  ( -72.00000337463102085, -51.96152422706641971, -9.999999999999998224 ) ) ;
#5419 = DIRECTION ( 'NONE',  ( -1.000000000000000000, 0.000000000000000000, 0.000000000000000000 ) ) ;
#5420 = AXIS2_PLACEMENT_3D ( 'NONE', #28121, #21749, #33183 ) ;
#5421 = EDGE_LOOP ( 'NONE', ( #14886, #17296, #2109, #5255 ) ) ;
#5422 = ORIENTED_EDGE ( 'NONE', *, *, #5986, .T. ) ;
#5423 = EDGE_CURVE ( 'NONE', #12033, #29187, #15352, .T. ) ;
#5424 = ORIENTED_EDGE ( 'NONE', *, *, #6812, .T. ) ;
#5425 = DIRECTION ( 'NONE',  ( 0.000000000000000000, 0.000000000000000000, 1.000000000000000000 ) ) ;
#5426 = CIRCLE ( 'NONE', #26373, 2.000000000000000000 ) ;
#5427 = DIRECTION ( 'NONE',  ( 1.000000000000000000, 0.000000000000000000, 0.000000000000000000 ) ) ;
#5428 = CARTESIAN_POINT ( 'NONE',  ( 0.000000000000000000, 89.94802294027088863, 27.49999999999999645 ) ) ;
#5429 = DIRECTION ( 'NONE',  ( 0.8660254037844415942, 0.4999999999999949485, 0.000000000000000000 ) ) ;
#5430 = CARTESIAN_POINT ( 'NONE',  ( 106.8157911955970718, -52.30559212667386504, 32.49999999999999289 ) ) ;
#5431 = DIRECTION ( 'NONE',  ( -1.000000000000000000, 0.000000000000000000, 0.000000000000000000 ) ) ;
#5432 = CARTESIAN_POINT ( 'NONE',  ( -65.00000337463102085, 25.98076211353317433, -5.000000000000000000 ) ) ;
#5433 = FACE_OUTER_BOUND ( 'NONE', #31445, .T. ) ;
#5434 = ORIENTED_EDGE ( 'NONE', *, *, #19072, .F. ) ;
#5435 =( BOUNDED_SURFACE ( )  B_SPLINE_SURFACE ( 3, 2, ( 
 ( #8625, #25714, #8281 ),
 ( #30759, #20059, #7903 ),
 ( #16522, #27953, #2278 ),
 ( #13713, #25170, #16722 ),
 ( #5464, #28147, #2465 ),
 ( #25332, #11068, #19712 ) ),
 .UNSPECIFIED., .F., .F., .T. ) 
 B_SPLINE_SURFACE_WITH_KNOTS ( ( 4, 2, 4 ),
 ( 3, 3 ),
 ( 0.02452952700623422036, 0.02759707648669815216, 0.03066462596716208050 ),
 ( 0.000000000000000000, 1.000000000000000000 ),
 .UNSPECIFIED. ) 
 GEOMETRIC_REPRESENTATION_ITEM ( )  RATIONAL_B_SPLINE_SURFACE ( (
 ( 1.000000000000000000, 0.8047781199190355839, 1.000000000000000000),
 ( 1.000000000000000000, 0.8123783328842254514, 1.000000000000000000),
 ( 1.000000000000000000, 0.8190665273150808945, 1.000000000000000000),
 ( 1.000000000000000000, 0.8192358268326377368, 1.000000000000000000),
 ( 1.000000000000000000, 0.8126132377674081253, 1.000000000000000000),
 ( 1.000000000000000000, 0.8047712443734141852, 1.000000000000000000) ) ) 
 REPRESENTATION_ITEM ( '' )  SURFACE ( )  );
#5436 = ORIENTED_EDGE ( 'NONE', *, *, #14831, .T. ) ;
#5437 = DIRECTION ( 'NONE',  ( -1.000000000000000000, 0.000000000000000000, 0.000000000000000000 ) ) ;
#5438 = EDGE_CURVE ( 'NONE', #16509, #21044, #29079, .T. ) ;
#5439 = CARTESIAN_POINT ( 'NONE',  ( 61.99999662536843914, -34.64101615137759893, 17.49999999999999645 ) ) ;
#5440 = DIRECTION ( 'NONE',  ( -1.000000000000000000, 0.000000000000000000, 0.000000000000000000 ) ) ;
#5441 = PLANE ( 'NONE',  #7126 ) ;
#5442 = ORIENTED_EDGE ( 'NONE', *, *, #30402, .T. ) ;
#5443 = UNCERTAINTY_MEASURE_WITH_UNIT (LENGTH_MEASURE( 1.000000000000000082E-05 ), #4517, 'distance_accuracy_value', 'NONE');
#5444 = EDGE_CURVE ( 'NONE', #16686, #11450, #31343, .T. ) ;
#5445 = FACE_BOUND ( 'NONE', #26045, .T. ) ;
#5446 = ORIENTED_EDGE ( 'NONE', *, *, #24969, .T. ) ;
#5447 = VERTEX_POINT ( 'NONE', #11305 ) ;
#5448 = ADVANCED_FACE ( 'NONE', ( #20294 ), #31526, .F. ) ;
#5449 = DIRECTION ( 'NONE',  ( -0.000000000000000000, 1.625241993126352989E-15, 1.000000000000000000 ) ) ;
#5450 = ORIENTED_EDGE ( 'NONE', *, *, #26667, .F. ) ;
#5451 = CARTESIAN_POINT ( 'NONE',  ( -3.374631334790434423E-06, 69.28203230275516944, -9.999999999999998224 ) ) ;
#5452 = CARTESIAN_POINT ( 'NONE',  ( 31.99999662536856704, 69.28203230275518365, -5.000000000000000000 ) ) ;
#5453 = EDGE_CURVE ( 'NONE', #21264, #21182, #19918, .T. ) ;
#5454 = DIRECTION ( 'NONE',  ( 1.000000000000000000, 0.000000000000000000, 0.000000000000000000 ) ) ;
#5455 = ORIENTED_EDGE ( 'NONE', *, *, #33103, .F. ) ;
#5456 = ORIENTED_EDGE ( 'NONE', *, *, #34431, .T. ) ;
#5457 = ORIENTED_EDGE ( 'NONE', *, *, #20207, .F. ) ;
#5458 = ORIENTED_EDGE ( 'NONE', *, *, #7849, .F. ) ;
#5459 = ORIENTED_EDGE ( 'NONE', *, *, #31836, .T. ) ;
#5460 = CARTESIAN_POINT ( 'NONE',  ( 54.99999662536844625, -60.62177826491080168, 12.50000000000000000 ) ) ;
#5461 = DIRECTION ( 'NONE',  ( 1.000000000000000000, 0.000000000000000000, 0.000000000000000000 ) ) ;
#5462 = DIRECTION ( 'NONE',  ( 0.000000000000000000, 0.000000000000000000, 1.000000000000000000 ) ) ;
#5463 = DIRECTION ( 'NONE',  ( 1.000000000000000000, 0.000000000000000000, 0.000000000000000000 ) ) ;
#5464 = CARTESIAN_POINT ( 'NONE',  ( 4.999999999999999112, 2.094490679362924546, -3.837546594561450863 ) ) ;
#5465 = VERTEX_POINT ( 'NONE', #23294 ) ;
#5466 = CARTESIAN_POINT ( 'NONE',  ( 94.55012560584681580, 9.234378588654079678, 27.50000000000000000 ) ) ;
#5467 = EDGE_CURVE ( 'NONE', #406, #20086, #32121, .T. ) ;
#5468 = CARTESIAN_POINT ( 'NONE',  ( -65.00000337463104927, -43.30127018922202353, -5.000000000000000000 ) ) ;
#5469 = DIRECTION ( 'NONE',  ( 0.4999999999999919509, -0.8660254037844433705, 0.000000000000000000 ) ) ;
#5470 = VERTEX_POINT ( 'NONE', #9035 ) ;
#5471 = CYLINDRICAL_SURFACE ( 'NONE', #11259, 2.000000000000001776 ) ;
#5472 = CARTESIAN_POINT ( 'NONE',  ( -51.13139720814379530, 27.50000000000055422, -10.00000000000000178 ) ) ;
#5473 = VERTEX_POINT ( 'NONE', #26096 ) ;
#5474 = ADVANCED_FACE ( 'NONE', ( #5666 ), #1601, .F. ) ;
#5475 = VERTEX_POINT ( 'NONE', #17107 ) ;
#5476 = CYLINDRICAL_SURFACE ( 'NONE', #18240, 2.000000000000001776 ) ;
#5477 = EDGE_CURVE ( 'NONE', #8103, #28577, #36937, .T. ) ;
#5478 = DIRECTION ( 'NONE',  ( 0.000000000000000000, 0.000000000000000000, -1.000000000000000000 ) ) ;
#5479 = FACE_BOUND ( 'NONE', #29963, .T. ) ;
#5480 = DIRECTION ( 'NONE',  ( 0.000000000000000000, 0.000000000000000000, 1.000000000000000000 ) ) ;
#5481 = ORIENTED_EDGE ( 'NONE', *, *, #1794, .F. ) ;
#5482 = ORIENTED_EDGE ( 'NONE', *, *, #6964, .F. ) ;
#5483 = DIRECTION ( 'NONE',  ( -1.000000000000000000, -8.994862468027885935E-16, 0.000000000000000000 ) ) ;
#5484 = ORIENTED_EDGE ( 'NONE', *, *, #36172, .F. ) ;
#5485 = AXIS2_PLACEMENT_3D ( 'NONE', #19860, #14033, #25485 ) ;
#5486 = DIRECTION ( 'NONE',  ( -1.000000000000000000, 0.000000000000000000, 0.000000000000000000 ) ) ;
#5487 = ORIENTED_EDGE ( 'NONE', *, *, #33894, .F. ) ;
#5488 = VERTEX_POINT ( 'NONE', #6214 ) ;
#5489 = CARTESIAN_POINT ( 'NONE',  ( 0.000000000000000000, 86.49289592134881843, -29.01554445662268833 ) ) ;
#5490 = CYLINDRICAL_SURFACE ( 'NONE', #26206, 3.500000000000003109 ) ;
#5491 = EDGE_CURVE ( 'NONE', #281, #3592, #10696, .T. ) ;
#5492 = DIRECTION ( 'NONE',  ( -1.000000000000000000, 0.000000000000000000, 0.000000000000000000 ) ) ;
#5493 = VERTEX_POINT ( 'NONE', #34359 ) ;
#5494 = ORIENTED_EDGE ( 'NONE', *, *, #21590, .F. ) ;
#5495 = DIRECTION ( 'NONE',  ( 0.000000000000000000, 0.000000000000000000, 1.000000000000000000 ) ) ;
#5496 = DIRECTION ( 'NONE',  ( 1.000000000000000000, 0.000000000000000000, 0.000000000000000000 ) ) ;
#5497 = CARTESIAN_POINT ( 'NONE',  ( 13.89091430021463935, 62.33939050065170306, 12.49999999999999822 ) ) ;
#5498 = DIRECTION ( 'NONE',  ( 1.000000000000000000, -1.047444401652940007E-14, 0.000000000000000000 ) ) ;
#5499 = ORIENTED_EDGE ( 'NONE', *, *, #11864, .F. ) ;
#5500 = CARTESIAN_POINT ( 'NONE',  ( -36.97203788308986105, 58.48108235278859013, -4.999999999999997335 ) ) ;
#5501 = FACE_BOUND ( 'NONE', #35424, .T. ) ;
#5502 = DIRECTION ( 'NONE',  ( 0.000000000000000000, 0.4999999999999991118, -0.8660254037844391517 ) ) ;
#5503 = CARTESIAN_POINT ( 'NONE',  ( -90.60231327712325822, -15.97563234535699017, -49.86561046011506448 ) ) ;
#5504 = DIRECTION ( 'NONE',  ( -0.000000000000000000, 0.8660254037844391517, 0.4999999999999990563 ) ) ;
#5505 = FACE_OUTER_BOUND ( 'NONE', #5873, .T. ) ;
#5506 = ADVANCED_FACE ( 'NONE', ( #26289 ), #599, .T. ) ;
#5507 = DIRECTION ( 'NONE',  ( 0.000000000000000000, 0.000000000000000000, 1.000000000000000000 ) ) ;
#5508 = VECTOR ( 'NONE', #33063, 1000.000000000000000 ) ;
#5509 = CARTESIAN_POINT ( 'NONE',  ( -77.93343913441745485, -72.12058696850748163, 32.50002500000000083 ) ) ;
#5510 = ORIENTED_EDGE ( 'NONE', *, *, #5029, .T. ) ;
#5511 = EDGE_CURVE ( 'NONE', #29140, #34620, #8490, .T. ) ;
#5512 = CARTESIAN_POINT ( 'NONE',  ( 42.97377950131527058, 96.90768712682506703, -11.00000000000000000 ) ) ;
#5513 = FACE_OUTER_BOUND ( 'NONE', #20011, .T. ) ;
#5514 = CARTESIAN_POINT ( 'NONE',  ( 139.0000000000000284, -5.056524707326808249E-13, 32.50000000000000000 ) ) ;
#5515 = EDGE_LOOP ( 'NONE', ( #34661, #27608, #7035, #21329 ) ) ;
#5516 = ADVANCED_FACE ( 'NONE', ( #211 ), #28346, .F. ) ;
#5517 = ORIENTED_EDGE ( 'NONE', *, *, #16507, .T. ) ;
#5518 = EDGE_LOOP ( 'NONE', ( #36607, #1065, #18068, #14849 ) ) ;
#5519 = CYLINDRICAL_SURFACE ( 'NONE', #12331, 1.999999999999998224 ) ;
#5520 = DIRECTION ( 'NONE',  ( 0.000000000000000000, 0.000000000000000000, 1.000000000000000000 ) ) ;
#5521 = EDGE_CURVE ( 'NONE', #15624, #8981, #11642, .T. ) ;
#5522 = ORIENTED_EDGE ( 'NONE', *, *, #28428, .F. ) ;
#5523 = EDGE_CURVE ( 'NONE', #24614, #28759, #27440, .T. ) ;
#5524 = LINE ( 'NONE', #33837, #21516 ) ;
#5525 = ORIENTED_EDGE ( 'NONE', *, *, #6407, .T. ) ;
#5526 = CARTESIAN_POINT ( 'NONE',  ( 23.27270485391772681, -104.1536085790715305, 32.50000000000000711 ) ) ;
#5527 = ORIENTED_EDGE ( 'NONE', *, *, #10048, .F. ) ;
#5528 = DIRECTION ( 'NONE',  ( 0.000000000000000000, 0.000000000000000000, 1.000000000000000000 ) ) ;
#5529 = EDGE_CURVE ( 'NONE', #28630, #19593, #28733, .T. ) ;
#5530 = VERTEX_POINT ( 'NONE', #34546 ) ;
#5531 = EDGE_CURVE ( 'NONE', #17059, #7036, #14859, .T. ) ;
#5532 = DIRECTION ( 'NONE',  ( 0.000000000000000000, 0.000000000000000000, 1.000000000000000000 ) ) ;
#5533 = CARTESIAN_POINT ( 'NONE',  ( 33.99999999999986500, -58.88972745734191250, 12.49999999999999822 ) ) ;
#5534 = EDGE_CURVE ( 'NONE', #19701, #31662, #11276, .T. ) ;
#5535 = ADVANCED_FACE ( 'NONE', ( #29277 ), #4678, .F. ) ;
#5536 = ORIENTED_EDGE ( 'NONE', *, *, #8297, .T. ) ;
#5537 = DIRECTION ( 'NONE',  ( 0.000000000000000000, 0.000000000000000000, 1.000000000000000000 ) ) ;
#5538 = CONTEXT_DEPENDENT_SHAPE_REPRESENTATION ( #9187, #4736 ) ;
#5539 = DIRECTION ( 'NONE',  ( 1.000000000000000000, 0.000000000000000000, 0.000000000000000000 ) ) ;
#5540 = CARTESIAN_POINT ( 'NONE',  ( -85.00000337463092137, 8.660254037844389075, -9.999999999999998224 ) ) ;
#5541 = ORIENTED_EDGE ( 'NONE', *, *, #23082, .T. ) ;
#5542 = FACE_OUTER_BOUND ( 'NONE', #13616, .T. ) ;
#5543 = DIRECTION ( 'NONE',  ( 0.000000000000000000, 0.000000000000000000, 1.000000000000000000 ) ) ;
#5544 = ORIENTED_EDGE ( 'NONE', *, *, #34515, .F. ) ;
#5545 = CYLINDRICAL_SURFACE ( 'NONE', #425, 2.000000000000001776 ) ;
#5546 = FACE_OUTER_BOUND ( 'NONE', #27278, .T. ) ;
#5547 = CARTESIAN_POINT ( 'NONE',  ( 15.97563234535730814, -90.60231327712320137, 12.49999999999999822 ) ) ;
#5548 = DIRECTION ( 'NONE',  ( 0.000000000000000000, 0.000000000000000000, -1.000000000000000000 ) ) ;
#5549 = ORIENTED_EDGE ( 'NONE', *, *, #22393, .F. ) ;
#5550 = ORIENTED_EDGE ( 'NONE', *, *, #2321, .T. ) ;
#5551 = DIRECTION ( 'NONE',  ( -1.000000000000000000, 0.000000000000000000, -0.000000000000000000 ) ) ;
#5552 = CARTESIAN_POINT ( 'NONE',  ( 51.99999662536847467, 51.96152422706637708, -9.999999999999998224 ) ) ;
#5553 = VERTEX_POINT ( 'NONE', #24729 ) ;
#5554 = VERTEX_POINT ( 'NONE', #7112 ) ;
#5555 = AXIS2_PLACEMENT_3D ( 'NONE', #5286, #22886, #16721 ) ;
#5556 = FACE_OUTER_BOUND ( 'NONE', #10774, .T. ) ;
#5557 = CYLINDRICAL_SURFACE ( 'NONE', #20799, 2.000000000000001776 ) ;
#5558 = FACE_OUTER_BOUND ( 'NONE', #3030, .T. ) ;
#5559 = VERTEX_POINT ( 'NONE', #36162 ) ;
#5560 = VERTEX_POINT ( 'NONE', #12183 ) ;
#5561 = PRODUCT_DEFINITION_SHAPE ( 'NONE', 'NONE',  #10927 ) ;
#5562 = DIRECTION ( 'NONE',  ( 0.000000000000000000, 0.000000000000000000, -1.000000000000000000 ) ) ;
#5563 = CYLINDRICAL_SURFACE ( 'NONE', #26057, 1.999999999999998224 ) ;
#5564 = VERTEX_POINT ( 'NONE', #7666 ) ;
#5565 = DIRECTION ( 'NONE',  ( 1.000000000000000000, 0.000000000000000000, 0.000000000000000000 ) ) ;
#5566 = ORIENTED_EDGE ( 'NONE', *, *, #23638, .F. ) ;
#5567 = FACE_BOUND ( 'NONE', #28915, .T. ) ;
#5568 = EDGE_CURVE ( 'NONE', #24605, #30139, #767, .T. ) ;
#5569 = VECTOR ( 'NONE', #31697, 1000.000000000000000 ) ;
#5570 = CARTESIAN_POINT ( 'NONE',  ( 39.27785635698568711, -86.50000000000001421, 27.50000000000000000 ) ) ;
#5571 = EDGE_CURVE ( 'NONE', #34006, #9332, #23861, .T. ) ;
#5572 = EDGE_CURVE ( 'NONE', #21745, #6695, #28640, .T. ) ;
#5573 = ORIENTED_EDGE ( 'NONE', *, *, #32457, .T. ) ;
#5574 = DIRECTION ( 'NONE',  ( 0.000000000000000000, 0.000000000000000000, 1.000000000000000000 ) ) ;
#5575 = FACE_OUTER_BOUND ( 'NONE', #2183, .T. ) ;
#5576 = CIRCLE ( 'NONE', #12730, 2.000000000000001776 ) ;
#5577 = CARTESIAN_POINT ( 'NONE',  ( 0.000000000000000000, 89.94802294027094547, 32.49999999999999289 ) ) ;
#5578 = CYLINDRICAL_SURFACE ( 'NONE', #31084, 30.00000000000000000 ) ;
#5579 = VERTEX_POINT ( 'NONE', #13277 ) ;
#5580 = CARTESIAN_POINT ( 'NONE',  ( 0.3000000000000016542, 0.000000000000000000, 0.000000000000000000 ) ) ;
#5581 = DIRECTION ( 'NONE',  ( 0.000000000000000000, 0.000000000000000000, 1.000000000000000000 ) ) ;
#5582 = CARTESIAN_POINT ( 'NONE',  ( -85.00000337463092137, -25.98076211353322051, -5.000000000000000000 ) ) ;
#5583 = VERTEX_POINT ( 'NONE', #15033 ) ;
#5584 = VERTEX_POINT ( 'NONE', #26460 ) ;
#5585 = ORIENTED_EDGE ( 'NONE', *, *, #8745, .T. ) ;
#5586 = FACE_OUTER_BOUND ( 'NONE', #16492, .T. ) ;
#5587 = AXIS2_PLACEMENT_3D ( 'NONE', #18436, #6624, #32659 ) ;
#5588 = CARTESIAN_POINT ( 'NONE',  ( 6.123233995736731770E-16, -145.0000000000000568, 32.50000000000000000 ) ) ;
#5589 = EDGE_CURVE ( 'NONE', #26322, #36878, #21719, .T. ) ;
#5590 = AXIS2_PLACEMENT_3D ( 'NONE', #8786, #333, #35598 ) ;
#5591 = FACE_OUTER_BOUND ( 'NONE', #29113, .T. ) ;
#5592 = DIRECTION ( 'NONE',  ( -0.000000000000000000, -0.000000000000000000, 1.000000000000000000 ) ) ;
#5593 = CARTESIAN_POINT ( 'NONE',  ( 3.000000000000000000, 0.000000000000000000, 0.000000000000000000 ) ) ;
#5594 = CARTESIAN_POINT ( 'NONE',  ( -107.0735279439396095, -50.67946230268560015, 32.50000000000000711 ) ) ;
#5595 = LINE ( 'NONE', #527, #25016 ) ;
#5596 = DIRECTION ( 'NONE',  ( 1.000000000000000000, 0.000000000000000000, 0.000000000000000000 ) ) ;
#5597 = ORIENTED_EDGE ( 'NONE', *, *, #8868, .F. ) ;
#5598 = AXIS2_PLACEMENT_3D ( 'NONE', #36501, #10801, #28041 ) ;
#5599 = EDGE_LOOP ( 'NONE', ( #12777, #35180, #19986, #24095 ) ) ;
#5600 = DIRECTION ( 'NONE',  ( 0.000000000000000000, 0.000000000000000000, -1.000000000000000000 ) ) ;
#5601 = AXIS2_PLACEMENT_3D ( 'NONE', #36815, #14116, #23312 ) ;
#5602 = DIRECTION ( 'NONE',  ( 1.000000000000000000, 0.000000000000000000, 0.000000000000000000 ) ) ;
#5603 = DIRECTION ( 'NONE',  ( 0.000000000000000000, 0.000000000000000000, 1.000000000000000000 ) ) ;
#5604 = CARTESIAN_POINT ( 'NONE',  ( 3.000000000000000000, -1.467624384280027172, 2.542000000000001592 ) ) ;
#5605 = ORIENTED_EDGE ( 'NONE', *, *, #12567, .F. ) ;
#5606 = AXIS2_PLACEMENT_3D ( 'NONE', #20357, #5936, #11170 ) ;
#5607 = FACE_BOUND ( 'NONE', #429, .T. ) ;
#5608 = ORIENTED_EDGE ( 'NONE', *, *, #34183, .F. ) ;
#5609 = ORIENTED_EDGE ( 'NONE', *, *, #5438, .T. ) ;
#5610 = EDGE_CURVE ( 'NONE', #902, #3385, #37036, .T. ) ;
#5611 = CARTESIAN_POINT ( 'NONE',  ( -37.50000000000000000, 103.4105893997321743, 32.50000000000000000 ) ) ;
#5612 = ORIENTED_EDGE ( 'NONE', *, *, #16330, .F. ) ;
#5613 =( NAMED_UNIT ( * ) PLANE_ANGLE_UNIT ( ) SI_UNIT ( $, .RADIAN. ) );
#5614 = CARTESIAN_POINT ( 'NONE',  ( 74.99999662536836809, -8.660254037844401509, -9.999999999999998224 ) ) ;
#5615 = AXIS2_PLACEMENT_3D ( 'NONE', #14175, #19818, #8190 ) ;
#5616 = CARTESIAN_POINT ( 'NONE',  ( 54.99999662536844625, 60.62177826491077326, -9.999999999999998224 ) ) ;
#5617 = CARTESIAN_POINT ( 'NONE',  ( 69.99999662536838230, -51.96152422706639840, 12.50000000000000000 ) ) ;
#5618 = ORIENTED_EDGE ( 'NONE', *, *, #17941, .T. ) ;
#5619 = ORIENTED_EDGE ( 'NONE', *, *, #18404, .T. ) ;
#5620 = ORIENTED_EDGE ( 'NONE', *, *, #7055, .T. ) ;
#5621 = VECTOR ( 'NONE', #32537, 1000.000000000000000 ) ;
#5622 = ORIENTED_EDGE ( 'NONE', *, *, #5323, .F. ) ;
#5623 = EDGE_LOOP ( 'NONE', ( #5926, #32484, #2209, #27208 ) ) ;
#5624 = FACE_OUTER_BOUND ( 'NONE', #20039, .T. ) ;
#5625 = CIRCLE ( 'NONE', #14585, 2.000000000000001776 ) ;
#5626 = CARTESIAN_POINT ( 'NONE',  ( -57.00000337463111322, -43.30127018922202353, 17.49999999999999645 ) ) ;
#5627 = DIRECTION ( 'NONE',  ( 0.000000000000000000, -0.8660254037844419273, -0.4999999999999945599 ) ) ;
#5628 = DIRECTION ( 'NONE',  ( 1.000000000000000000, 0.000000000000000000, 0.000000000000000000 ) ) ;
#5629 = DIRECTION ( 'NONE',  ( 1.000000000000000000, 0.000000000000000000, 0.000000000000000000 ) ) ;
#5630 = ADVANCED_FACE ( 'NONE', ( #12899 ), #24355, .T. ) ;
#5631 = ORIENTED_EDGE ( 'NONE', *, *, #4870, .T. ) ;
#5632 = DIRECTION ( 'NONE',  ( 0.000000000000000000, 0.000000000000000000, 1.000000000000000000 ) ) ;
#5633 = LINE ( 'NONE', #17275, #8992 ) ;
#5634 = DIRECTION ( 'NONE',  ( 0.000000000000000000, 0.000000000000000000, 1.000000000000000000 ) ) ;
#5635 = ORIENTED_EDGE ( 'NONE', *, *, #14250, .T. ) ;
#5636 = DIRECTION ( 'NONE',  ( -1.000000000000000000, 0.000000000000000000, 0.000000000000000000 ) ) ;
#5637 = EDGE_CURVE ( 'NONE', #35831, #32910, #4476, .T. ) ;
#5638 = DIRECTION ( 'NONE',  ( -0.8660254037844455910, -0.4999999999999878431, 0.000000000000000000 ) ) ;
#5639 = EDGE_LOOP ( 'NONE', ( #15835, #8141, #21391, #25745 ) ) ;
#5640 = CIRCLE ( 'NONE', #25403, 2.000000000000001776 ) ;
#5641 = ORIENTED_EDGE ( 'NONE', *, *, #9003, .F. ) ;
#5642 = EDGE_CURVE ( 'NONE', #9908, #1442, #16292, .T. ) ;
#5643 = DIRECTION ( 'NONE',  ( 0.000000000000000000, 0.000000000000000000, 1.000000000000000000 ) ) ;
#5644 = DIRECTION ( 'NONE',  ( 1.000000000000000000, 0.000000000000000000, 0.000000000000000000 ) ) ;
#5645 = LINE ( 'NONE', #8301, #2515 ) ;
#5646 = DIRECTION ( 'NONE',  ( 0.000000000000000000, 0.000000000000000000, 1.000000000000000000 ) ) ;
#5647 = VERTEX_POINT ( 'NONE', #18559 ) ;
#5648 = ORIENTED_EDGE ( 'NONE', *, *, #31414, .T. ) ;
#5649 = CIRCLE ( 'NONE', #35593, 19.53925848833874213 ) ;
#5650 = CYLINDRICAL_SURFACE ( 'NONE', #3322, 2.000000000000001776 ) ;
#5651 = DIRECTION ( 'NONE',  ( -1.000000000000000000, 0.000000000000000000, 0.000000000000000000 ) ) ;
#5652 = VECTOR ( 'NONE', #24376, 1000.000000000000000 ) ;
#5653 = ORIENTED_EDGE ( 'NONE', *, *, #11287, .T. ) ;
#5654 = EDGE_CURVE ( 'NONE', #7645, #17074, #16663, .T. ) ;
#5655 = CARTESIAN_POINT ( 'NONE',  ( 83.49774710563264080, -24.66044155380014402, -5.000000000000000000 ) ) ;
#5656 = ORIENTED_EDGE ( 'NONE', *, *, #3410, .F. ) ;
#5657 = ORIENTED_EDGE ( 'NONE', *, *, #11577, .T. ) ;
#5658 = FACE_OUTER_BOUND ( 'NONE', #28293, .T. ) ;
#5659 = CARTESIAN_POINT ( 'NONE',  ( -48.00000337463109190, 51.96152422706637708, -5.000000000000000000 ) ) ;
#5660 = CIRCLE ( 'NONE', #13528, 2.000000000000000000 ) ;
#5661 = FACE_BOUND ( 'NONE', #5737, .T. ) ;
#5662 = EDGE_LOOP ( 'NONE', ( #14126, #34485, #29872, #15244 ) ) ;
#5663 = CIRCLE ( 'NONE', #10454, 95.00000000000001421 ) ;
#5664 = ORIENTED_EDGE ( 'NONE', *, *, #20191, .T. ) ;
#5665 = CARTESIAN_POINT ( 'NONE',  ( 0.000000000000000000, 81.28776890242656350, 37.49999999999985079 ) ) ;
#5666 = FACE_OUTER_BOUND ( 'NONE', #32992, .T. ) ;
#5667 = EDGE_CURVE ( 'NONE', #5415, #16153, #19082, .T. ) ;
#5668 = DIRECTION ( 'NONE',  ( -1.000000000000000000, -0.000000000000000000, -0.000000000000000000 ) ) ;
#5669 = CARTESIAN_POINT ( 'NONE',  ( -62.97617850287781494, -4.279621169095772615, -4.999999999999997335 ) ) ;
#5670 = ORIENTED_EDGE ( 'NONE', *, *, #5921, .T. ) ;
#5671 = DIRECTION ( 'NONE',  ( 0.000000000000000000, 0.000000000000000000, 1.000000000000000000 ) ) ;
#5672 = ADVANCED_FACE ( 'NONE', ( #27344 ), #18730, .F. ) ;
#5673 = FACE_BOUND ( 'NONE', #3440, .T. ) ;
#5674 = CYLINDRICAL_SURFACE ( 'NONE', #16616, 2.000000000000001776 ) ;
#5675 = CARTESIAN_POINT ( 'NONE',  ( 19.13981058454793072, -60.93295298010985306, 12.49999999999999822 ) ) ;
#5676 = FACE_OUTER_BOUND ( 'NONE', #24590, .T. ) ;
#5677 = DIRECTION ( 'NONE',  ( 0.000000000000000000, 0.000000000000000000, 1.000000000000000000 ) ) ;
#5678 = CIRCLE ( 'NONE', #14046, 2.000000000000001776 ) ;
#5679 = EDGE_CURVE ( 'NONE', #23785, #29460, #28032, .T. ) ;
#5680 = CIRCLE ( 'NONE', #12233, 27.00000000000001421 ) ;
#5681 = DIRECTION ( 'NONE',  ( -1.000000000000000000, 0.000000000000000000, 0.000000000000000000 ) ) ;
#5682 = B_SPLINE_CURVE_WITH_KNOTS ( 'NONE', 3,
 ( #21895, #16649, #33341, #7281 ),
 .UNSPECIFIED., .F., .F.,
 ( 4, 4 ),
 ( 2.380735200870747991E-07, 0.002921158011986710323 ),
 .UNSPECIFIED. ) ;
#5683 = VECTOR ( 'NONE', #28276, 1000.000000000000000 ) ;
#5684 = CARTESIAN_POINT ( 'NONE',  ( -75.00000337463097821, 43.30127018922197379, -5.000000000000000000 ) ) ;
#5685 = ORIENTED_EDGE ( 'NONE', *, *, #1310, .T. ) ;
#5686 = DIRECTION ( 'NONE',  ( 1.000000000000000000, 0.000000000000000000, 0.000000000000000000 ) ) ;
#5687 = EDGE_CURVE ( 'NONE', #12630, #5993, #12467, .T. ) ;
#5688 = CARTESIAN_POINT ( 'NONE',  ( 74.99999662536836809, -8.660254037844401509, 12.50000000000000000 ) ) ;
#5689 = CARTESIAN_POINT ( 'NONE',  ( -25.00000337463120914, 77.94228634059957983, -9.999999999999998224 ) ) ;
#5690 = ORIENTED_EDGE ( 'NONE', *, *, #10819, .F. ) ;
#5691 = EDGE_LOOP ( 'NONE', ( #1645, #19043 ) ) ;
#5692 = ORIENTED_EDGE ( 'NONE', *, *, #35597, .T. ) ;
#5693 = ADVANCED_FACE ( 'NONE', ( #18913 ), #16116, .F. ) ;
#5694 = AXIS2_PLACEMENT_3D ( 'NONE', #32993, #7307, #13120 ) ;
#5695 = DIRECTION ( 'NONE',  ( 0.000000000000000000, 0.000000000000000000, 1.000000000000000000 ) ) ;
#5696 = DIRECTION ( 'NONE',  ( 0.000000000000000000, 0.000000000000000000, 1.000000000000000000 ) ) ;
#5697 = CIRCLE ( 'NONE', #10483, 2.000000000000001776 ) ;
#5698 = CARTESIAN_POINT ( 'NONE',  ( 14.80603122773119118, -87.83969979969866415, -4.999999999999997335 ) ) ;
#5699 = VERTEX_POINT ( 'NONE', #19290 ) ;
#5700 = CIRCLE ( 'NONE', #5732, 2.000000000000000000 ) ;
#5701 = VECTOR ( 'NONE', #34293, 1000.000000000000000 ) ;
#5702 = CARTESIAN_POINT ( 'NONE',  ( 2.999996625368645198, 77.94228634059957983, -5.000000000000000000 ) ) ;
#5703 = EDGE_LOOP ( 'NONE', ( #28947, #13400, #26881, #34096 ) ) ;
#5704 = DIRECTION ( 'NONE',  ( -1.000000000000000000, 1.798972493605577187E-15, 0.000000000000000000 ) ) ;
#5705 = VERTEX_POINT ( 'NONE', #11558 ) ;
#5706 = DIRECTION ( 'NONE',  ( 0.000000000000000000, 0.000000000000000000, -1.000000000000000000 ) ) ;
#5707 = EDGE_LOOP ( 'NONE', ( #27266, #7839, #4199, #649 ) ) ;
#5708 = CIRCLE ( 'NONE', #24880, 33.00000000000002132 ) ;
#5709 = EDGE_LOOP ( 'NONE', ( #22541, #7241, #33591, #26599 ) ) ;
#5710 = AXIS2_PLACEMENT_3D ( 'NONE', #29491, #23899, #34952 ) ;
#5711 = EDGE_CURVE ( 'NONE', #12879, #25301, #17280, .T. ) ;
#5712 = CYLINDRICAL_SURFACE ( 'NONE', #27964, 5.750000000000002665 ) ;
#5713 = DIRECTION ( 'NONE',  ( 0.000000000000000000, 0.000000000000000000, 1.000000000000000000 ) ) ;
#5714 = ORIENTED_EDGE ( 'NONE', *, *, #28098, .T. ) ;
#5715 = CARTESIAN_POINT ( 'NONE',  ( 69.99999662536838230, -51.96152422706639840, -9.999999999999998224 ) ) ;
#5716 = CONTEXT_DEPENDENT_SHAPE_REPRESENTATION ( #34833, #35552 ) ;
#5717 = EDGE_CURVE ( 'NONE', #35764, #28135, #18490, .T. ) ;
#5718 = CYLINDRICAL_SURFACE ( 'NONE', #6094, 3.500000000000003109 ) ;
#5719 = DIRECTION ( 'NONE',  ( 1.000000000000000000, 0.000000000000000000, 0.000000000000000000 ) ) ;
#5720 = CIRCLE ( 'NONE', #24263, 4.749999999999999112 ) ;
#5721 = ORIENTED_EDGE ( 'NONE', *, *, #36200, .T. ) ;
#5722 = DIRECTION ( 'NONE',  ( 0.000000000000000000, 0.000000000000000000, 1.000000000000000000 ) ) ;
#5723 = FACE_OUTER_BOUND ( 'NONE', #4846, .T. ) ;
#5725 = VERTEX_POINT ( 'NONE', #28638 ) ;
#5724 = EDGE_CURVE ( 'NONE', #30650, #1757, #2317, .T. ) ;
#5726 = CARTESIAN_POINT ( 'NONE',  ( 7.122621931239992550E-13, 68.00000000000000000, 12.49999999999999822 ) ) ;
#5727 = AXIS2_PLACEMENT_3D ( 'NONE', #18039, #14490, #14660 ) ;
#5728 = EDGE_CURVE ( 'NONE', #15109, #9425, #11847, .T. ) ;
#5729 = CARTESIAN_POINT ( 'NONE',  ( -67.00000337463102085, 60.62177826491077326, -9.999999999999998224 ) ) ;
#5730 = CARTESIAN_POINT ( 'NONE',  ( 0.000000000000000000, 0.000000000000000000, 15.00000000000000000 ) ) ;
#5731 = AXIS2_PLACEMENT_3D ( 'NONE', #29063, #14291, #14836 ) ;
#5732 = AXIS2_PLACEMENT_3D ( 'NONE', #32964, #18143, #1648 ) ;
#5733 = DIRECTION ( 'NONE',  ( 0.000000000000000000, 0.000000000000000000, 1.000000000000000000 ) ) ;
#5734 = CIRCLE ( 'NONE', #32668, 4.700000000000000178 ) ;
#5735 = VERTEX_POINT ( 'NONE', #28265 ) ;
#5736 = VECTOR ( 'NONE', #3764, 1000.000000000000000 ) ;
#5737 = EDGE_LOOP ( 'NONE', ( #24273, #27245 ) ) ;
#5738 = CARTESIAN_POINT ( 'NONE',  ( -43.00000337463111322, -77.94228634059960825, -9.999999999999998224 ) ) ;
#5739 = LINE ( 'NONE', #34254, #9803 ) ;
#5740 = CIRCLE ( 'NONE', #23694, 2.000000000000001776 ) ;
#5741 = VERTEX_POINT ( 'NONE', #36713 ) ;
#5742 = ORIENTED_EDGE ( 'NONE', *, *, #21967, .T. ) ;
#5743 = EDGE_CURVE ( 'NONE', #26422, #21946, #1700, .T. ) ;
#5744 = DIRECTION ( 'NONE',  ( -0.000000000000000000, 0.000000000000000000, -1.000000000000000000 ) ) ;
#5745 = DIRECTION ( 'NONE',  ( 0.000000000000000000, 0.000000000000000000, -1.000000000000000000 ) ) ;
#5746 = DIRECTION ( 'NONE',  ( -0.000000000000000000, -0.000000000000000000, 1.000000000000000000 ) ) ;
#5747 = EDGE_LOOP ( 'NONE', ( #10837, #962, #32016, #22866, #12723, #14069, #22623, #4523, #6373, #19311, #17991, #35602, #21785, #11422, #16988, #22383, #26959, #6556, #9313, #7228, #14880, #20971, #18334, #1230 ) ) ;
#5748 = AXIS2_PLACEMENT_3D ( 'NONE', #21644, #1942, #33642 ) ;
#5749 = DIRECTION ( 'NONE',  ( 1.000000000000000000, 0.000000000000000000, 0.000000000000000000 ) ) ;
#5750 = VERTEX_POINT ( 'NONE', #37095 ) ;
#5751 = CARTESIAN_POINT ( 'NONE',  ( 39.99999662536853151, 69.28203230275518365, -9.999999999999998224 ) ) ;
#5752 = EDGE_LOOP ( 'NONE', ( #32441, #3564 ) ) ;
#5753 = FACE_BOUND ( 'NONE', #1815, .T. ) ;
#5754 = VECTOR ( 'NONE', #16148, 1000.000000000000000 ) ;
#5755 = CIRCLE ( 'NONE', #10513, 8.500000000000003553 ) ;
#5756 = B_SPLINE_CURVE_WITH_KNOTS ( 'NONE', 3,
 ( #26743, #3687, #23556, #23752, #505, #14746 ),
 .UNSPECIFIED., .F., .F.,
 ( 4, 2, 4 ),
 ( 0.000000000000000000, 0.001529397995383609786, 0.003058795990767219572 ),
 .UNSPECIFIED. ) ;
#5757 = AXIS2_PLACEMENT_3D ( 'NONE', #34028, #36467, #2893 ) ;
#5758 = AXIS2_PLACEMENT_3D ( 'NONE', #3966, #14010, #13453 ) ;
#5759 = EDGE_CURVE ( 'NONE', #19312, #15209, #485, .T. ) ;
#5760 = DIRECTION ( 'NONE',  ( -1.000000000000000000, 0.000000000000000000, 0.000000000000000000 ) ) ;
#5761 = CARTESIAN_POINT ( 'NONE',  ( -51.13139720814380951, 27.50000000000055422, -5.000000000000000888 ) ) ;
#5762 = ADVANCED_FACE ( 'NONE', ( #30707 ), #22074, .T. ) ;
#5763 = ORIENTED_EDGE ( 'NONE', *, *, #23290, .T. ) ;
#5764 = DIRECTION ( 'NONE',  ( -0.4999999999999919509, 0.8660254037844432595, 0.000000000000000000 ) ) ;
#5765 = AXIS2_PLACEMENT_3D ( 'NONE', #3398, #14834, #11458 ) ;
#5766 = EDGE_CURVE ( 'NONE', #15986, #17720, #21448, .T. ) ;
#5767 = CARTESIAN_POINT ( 'NONE',  ( -75.00000337463099243, -25.98076211353322051, 17.49999999999999645 ) ) ;
#5768 = DIRECTION ( 'NONE',  ( -0.000000000000000000, -0.000000000000000000, 1.000000000000000000 ) ) ;
#5769 = DIRECTION ( 'NONE',  ( 0.000000000000000000, 0.000000000000000000, -1.000000000000000000 ) ) ;
#5770 = VERTEX_POINT ( 'NONE', #10848 ) ;
#5771 = DIRECTION ( 'NONE',  ( 0.000000000000000000, 0.000000000000000000, 1.000000000000000000 ) ) ;
#5772 = EDGE_CURVE ( 'NONE', #36626, #19079, #31030, .T. ) ;
#5773 = DIRECTION ( 'NONE',  ( 0.000000000000000000, 0.000000000000000000, 1.000000000000000000 ) ) ;
#5774 = CARTESIAN_POINT ( 'NONE',  ( -68.00000337463099243, 17.32050807568877460, -5.000000000000000000 ) ) ;
#5775 = ADVANCED_FACE ( 'NONE', ( #5223 ), #25662, .F. ) ;
#5776 = AXIS2_PLACEMENT_3D ( 'NONE', #3471, #3271, #14706 ) ;
#5777 = VERTEX_POINT ( 'NONE', #28440 ) ;
#5778 = ORIENTED_EDGE ( 'NONE', *, *, #21162, .F. ) ;
#5779 = AXIS2_PLACEMENT_3D ( 'NONE', #32423, #20803, #23816 ) ;
#5780 = ORIENTED_EDGE ( 'NONE', *, *, #24013, .F. ) ;
#5781 = AXIS2_PLACEMENT_3D ( 'NONE', #28631, #2410, #2579 ) ;
#5782 = CIRCLE ( 'NONE', #10573, 5.750000000000005329 ) ;
#5783 = AXIS2_PLACEMENT_3D ( 'NONE', #29387, #15133, #6700 ) ;
#5784 = EDGE_CURVE ( 'NONE', #16909, #8594, #2772, .T. ) ;
#5785 = AXIS2_PLACEMENT_3D ( 'NONE', #26478, #12199, #23668 ) ;
#5786 = EDGE_CURVE ( 'NONE', #22308, #30710, #4709, .T. ) ;
#5787 = CARTESIAN_POINT ( 'NONE',  ( 52.99999662536846046, -43.30127018922200222, -9.999999999999998224 ) ) ;
#5788 = CIRCLE ( 'NONE', #15357, 2.000000000000000000 ) ;
#5789 = EDGE_CURVE ( 'NONE', #16751, #22685, #30440, .T. ) ;
#5790 = EDGE_CURVE ( 'NONE', #13632, #5750, #31057, .T. ) ;
#5791 = CARTESIAN_POINT ( 'NONE',  ( -3.352586340487482719, -3.837886065734386065, -0.05822226285685593722 ) ) ;
#5792 = CARTESIAN_POINT ( 'NONE',  ( 105.2115705174360016, -57.76812138680612918, 32.50000000000000000 ) ) ;
#5793 = CYLINDRICAL_SURFACE ( 'NONE', #20702, 2.000000000000001776 ) ;
#5794 = DIRECTION ( 'NONE',  ( -1.000000000000000000, 0.000000000000000000, 0.000000000000000000 ) ) ;
#5795 = DIRECTION ( 'NONE',  ( -0.000000000000000000, -0.000000000000000000, 1.000000000000000000 ) ) ;
#5796 = ORIENTED_EDGE ( 'NONE', *, *, #21761, .T. ) ;
#5797 = AXIS2_PLACEMENT_3D ( 'NONE', #2152, #13594, #28031 ) ;
#5798 = ORIENTED_EDGE ( 'NONE', *, *, #1259, .T. ) ;
#5799 = PLANE ( 'NONE',  #30230 ) ;
#5800 = DIRECTION ( 'NONE',  ( 1.000000000000000000, 0.000000000000000000, 0.000000000000000000 ) ) ;
#5801 = DIRECTION ( 'NONE',  ( 1.000000000000000000, 0.000000000000000000, 0.000000000000000000 ) ) ;
#5802 = CARTESIAN_POINT ( 'NONE',  ( -65.00000337463102085, 43.30127018922198801, 12.50000000000000000 ) ) ;
#5803 = VERTEX_POINT ( 'NONE', #28091 ) ;
#5804 = UNCERTAINTY_MEASURE_WITH_UNIT (LENGTH_MEASURE( 1.000000000000000082E-05 ), #29293, 'distance_accuracy_value', 'NONE');
#5805 = AXIS2_PLACEMENT_3D ( 'NONE', #24004, #7305, #15738 ) ;
#5806 = CARTESIAN_POINT ( 'NONE',  ( 31.27962116909601420, -62.97617850287780072, -4.999999999999997335 ) ) ;
#5807 = ORIENTED_EDGE ( 'NONE', *, *, #13744, .T. ) ;
#5808 = ORIENTED_EDGE ( 'NONE', *, *, #25444, .T. ) ;
#5809 = CARTESIAN_POINT ( 'NONE',  ( -38.00000337463113453, -69.28203230275519786, -9.999999999999998224 ) ) ;
#5810 = EDGE_LOOP ( 'NONE', ( #15299, #27496 ) ) ;
#5812 = CIRCLE ( 'NONE', #15388, 3.499999999999996003 ) ;
#5811 = FILL_AREA_STYLE_COLOUR ( '', #29097 ) ;
#5813 = AXIS2_PLACEMENT_3D ( 'NONE', #29808, #15376, #10302 ) ;
#5814 = DIRECTION ( 'NONE',  ( 1.000000000000000000, 0.000000000000000000, 0.000000000000000000 ) ) ;
#5815 = VECTOR ( 'NONE', #13562, 1000.000000000000000 ) ;
#5816 = DIRECTION ( 'NONE',  ( 0.000000000000000000, 0.000000000000000000, 1.000000000000000000 ) ) ;
#5817 = VERTEX_POINT ( 'NONE', #33721 ) ;
#5818 = EDGE_LOOP ( 'NONE', ( #27589, #29699, #25715, #12969 ) ) ;
#5819 = B_SPLINE_CURVE_WITH_KNOTS ( 'NONE', 3,
 ( #10636, #5390, #16825, #8554, #5194, #24886 ),
 .UNSPECIFIED., .F., .F.,
 ( 4, 2, 4 ),
 ( 0.004308305454211647581, 0.005784651566377423289, 0.007260997678543198997 ),
 .UNSPECIFIED. ) ;
#5820 = ORIENTED_EDGE ( 'NONE', *, *, #1607, .F. ) ;
#5821 = VECTOR ( 'NONE', #15632, 1000.000000000000000 ) ;
#5822 = VERTEX_POINT ( 'NONE', #8023 ) ;
#5823 = ORIENTED_EDGE ( 'NONE', *, *, #27328, .T. ) ;
#5824 = FACE_OUTER_BOUND ( 'NONE', #9459, .T. ) ;
#5826 = AXIS2_PLACEMENT_3D ( 'NONE', #24466, #4581, #35906 ) ;
#5825 = DIRECTION ( 'NONE',  ( 0.000000000000000000, 0.000000000000000000, -1.000000000000000000 ) ) ;
#5827 = DIRECTION ( 'NONE',  ( 0.000000000000000000, 0.000000000000000000, -1.000000000000000000 ) ) ;
#5828 = CARTESIAN_POINT ( 'NONE',  ( -62.00000337463107769, -34.64101615137762025, -9.999999999999998224 ) ) ;
#5829 = ORIENTED_EDGE ( 'NONE', *, *, #3233, .T. ) ;
#5830 = FACE_OUTER_BOUND ( 'NONE', #24686, .T. ) ;
#5831 = CONICAL_SURFACE ( 'NONE', #5214, 2.449999999999998845, 0.9599310885968813656 ) ;
#5832 = CARTESIAN_POINT ( 'NONE',  ( -2.775557561562891351E-14, 19.94802294027085310, 18.49999999999999645 ) ) ;
#5833 = AXIS2_PLACEMENT_3D ( 'NONE', #3487, #26524, #20707 ) ;
#5834 = ADVANCED_FACE ( 'NONE', ( #16660 ), #2416, .F. ) ;
#5835 = CARTESIAN_POINT ( 'NONE',  ( 17.99999662536861678, -69.28203230275519786, -9.999999999999998224 ) ) ;
#5836 = ORIENTED_EDGE ( 'NONE', *, *, #6002, .T. ) ;
#5837 = FACE_OUTER_BOUND ( 'NONE', #11541, .T. ) ;
#5838 = CYLINDRICAL_SURFACE ( 'NONE', #29167, 2.000000000000000000 ) ;
#5839 = AXIS2_PLACEMENT_3D ( 'NONE', #32318, #34779, #6082 ) ;
#5840 = VERTEX_POINT ( 'NONE', #33903 ) ;
#5841 = AXIS2_PLACEMENT_3D ( 'NONE', #6145, #26403, #3333 ) ;
#5842 = ORIENTED_EDGE ( 'NONE', *, *, #22571, .F. ) ;
#5843 = AXIS2_PLACEMENT_3D ( 'NONE', #35349, #34951, #23341 ) ;
#5844 = CARTESIAN_POINT ( 'NONE',  ( 52.39915983220795681, 35.19434990244919703, 12.49999999999999822 ) ) ;
#5845 = DIRECTION ( 'NONE',  ( 1.000000000000000000, 0.000000000000000000, 0.000000000000000000 ) ) ;
#5846 = DIRECTION ( 'NONE',  ( 0.000000000000000000, 0.000000000000000000, 1.000000000000000000 ) ) ;
#5847 = CARTESIAN_POINT ( 'NONE',  ( -79.83584802575171580, -32.64776428033012934, -5.000000000000000000 ) ) ;
#5848 = ORIENTED_EDGE ( 'NONE', *, *, #19549, .T. ) ;
#5849 = ORIENTED_EDGE ( 'NONE', *, *, #21287, .T. ) ;
#5850 = AXIS2_PLACEMENT_3D ( 'NONE', #26201, #6692, #17397 ) ;
#5851 = DIRECTION ( 'NONE',  ( 0.000000000000000000, 0.000000000000000000, 1.000000000000000000 ) ) ;
#5852 = CARTESIAN_POINT ( 'NONE',  ( 41.00000000000000000, 103.4105893997321743, -19.99999999999999645 ) ) ;
#5853 = DIRECTION ( 'NONE',  ( 1.000000000000000000, 0.000000000000000000, 0.000000000000000000 ) ) ;
#5854 = VERTEX_POINT ( 'NONE', #28984 ) ;
#5855 = CIRCLE ( 'NONE', #8268, 1.750000000000015765 ) ;
#5856 = AXIS2_PLACEMENT_3D ( 'NONE', #27758, #7719, #13711 ) ;
#5857 = DIRECTION ( 'NONE',  ( 1.000000000000000000, 0.000000000000000000, 0.000000000000000000 ) ) ;
#5858 = ORIENTED_EDGE ( 'NONE', *, *, #4540, .T. ) ;
#5859 = EDGE_CURVE ( 'NONE', #1125, #22827, #28057, .T. ) ;
#5860 = EDGE_CURVE ( 'NONE', #17303, #6640, #23267, .T. ) ;
#5861 = VECTOR ( 'NONE', #22453, 1000.000000000000000 ) ;
#5862 = EDGE_LOOP ( 'NONE', ( #6667, #36625, #36718, #34464 ) ) ;
#5863 = DIRECTION ( 'NONE',  ( 0.5000000000000009992, 0.8660254037844381525, -0.000000000000000000 ) ) ;
#5864 = CIRCLE ( 'NONE', #10655, 2.000000000000001776 ) ;
#5865 = DIRECTION ( 'NONE',  ( -1.000000000000000000, 0.000000000000000000, 0.000000000000000000 ) ) ;
#5866 = ORIENTED_EDGE ( 'NONE', *, *, #9576, .T. ) ;
#5867 = ORIENTED_EDGE ( 'NONE', *, *, #2139, .F. ) ;
#5868 = DIRECTION ( 'NONE',  ( 0.000000000000000000, 0.000000000000000000, 1.000000000000000000 ) ) ;
#5869 = DIRECTION ( 'NONE',  ( 0.000000000000000000, 0.000000000000000000, 1.000000000000000000 ) ) ;
#5870 = DIRECTION ( 'NONE',  ( 0.000000000000000000, 0.000000000000000000, 1.000000000000000000 ) ) ;
#5871 = AXIS2_PLACEMENT_3D ( 'NONE', #23703, #12057, #3652 ) ;
#5872 = ADVANCED_FACE ( 'NONE', ( #6311 ), #9306, .T. ) ;
#5873 = EDGE_LOOP ( 'NONE', ( #32178, #9799, #26930 ) ) ;
#5874 = DIRECTION ( 'NONE',  ( 0.000000000000000000, 0.000000000000000000, 1.000000000000000000 ) ) ;
#5875 = FACE_BOUND ( 'NONE', #36860, .T. ) ;
#5876 = CARTESIAN_POINT ( 'NONE',  ( -107.2724133595211526, 47.50000000000096634, 27.50000000000000000 ) ) ;
#5877 = DIRECTION ( 'NONE',  ( 0.000000000000000000, 0.000000000000000000, -1.000000000000000000 ) ) ;
#5878 = CIRCLE ( 'NONE', #20241, 2.000000000000001776 ) ;
#5879 = CARTESIAN_POINT ( 'NONE',  ( -12.00000337463128197, 86.60254037844397601, -5.000000000000000000 ) ) ;
#5880 = DIRECTION ( 'NONE',  ( 1.000000000000000000, 0.000000000000000000, 0.000000000000000000 ) ) ;
#5881 = PRODUCT ( 'BR-596', 'BR-596', '', ( #21112 ) ) ;
#5882 = CARTESIAN_POINT ( 'NONE',  ( 9.999996625368625658, 86.60254037844397601, 12.50000000000000000 ) ) ;
#5883 = AXIS2_PLACEMENT_3D ( 'NONE', #16158, #12748, #29835 ) ;
#5884 = EDGE_CURVE ( 'NONE', #9210, #36782, #16695, .T. ) ;
#5885 = DIRECTION ( 'NONE',  ( 0.000000000000000000, 0.000000000000000000, 1.000000000000000000 ) ) ;
#5886 = ORIENTED_EDGE ( 'NONE', *, *, #26187, .T. ) ;
#5887 = DIRECTION ( 'NONE',  ( -0.5000000000000112133, -0.8660254037844322683, 0.000000000000000000 ) ) ;
#5888 = AXIS2_PLACEMENT_3D ( 'NONE', #26721, #24102, #18487 ) ;
#5889 = CIRCLE ( 'NONE', #37045, 95.00000000000001421 ) ;
#5890 = FACE_BOUND ( 'NONE', #29207, .T. ) ;
#5891 = DIRECTION ( 'NONE',  ( 0.000000000000000000, 0.000000000000000000, 1.000000000000000000 ) ) ;
#5892 = VECTOR ( 'NONE', #6515, 999.9999999999998863 ) ;
#5893 = VERTEX_POINT ( 'NONE', #32179 ) ;
#5894 = ORIENTED_EDGE ( 'NONE', *, *, #20040, .T. ) ;
#5895 = VERTEX_POINT ( 'NONE', #35005 ) ;
#5896 = VECTOR ( 'NONE', #34331, 1000.000000000000000 ) ;
#5897 = CARTESIAN_POINT ( 'NONE',  ( 3.000000000000000000, 2.935248768560057453, -3.903127820947815962E-15 ) ) ;
#5898 = CARTESIAN_POINT ( 'NONE',  ( -72.00000337463102085, -34.64101615137762025, 12.50000000000000000 ) ) ;
#5899 = CARTESIAN_POINT ( 'NONE',  ( 5.000000000000000000, 24.49489742783178414, -15.00000000000000000 ) ) ;
#5900 = ORIENTED_EDGE ( 'NONE', *, *, #31535, .F. ) ;
#5901 = AXIS2_PLACEMENT_3D ( 'NONE', #23907, #35359, #9647 ) ;
#5902 = DIRECTION ( 'NONE',  ( 1.000000000000000000, 0.000000000000000000, 0.000000000000000000 ) ) ;
#5903 = EDGE_LOOP ( 'NONE', ( #6803, #33611 ) ) ;
#5904 = ADVANCED_FACE ( 'NONE', ( #31800 ), #692, .T. ) ;
#5905 = FACE_OUTER_BOUND ( 'NONE', #33697, .T. ) ;
#5906 = ORIENTED_EDGE ( 'NONE', *, *, #6463, .F. ) ;
#5907 = DIRECTION ( 'NONE',  ( -1.000000000000000000, -0.000000000000000000, -0.000000000000000000 ) ) ;
#5908 = ORIENTED_EDGE ( 'NONE', *, *, #11943, .T. ) ;
#5909 = EDGE_LOOP ( 'NONE', ( #31566, #32402, #28800, #21060, #7469, #33330, #34789, #158 ) ) ;
#5910 =( LENGTH_UNIT ( ) NAMED_UNIT ( * ) SI_UNIT ( .MILLI., .METRE. ) );
#5911 = DIRECTION ( 'NONE',  ( -1.000000000000000000, 0.000000000000000000, 0.000000000000000000 ) ) ;
#5912 = VECTOR ( 'NONE', #2264, 1000.000000000000000 ) ;
#5913 = DIRECTION ( 'NONE',  ( 1.000000000000000000, 0.000000000000000000, 0.000000000000000000 ) ) ;
#5914 = EDGE_CURVE ( 'NONE', #12313, #8445, #8233, .T. ) ;
#5915 = VERTEX_POINT ( 'NONE', #20741 ) ;
#5916 = FACE_OUTER_BOUND ( 'NONE', #7589, .T. ) ;
#5917 = VECTOR ( 'NONE', #20005, 1000.000000000000000 ) ;
#5918 = AXIS2_PLACEMENT_3D ( 'NONE', #11703, #25805, #465 ) ;
#5919 = DIRECTION ( 'NONE',  ( -0.000000000000000000, -0.000000000000000000, 1.000000000000000000 ) ) ;
#5920 = CARTESIAN_POINT ( 'NONE',  ( -58.00000337463104216, 51.96152422706639129, -9.999999999999998224 ) ) ;
#5921 = EDGE_CURVE ( 'NONE', #28766, #22882, #13010, .T. ) ;
#5922 = AXIS2_PLACEMENT_3D ( 'NONE', #24578, #30358, #24934 ) ;
#5923 = ORIENTED_EDGE ( 'NONE', *, *, #24914, .F. ) ;
#5924 = CARTESIAN_POINT ( 'NONE',  ( -80.00000337463096400, -34.64101615137762025, -5.000000000000000000 ) ) ;
#5925 = CARTESIAN_POINT ( 'NONE',  ( -40.00000337463113453, 69.28203230275516944, -9.999999999999998224 ) ) ;
#5926 = ORIENTED_EDGE ( 'NONE', *, *, #20422, .F. ) ;
#5927 = DIRECTION ( 'NONE',  ( 0.000000000000000000, 0.000000000000000000, 1.000000000000000000 ) ) ;
#5928 = CARTESIAN_POINT ( 'NONE',  ( 0.000000000000000000, 0.000000000000000000, 12.49999999999999822 ) ) ;
#5929 = CARTESIAN_POINT ( 'NONE',  ( -5.236872748402766398, -0.5087250997262755536, -4.057689166958452276 ) ) ;
#5930 = VECTOR ( 'NONE', #13134, 1000.000000000000000 ) ;
#5931 = LINE ( 'NONE', #101, #31403 ) ;
#5932 = VECTOR ( 'NONE', #17846, 1000.000000000000000 ) ;
#5933 = CYLINDRICAL_SURFACE ( 'NONE', #29275, 2.000000000000001776 ) ;
#5934 = ORIENTED_EDGE ( 'NONE', *, *, #29349, .T. ) ;
#5935 = CARTESIAN_POINT ( 'NONE',  ( 0.000000000000000000, 0.000000000000000000, -5.624496230895140947 ) ) ;
#5936 = DIRECTION ( 'NONE',  ( 0.000000000000000000, 0.000000000000000000, 1.000000000000000000 ) ) ;
#5937 = B_SPLINE_CURVE_WITH_KNOTS ( 'NONE', 3,
 ( #27507, #7633, #19626, #18879, #13250, #22075 ),
 .UNSPECIFIED., .F., .F.,
 ( 4, 2, 4 ),
 ( -3.988673288089476442E-06, 0.0002483701411510734502, 0.0005007289555902363692 ),
 .UNSPECIFIED. ) ;
#5938 = ORIENTED_EDGE ( 'NONE', *, *, #29573, .F. ) ;
#5939 = EDGE_CURVE ( 'NONE', #25343, #10270, #33392, .T. ) ;
#5940 = ORIENTED_EDGE ( 'NONE', *, *, #14639, .T. ) ;
#5941 = EDGE_LOOP ( 'NONE', ( #16432, #3338, #5149, #21200 ) ) ;
#5942 = AXIS2_PLACEMENT_3D ( 'NONE', #26003, #690, #125 ) ;
#5943 = CARTESIAN_POINT ( 'NONE',  ( -35.00000337463117717, -77.94228634059963667, -9.999999999999998224 ) ) ;
#5944 = CARTESIAN_POINT ( 'NONE',  ( -85.00000337463092137, -8.660254037844422825, -5.000000000000000000 ) ) ;
#5945 = CYLINDRICAL_SURFACE ( 'NONE', #27832, 2.000000000000001776 ) ;
#5946 = EDGE_CURVE ( 'NONE', #15938, #5488, #20948, .T. ) ;
#5947 = DIRECTION ( 'NONE',  ( 1.000000000000000000, 0.000000000000000000, 0.000000000000000000 ) ) ;
#5948 = ORIENTED_EDGE ( 'NONE', *, *, #15165, .T. ) ;
#5949 = AXIS2_PLACEMENT_3D ( 'NONE', #23133, #34586, #77 ) ;
#5950 = EDGE_CURVE ( 'NONE', #10634, #26137, #3695, .T. ) ;
#5951 = DIRECTION ( 'NONE',  ( 1.000000000000000000, 0.000000000000000000, 0.000000000000000000 ) ) ;
#5952 = VERTEX_POINT ( 'NONE', #867 ) ;
#5953 = FACE_BOUND ( 'NONE', #15367, .T. ) ;
#5954 = CIRCLE ( 'NONE', #8914, 2.000000000000001776 ) ;
#5955 = AXIS2_PLACEMENT_3D ( 'NONE', #10275, #21707, #33137 ) ;
#5956 = DIRECTION ( 'NONE',  ( -0.000000000000000000, 0.000000000000000000, -1.000000000000000000 ) ) ;
#5957 = CARTESIAN_POINT ( 'NONE',  ( -72.00000337463100664, 51.96152422706637708, -9.999999999999998224 ) ) ;
#5958 = CIRCLE ( 'NONE', #4839, 2.000000000000001776 ) ;
#5959 = CARTESIAN_POINT ( 'NONE',  ( 62.99999662536839651, 60.62177826491078747, 17.49999999999999645 ) ) ;
#5960 = CARTESIAN_POINT ( 'NONE',  ( -108.3061974404900241, -19.22934205794863516, 38.50000000000000000 ) ) ;
#5961 = CARTESIAN_POINT ( 'NONE',  ( 3.000000000000000000, -1.467624384280027172, 2.542000000000001592 ) ) ;
#5962 = CIRCLE ( 'NONE', #1162, 27.00000000000001421 ) ;
#5963 = ADVANCED_FACE ( 'NONE', ( #29378 ), #15123, .F. ) ;
#5964 = CIRCLE ( 'NONE', #4763, 3.000000000000004885 ) ;
#5965 = DIRECTION ( 'NONE',  ( 1.000000000000000000, 0.000000000000000000, 0.000000000000000000 ) ) ;
#5966 = CARTESIAN_POINT ( 'NONE',  ( -2.000003374631327713, 86.60254037844397601, 17.49999999999999645 ) ) ;
#5967 = ORIENTED_EDGE ( 'NONE', *, *, #10642, .T. ) ;
#5968 = DIRECTION ( 'NONE',  ( 1.000000000000000000, 0.000000000000000000, 0.000000000000000000 ) ) ;
#5969 = CIRCLE ( 'NONE', #19149, 1.133333333332999571 ) ;
#5970 = CYLINDRICAL_SURFACE ( 'NONE', #29208, 5.750000000000002665 ) ;
#5971 = DIRECTION ( 'NONE',  ( -0.000000000000000000, -0.000000000000000000, 1.000000000000000000 ) ) ;
#5972 = EDGE_LOOP ( 'NONE', ( #25885, #29686 ) ) ;
#5973 = VERTEX_POINT ( 'NONE', #6132 ) ;
#5974 = ORIENTED_EDGE ( 'NONE', *, *, #22035, .F. ) ;
#5975 = AXIS2_PLACEMENT_3D ( 'NONE', #18896, #15710, #30327 ) ;
#5976 = FACE_BOUND ( 'NONE', #1359, .T. ) ;
#5977 = AXIS2_PLACEMENT_3D ( 'NONE', #8755, #5956, #17387 ) ;
#5978 = EDGE_CURVE ( 'NONE', #33338, #9891, #1051, .T. ) ;
#5979 = FACE_OUTER_BOUND ( 'NONE', #28305, .T. ) ;
#5980 = CARTESIAN_POINT ( 'NONE',  ( 56.67878100130369035, -27.78182860042797131, -4.999999999999997335 ) ) ;
#5981 = EDGE_CURVE ( 'NONE', #9506, #7462, #14215, .T. ) ;
#5982 = DIRECTION ( 'NONE',  ( 0.000000000000000000, -0.000000000000000000, -1.000000000000000000 ) ) ;
#5983 = VECTOR ( 'NONE', #35656, 1000.000000000000000 ) ;
#5984 = DIRECTION ( 'NONE',  ( 0.000000000000000000, 0.000000000000000000, 1.000000000000000000 ) ) ;
#5985 = ORIENTED_EDGE ( 'NONE', *, *, #7149, .F. ) ;
#5986 = EDGE_CURVE ( 'NONE', #32159, #24412, #26005, .T. ) ;
#5987 = EDGE_LOOP ( 'NONE', ( #21795, #6589, #2242, #5249 ) ) ;
#5988 = CARTESIAN_POINT ( 'NONE',  ( 36.99999662536855283, -60.62177826491080168, 12.50000000000000000 ) ) ;
#5989 = CIRCLE ( 'NONE', #21383, 2.000000000000001776 ) ;
#5990 = DIRECTION ( 'NONE',  ( 1.000000000000000000, 0.000000000000000000, 0.000000000000000000 ) ) ;
#5991 = DIRECTION ( 'NONE',  ( 0.000000000000000000, 0.000000000000000000, -1.000000000000000000 ) ) ;
#5992 = EDGE_CURVE ( 'NONE', #2172, #1857, #23206, .T. ) ;
#5993 = VERTEX_POINT ( 'NONE', #23397 ) ;
#5994 = CIRCLE ( 'NONE', #27565, 2.541999999999999815 ) ;
#5995 = ADVANCED_FACE ( 'NONE', ( #34828 ), #9122, .F. ) ;
#5996 = FACE_BOUND ( 'NONE', #31581, .T. ) ;
#5997 = EDGE_LOOP ( 'NONE', ( #29635, #26327, #33515, #1906 ) ) ;
#5998 = ORIENTED_EDGE ( 'NONE', *, *, #9096, .T. ) ;
#5999 = CYLINDRICAL_SURFACE ( 'NONE', #880, 1.999999999999998224 ) ;
#6000 = ORIENTED_EDGE ( 'NONE', *, *, #8976, .T. ) ;
#6001 = AXIS2_PLACEMENT_3D ( 'NONE', #9448, #12424, #6248 ) ;
#6002 = EDGE_CURVE ( 'NONE', #22484, #18228, #19024, .T. ) ;
#6003 = EDGE_CURVE ( 'NONE', #17282, #22792, #24400, .T. ) ;
#6004 = CARTESIAN_POINT ( 'NONE',  ( 69.99999662536838230, -34.64101615137759183, -9.999999999999998224 ) ) ;
#6005 = EDGE_CURVE ( 'NONE', #24584, #28819, #10250, .T. ) ;
#6006 = CARTESIAN_POINT ( 'NONE',  ( 72.99999662536836809, 25.98076211353319565, 17.49999999999999645 ) ) ;
#6007 = EDGE_CURVE ( 'NONE', #21544, #5447, #31578, .T. ) ;
#6008 = ORIENTED_EDGE ( 'NONE', *, *, #15783, .F. ) ;
#6009 = ADVANCED_FACE ( 'NONE', ( #10070 ), #19073, .F. ) ;
#6010 = ORIENTED_EDGE ( 'NONE', *, *, #24301, .F. ) ;
#6011 = ORIENTED_EDGE ( 'NONE', *, *, #7220, .F. ) ;
#6012 = ORIENTED_EDGE ( 'NONE', *, *, #2758, .F. ) ;
#6013 = VERTEX_POINT ( 'NONE', #21861 ) ;
#6014 = CYLINDRICAL_SURFACE ( 'NONE', #33201, 27.00000000000001066 ) ;
#6015 = CIRCLE ( 'NONE', #20796, 2.000000000000001776 ) ;
#6016 = CARTESIAN_POINT ( 'NONE',  ( -4.279621169095561228, 62.97617850287782915, 12.49999999999999822 ) ) ;
#6017 = DIRECTION ( 'NONE',  ( -1.000000000000000000, 0.000000000000000000, 0.000000000000000000 ) ) ;
#6018 = CARTESIAN_POINT ( 'NONE',  ( 4.654160418576254177E-15, -6.066067634115602125, -4.359491423763670603 ) ) ;
#6019 = DIRECTION ( 'NONE',  ( 1.000000000000000000, 0.000000000000000000, 0.000000000000000000 ) ) ;
#6020 = ORIENTED_EDGE ( 'NONE', *, *, #23180, .F. ) ;
#6021 = CARTESIAN_POINT ( 'NONE',  ( -72.00000337463100664, 51.96152422706637708, -9.999999999999998224 ) ) ;
#6022 = CARTESIAN_POINT ( 'NONE',  ( -3.500188911486801224, -4.028306647601615609, -4.085926550512745337 ) ) ;
#6023 = DIRECTION ( 'NONE',  ( 1.000000000000000000, 0.000000000000000000, 0.000000000000000000 ) ) ;
#6024 = ORIENTED_EDGE ( 'NONE', *, *, #34641, .F. ) ;
#6025 = AXIS2_PLACEMENT_3D ( 'NONE', #28458, #22125, #5431 ) ;
#6026 = LINE ( 'NONE', #12158, #33436 ) ;
#6027 = CYLINDRICAL_SURFACE ( 'NONE', #11781, 2.000000000000001776 ) ;
#6028 = ORIENTED_EDGE ( 'NONE', *, *, #36005, .T. ) ;
#6029 = EDGE_LOOP ( 'NONE', ( #28725, #3437 ) ) ;
#6030 = DIRECTION ( 'NONE',  ( 1.000000000000000000, 0.000000000000000000, 0.000000000000000000 ) ) ;
#6031 = CARTESIAN_POINT ( 'NONE',  ( 41.99999662536853151, 69.28203230275518365, -9.999999999999998224 ) ) ;
#6032 = AXIS2_PLACEMENT_3D ( 'NONE', #30764, #22717, #16346 ) ;
#6033 = DIRECTION ( 'NONE',  ( -1.000000000000000000, 0.000000000000000000, 0.000000000000000000 ) ) ;
#6034 = FACE_OUTER_BOUND ( 'NONE', #17888, .T. ) ;
#6035 = ORIENTED_EDGE ( 'NONE', *, *, #27011, .F. ) ;
#6036 = DIRECTION ( 'NONE',  ( 1.000000000000000000, 0.000000000000000000, 0.000000000000000000 ) ) ;
#6037 = DIRECTION ( 'NONE',  ( 0.000000000000000000, 0.000000000000000000, 1.000000000000000000 ) ) ;
#6038 = FACE_OUTER_BOUND ( 'NONE', #26405, .T. ) ;
#6039 = ORIENTED_EDGE ( 'NONE', *, *, #22238, .F. ) ;
#6040 = DIRECTION ( 'NONE',  ( 0.000000000000000000, 0.000000000000000000, -1.000000000000000000 ) ) ;
#6041 = EDGE_LOOP ( 'NONE', ( #33797, #13649 ) ) ;
#6042 = VERTEX_POINT ( 'NONE', #32942 ) ;
#6043 = EDGE_CURVE ( 'NONE', #23996, #3218, #4054, .T. ) ;
#6044 = DIRECTION ( 'NONE',  ( 1.000000000000000000, 0.000000000000000000, 0.000000000000000000 ) ) ;
#6045 = CARTESIAN_POINT ( 'NONE',  ( -5.000003374631269537, -77.94228634059960825, 17.49999999999999645 ) ) ;
#6046 = EDGE_CURVE ( 'NONE', #6156, #14042, #18872, .T. ) ;
#6047 = ORIENTED_EDGE ( 'NONE', *, *, #21822, .F. ) ;
#6048 = ORIENTED_EDGE ( 'NONE', *, *, #13867, .T. ) ;
#6049 = CARTESIAN_POINT ( 'NONE',  ( 52.39915983220795681, 35.19434990244919703, -4.999999999999997335 ) ) ;
#6050 = DIRECTION ( 'NONE',  ( 0.000000000000000000, 0.000000000000000000, 1.000000000000000000 ) ) ;
#6051 = CYLINDRICAL_SURFACE ( 'NONE', #9509, 2.000000000000001776 ) ;
#6052 = VERTEX_POINT ( 'NONE', #1617 ) ;
#6053 = DIRECTION ( 'NONE',  ( 1.000000000000000000, 0.000000000000000000, 0.000000000000000000 ) ) ;
#6054 = FACE_BOUND ( 'NONE', #14891, .T. ) ;
#6055 = CARTESIAN_POINT ( 'NONE',  ( 19.99999662536858835, 69.28203230275516944, 12.50000000000000000 ) ) ;
#6056 = FACE_OUTER_BOUND ( 'NONE', #32004, .T. ) ;
#6057 = CARTESIAN_POINT ( 'NONE',  ( 5.000000000000000888, 0.000000000000000000, -6.000000000000000000 ) ) ;
#6058 = CARTESIAN_POINT ( 'NONE',  ( 45.00000000000000711, 0.000000000000000000, -5.000000000000000000 ) ) ;
#6059 = CARTESIAN_POINT ( 'NONE',  ( 69.99999662536839651, 17.32050807568879236, -9.999999999999998224 ) ) ;
#6060 = CARTESIAN_POINT ( 'NONE',  ( 5.000000000000000000, 1.924500897298748958, -3.818275046351161883 ) ) ;
#6061 = VERTEX_POINT ( 'NONE', #4822 ) ;
#6062 = CARTESIAN_POINT ( 'NONE',  ( -72.72667006428976322, 101.6652913307188868, 32.50002500000000083 ) ) ;
#6063 = CARTESIAN_POINT ( 'NONE',  ( -2.448772250512182280E-15, 99.94802294027086020, 18.49999999999999645 ) ) ;
#6064 = DIRECTION ( 'NONE',  ( 1.000000000000000000, 0.000000000000000000, 0.000000000000000000 ) ) ;
#6065 = ADVANCED_FACE ( 'NONE', ( #35575 ), #15509, .T. ) ;
#6066 = ORIENTED_EDGE ( 'NONE', *, *, #3708, .T. ) ;
#6067 = ORIENTED_EDGE ( 'NONE', *, *, #34041, .F. ) ;
#6068 = ORIENTED_EDGE ( 'NONE', *, *, #12726, .F. ) ;
#6069 = CARTESIAN_POINT ( 'NONE',  ( 19.99999662536861678, -69.28203230275519786, -9.999999999999998224 ) ) ;
#6070 = DIRECTION ( 'NONE',  ( 0.000000000000000000, 0.000000000000000000, 1.000000000000000000 ) ) ;
#6071 = DIRECTION ( 'NONE',  ( 0.000000000000000000, 0.000000000000000000, 1.000000000000000000 ) ) ;
#6072 = ORIENTED_EDGE ( 'NONE', *, *, #22021, .F. ) ;
#6073 = VECTOR ( 'NONE', #25857, 1000.000000000000000 ) ;
#6074 = EDGE_CURVE ( 'NONE', #20247, #33988, #23805, .T. ) ;
#6075 = DIRECTION ( 'NONE',  ( 0.000000000000000000, 0.000000000000000000, 1.000000000000000000 ) ) ;
#6076 = EDGE_LOOP ( 'NONE', ( #14437, #8293, #14825, #8058 ) ) ;
#6077 = DIRECTION ( 'NONE',  ( -1.000000000000000000, 0.000000000000000000, 0.000000000000000000 ) ) ;
#6078 = ORIENTED_EDGE ( 'NONE', *, *, #30736, .F. ) ;
#6079 = CARTESIAN_POINT ( 'NONE',  ( -3.000003374631308173, 77.94228634059957983, -5.000000000000000000 ) ) ;
#6080 = ORIENTED_EDGE ( 'NONE', *, *, #23134, .F. ) ;
#6081 = ORIENTED_EDGE ( 'NONE', *, *, #16288, .F. ) ;
#6082 = DIRECTION ( 'NONE',  ( 1.000000000000000000, 0.000000000000000000, 0.000000000000000000 ) ) ;
#6083 = CARTESIAN_POINT ( 'NONE',  ( 2.018853055115724882, -4.607917337070903230, -0.5666985376598668855 ) ) ;
#6084 = FACE_OUTER_BOUND ( 'NONE', #19992, .T. ) ;
#6085 = EDGE_CURVE ( 'NONE', #34784, #9159, #2857, .T. ) ;
#6086 =( REPRESENTATION_RELATIONSHIP ('NONE','NONE', #15268, #35440 ) REPRESENTATION_RELATIONSHIP_WITH_TRANSFORMATION ( #10062 )SHAPE_REPRESENTATION_RELATIONSHIP( ) );
#6087 = ORIENTED_EDGE ( 'NONE', *, *, #18561, .T. ) ;
#6088 = CARTESIAN_POINT ( 'NONE',  ( 56.99999662536846046, -43.30127018922200222, -9.999999999999998224 ) ) ;
#6089 = CARTESIAN_POINT ( 'NONE',  ( 3.499999999999991562, -55.00000000000000000, -10.00000000000000000 ) ) ;
#6090 = CARTESIAN_POINT ( 'NONE',  ( -65.00000337463106348, -60.62177826491083010, 12.50000000000000000 ) ) ;
#6091 = ORIENTED_EDGE ( 'NONE', *, *, #3763, .T. ) ;
#6092 = CARTESIAN_POINT ( 'NONE',  ( -65.00000000000000000, 0.000000000000000000, 5.000000000000000000 ) ) ;
#6093 = PLANE ( 'NONE',  #594 ) ;
#6094 = AXIS2_PLACEMENT_3D ( 'NONE', #28589, #3468, #2923 ) ;
#6095 = ORIENTED_EDGE ( 'NONE', *, *, #35889, .F. ) ;
#6096 = CARTESIAN_POINT ( 'NONE',  ( -60.00000337463107059, -34.64101615137762025, -9.999999999999998224 ) ) ;
#6097 = CIRCLE ( 'NONE', #30042, 2.000000000000001776 ) ;
#6098 = CARTESIAN_POINT ( 'NONE',  ( 69.99999662536839651, -3.469446951953614189E-15, -5.000000000000000000 ) ) ;
#6099 = CARTESIAN_POINT ( 'NONE',  ( 34.99999662536855283, 60.62177826491078747, -9.999999999999998224 ) ) ;
#6100 = DIRECTION ( 'NONE',  ( 1.000000000000000000, 0.000000000000000000, 0.000000000000000000 ) ) ;
#6101 = DIRECTION ( 'NONE',  ( -0.4999999999999980016, 0.8660254037844398178, 0.000000000000000000 ) ) ;
#6102 = EDGE_CURVE ( 'NONE', #3063, #34990, #16025, .T. ) ;
#6103 = ORIENTED_EDGE ( 'NONE', *, *, #18304, .F. ) ;
#6104 = CARTESIAN_POINT ( 'NONE',  ( 5.253368672218635460, 3.033033817057773529, -4.359491423763652840 ) ) ;
#6105 = LINE ( 'NONE', #34802, #8017 ) ;
#6106 = EDGE_CURVE ( 'NONE', #859, #30760, #27975, .T. ) ;
#6107 = ORIENTED_EDGE ( 'NONE', *, *, #8478, .F. ) ;
#6108 = ORIENTED_EDGE ( 'NONE', *, *, #12609, .T. ) ;
#6109 = ORIENTED_EDGE ( 'NONE', *, *, #30397, .T. ) ;
#6110 = CYLINDRICAL_SURFACE ( 'NONE', #27798, 2.000000000000001776 ) ;
#6111 = DIRECTION ( 'NONE',  ( 1.000000000000000000, 0.000000000000000000, 0.000000000000000000 ) ) ;
#6112 = EDGE_CURVE ( 'NONE', #27114, #21710, #12853, .T. ) ;
#6113 = CARTESIAN_POINT ( 'NONE',  ( -7.000003374631307729, 77.94228634059957983, 17.49999999999999645 ) ) ;
#6114 = ADVANCED_FACE ( 'NONE', ( #18691 ), #6866, .F. ) ;
#6115 = DIRECTION ( 'NONE',  ( 1.000000000000000000, 0.000000000000000000, 0.000000000000000000 ) ) ;
#6116 = EDGE_LOOP ( 'NONE', ( #25095, #2446, #23430, #26963 ) ) ;
#6117 = CARTESIAN_POINT ( 'NONE',  ( 61.99999662536842493, 51.96152422706639129, -9.999999999999998224 ) ) ;
#6118 = EDGE_LOOP ( 'NONE', ( #12284, #226, #36419, #19895 ) ) ;
#6119 = FACE_BOUND ( 'NONE', #35341, .T. ) ;
#6120 = CYLINDRICAL_SURFACE ( 'NONE', #3542, 2.000000000000000000 ) ;
#6121 = DIRECTION ( 'NONE',  ( 1.000000000000000000, 0.000000000000000000, 0.000000000000000000 ) ) ;
#6122 = EDGE_CURVE ( 'NONE', #22882, #32886, #7642, .T. ) ;
#6123 = DIRECTION ( 'NONE',  ( 0.000000000000000000, 0.000000000000000000, 1.000000000000000000 ) ) ;
#6124 = SHAPE_DEFINITION_REPRESENTATION ( #5269, #15268 ) ;
#6125 = CARTESIAN_POINT ( 'NONE',  ( -3.374631303565411855E-06, -86.60254037844400443, -5.000000000000000000 ) ) ;
#6126 = VECTOR ( 'NONE', #21950, 1000.000000000000000 ) ;
#6127 = EDGE_CURVE ( 'NONE', #23686, #6764, #8835, .T. ) ;
#6128 = AXIS2_PLACEMENT_3D ( 'NONE', #11081, #13729, #22731 ) ;
#6129 = FACE_OUTER_BOUND ( 'NONE', #36974, .T. ) ;
#6130 = DIRECTION ( 'NONE',  ( 0.000000000000000000, 0.000000000000000000, -1.000000000000000000 ) ) ;
#6131 = ORIENTED_EDGE ( 'NONE', *, *, #16412, .F. ) ;
#6132 = CARTESIAN_POINT ( 'NONE',  ( -104.8061974404896262, 19.22934205795090534, 27.50000000000000000 ) ) ;
#6133 = PLANE ( 'NONE',  #19646 ) ;
#6134 = DIRECTION ( 'NONE',  ( 0.000000000000000000, 0.000000000000000000, -1.000000000000000000 ) ) ;
#6135 = EDGE_CURVE ( 'NONE', #1757, #30650, #11787, .T. ) ;
#6136 = ORIENTED_EDGE ( 'NONE', *, *, #32051, .T. ) ;
#6137 = EDGE_LOOP ( 'NONE', ( #20883, #11085, #4785 ) ) ;
#6138 = AXIS2_PLACEMENT_3D ( 'NONE', #4690, #24569, #10676 ) ;
#6139 = EDGE_CURVE ( 'NONE', #24840, #32261, #32163, .T. ) ;
#6140 = EDGE_LOOP ( 'NONE', ( #29870, #32473, #22904, #36445 ) ) ;
#6141 = LINE ( 'NONE', #28993, #13533 ) ;
#6142 = FACE_BOUND ( 'NONE', #10988, .T. ) ;
#6143 = DIRECTION ( 'NONE',  ( -1.000000000000000000, 1.632680918566405215E-15, 0.000000000000000000 ) ) ;
#6144 = DIRECTION ( 'NONE',  ( -1.000000000000000000, 0.000000000000000000, -0.000000000000000000 ) ) ;
#6145 = CARTESIAN_POINT ( 'NONE',  ( -50.00000337463112032, -51.96152422706641971, -9.999999999999998224 ) ) ;
#6146 = DIRECTION ( 'NONE',  ( 1.000000000000000000, 0.000000000000000000, 0.000000000000000000 ) ) ;
#6147 = ORIENTED_EDGE ( 'NONE', *, *, #23889, .F. ) ;
#6148 = VERTEX_POINT ( 'NONE', #32743 ) ;
#6149 = AXIS2_PLACEMENT_3D ( 'NONE', #28710, #11997, #32253 ) ;
#6150 = DIRECTION ( 'NONE',  ( -0.000000000000000000, -0.000000000000000000, 1.000000000000000000 ) ) ;
#6151 = EDGE_CURVE ( 'NONE', #16958, #30923, #25075, .T. ) ;
#6152 = CARTESIAN_POINT ( 'NONE',  ( 93.36492675454790913, 17.14523346298246409, -4.999999999999997335 ) ) ;
#6153 = CARTESIAN_POINT ( 'NONE',  ( 44.99999662536849598, 60.62177826491077326, -9.999999999999998224 ) ) ;
#6154 = ORIENTED_EDGE ( 'NONE', *, *, #23477, .T. ) ;
#6155 = FACE_BOUND ( 'NONE', #33250, .T. ) ;
#6156 = VERTEX_POINT ( 'NONE', #19974 ) ;
#6157 = VECTOR ( 'NONE', #12640, 1000.000000000000000 ) ;
#6158 = ORIENTED_EDGE ( 'NONE', *, *, #15111, .F. ) ;
#6159 = CIRCLE ( 'NONE', #31291, 2.000000000000001776 ) ;
#6160 = DIRECTION ( 'NONE',  ( 1.000000000000000000, 0.000000000000000000, 0.000000000000000000 ) ) ;
#6161 = VERTEX_POINT ( 'NONE', #10972 ) ;
#6162 = CYLINDRICAL_SURFACE ( 'NONE', #13428, 2.000000000000001776 ) ;
#6163 = ADVANCED_FACE ( 'NONE', ( #36851 ), #7817, .F. ) ;
#6164 = LINE ( 'NONE', #8803, #20855 ) ;
#6165 = ORIENTED_EDGE ( 'NONE', *, *, #19629, .F. ) ;
#6166 = ORIENTED_EDGE ( 'NONE', *, *, #13322, .T. ) ;
#6167 = AXIS2_PLACEMENT_3D ( 'NONE', #17138, #6070, #17674 ) ;
#6168 = EDGE_LOOP ( 'NONE', ( #11472, #8715 ) ) ;
#6169 = ADVANCED_FACE ( 'NONE', ( #10809 ), #5545, .F. ) ;
#6170 = ORIENTED_EDGE ( 'NONE', *, *, #4522, .F. ) ;
#6171 = AXIS2_PLACEMENT_3D ( 'NONE', #9711, #32574, #24536 ) ;
#6172 = ORIENTED_EDGE ( 'NONE', *, *, #13744, .F. ) ;
#6173 = DIRECTION ( 'NONE',  ( 1.000000000000000000, 0.000000000000000000, 0.000000000000000000 ) ) ;
#6174 = EDGE_CURVE ( 'NONE', #34827, #8340, #29755, .T. ) ;
#6175 = CYLINDRICAL_SURFACE ( 'NONE', #621, 2.000000000000000000 ) ;
#6176 = ADVANCED_FACE ( 'NONE', ( #36508 ), #28399, .F. ) ;
#6177 = CARTESIAN_POINT ( 'NONE',  ( 44.99999662536851019, -60.62177826491080168, -5.000000000000000000 ) ) ;
#6178 = CARTESIAN_POINT ( 'NONE',  ( 84.91058168688746832, 72.42202624339670081, 32.50000000000000711 ) ) ;
#6179 = LINE ( 'NONE', #8815, #21940 ) ;
#6180 = ORIENTED_EDGE ( 'NONE', *, *, #9579, .T. ) ;
#6181 = CYLINDRICAL_SURFACE ( 'NONE', #4491, 2.000000000000001776 ) ;
#6182 = CARTESIAN_POINT ( 'NONE',  ( 12.99999662536859901, 77.94228634059957983, -9.999999999999998224 ) ) ;
#6183 = CIRCLE ( 'NONE', #18777, 1.999999999999998224 ) ;
#6184 = LINE ( 'NONE', #3747, #11028 ) ;
#6185 = ORIENTED_EDGE ( 'NONE', *, *, #28124, .F. ) ;
#6186 = CARTESIAN_POINT ( 'NONE',  ( -63.00000337463102085, 25.98076211353317433, -9.999999999999998224 ) ) ;
#6187 = FACE_OUTER_BOUND ( 'NONE', #26077, .T. ) ;
#6188 = EDGE_CURVE ( 'NONE', #22417, #16140, #26184, .T. ) ;
#6189 = ORIENTED_EDGE ( 'NONE', *, *, #20369, .F. ) ;
#6190 = EDGE_LOOP ( 'NONE', ( #3055, #17204, #19916, #17862 ) ) ;
#6191 = DIRECTION ( 'NONE',  ( 0.000000000000000000, 0.000000000000000000, 1.000000000000000000 ) ) ;
#6192 = EDGE_CURVE ( 'NONE', #35130, #28991, #10019, .T. ) ;
#6193 = CARTESIAN_POINT ( 'NONE',  ( -73.00000337463097821, -8.660254037844422825, -9.999999999999998224 ) ) ;
#6194 = CARTESIAN_POINT ( 'NONE',  ( -50.00000337463110611, -69.28203230275519786, -5.000000000000000000 ) ) ;
#6195 = DIRECTION ( 'NONE',  ( 0.000000000000000000, 0.000000000000000000, 1.000000000000000000 ) ) ;
#6196 = ORIENTED_EDGE ( 'NONE', *, *, #34736, .F. ) ;
#6197 = CIRCLE ( 'NONE', #33755, 2.000000000000000000 ) ;
#6198 = B_SPLINE_CURVE_WITH_KNOTS ( 'NONE', 3,
 ( #36143, #7646, #19099, #35975, #18709, #13431, #10645, #30525 ),
 .UNSPECIFIED., .F., .F.,
 ( 4, 2, 2, 4 ),
 ( 0.007260997678543198997, 0.007995810154593248689, 0.008730622630643298382, 0.01020024758274339603 ),
 .UNSPECIFIED. ) ;
#6199 = CARTESIAN_POINT ( 'NONE',  ( 19.99999662536861678, -86.60254037844400443, -9.999999999999998224 ) ) ;
#6200 = FACE_BOUND ( 'NONE', #23600, .T. ) ;
#6201 = DIRECTION ( 'NONE',  ( -0.000000000000000000, -0.000000000000000000, 1.000000000000000000 ) ) ;
#6202 = AXIS2_PLACEMENT_3D ( 'NONE', #9883, #1438, #26954 ) ;
#6203 = ORIENTED_EDGE ( 'NONE', *, *, #13322, .F. ) ;
#6204 = DIRECTION ( 'NONE',  ( 1.000000000000000000, 0.000000000000000000, 0.000000000000000000 ) ) ;
#6205 = ORIENTED_EDGE ( 'NONE', *, *, #33798, .T. ) ;
#6206 = DIRECTION ( 'NONE',  ( 0.000000000000000000, 0.000000000000000000, -1.000000000000000000 ) ) ;
#6207 = CIRCLE ( 'NONE', #23581, 2.000000000000001776 ) ;
#6208 = DIRECTION ( 'NONE',  ( 0.000000000000000000, 0.000000000000000000, 1.000000000000000000 ) ) ;
#6209 = EDGE_CURVE ( 'NONE', #14593, #22384, #11819, .T. ) ;
#6210 = CARTESIAN_POINT ( 'NONE',  ( -33.00000337463117006, -77.94228634059963667, -9.999999999999998224 ) ) ;
#6211 = ORIENTED_EDGE ( 'NONE', *, *, #826, .T. ) ;
#6212 = EDGE_CURVE ( 'NONE', #19957, #18483, #10052, .T. ) ;
#6213 = ORIENTED_EDGE ( 'NONE', *, *, #24053, .F. ) ;
#6214 = CARTESIAN_POINT ( 'NONE',  ( 61.25926521283102488, -32.16008401677932227, 12.49999999999999645 ) ) ;
#6215 = CARTESIAN_POINT ( 'NONE',  ( -77.93337901593650940, -72.12093275448718543, 32.50001250000000397 ) ) ;
#6216 = LINE ( 'NONE', #17648, #15504 ) ;
#6217 = VERTEX_POINT ( 'NONE', #25416 ) ;
#6218 = CARTESIAN_POINT ( 'NONE',  ( 74.99999662536836809, 25.98076211353319565, -9.999999999999998224 ) ) ;
#6219 = FACE_BOUND ( 'NONE', #9271, .T. ) ;
#6220 = EDGE_CURVE ( 'NONE', #24561, #18446, #36310, .T. ) ;
#6221 = CARTESIAN_POINT ( 'NONE',  ( -57.00000337463111322, -43.30127018922202353, -9.999999999999998224 ) ) ;
#6222 = CARTESIAN_POINT ( 'NONE',  ( 2.499999999999998224, 4.330127018922196314, -3.620524600599877019 ) ) ;
#6223 = CARTESIAN_POINT ( 'NONE',  ( -55.00000337463107059, 43.30127018922197379, -9.999999999999998224 ) ) ;
#6224 = DIRECTION ( 'NONE',  ( 0.000000000000000000, 0.000000000000000000, 1.000000000000000000 ) ) ;
#6225 = AXIS2_PLACEMENT_3D ( 'NONE', #4410, #3840, #29708 ) ;
#6226 = CARTESIAN_POINT ( 'NONE',  ( -63.00000337463104927, -25.98076211353322051, 12.50000000000000000 ) ) ;
#6227 = FACE_OUTER_BOUND ( 'NONE', #25491, .T. ) ;
#6228 = VERTEX_POINT ( 'NONE', #34061 ) ;
#6229 = FACE_OUTER_BOUND ( 'NONE', #10448, .T. ) ;
#6230 = FACE_BOUND ( 'NONE', #34854, .T. ) ;
#6231 = FACE_OUTER_BOUND ( 'NONE', #16994, .T. ) ;
#6232 = EDGE_CURVE ( 'NONE', #36096, #13826, #31003, .T. ) ;
#6233 = AXIS2_PLACEMENT_3D ( 'NONE', #11250, #3006, #5814 ) ;
#6234 = VERTEX_POINT ( 'NONE', #22067 ) ;
#6235 = ADVANCED_FACE ( 'NONE', ( #19252 ), #30667, .F. ) ;
#6236 = ORIENTED_EDGE ( 'NONE', *, *, #10351, .T. ) ;
#6237 = ORIENTED_EDGE ( 'NONE', *, *, #36344, .T. ) ;
#6238 = EDGE_CURVE ( 'NONE', #36749, #4152, #5878, .T. ) ;
#6239 = AXIS2_PLACEMENT_3D ( 'NONE', #26062, #11804, #32429 ) ;
#6240 = EDGE_CURVE ( 'NONE', #32504, #36248, #4986, .T. ) ;
#6241 = CARTESIAN_POINT ( 'NONE',  ( -65.00000337463102085, 43.30127018922198801, -5.000000000000000000 ) ) ;
#6242 = CARTESIAN_POINT ( 'NONE',  ( -45.00000337463112743, -60.62177826491080168, -5.000000000000000000 ) ) ;
#6243 = DIRECTION ( 'NONE',  ( 0.000000000000000000, 0.000000000000000000, 1.000000000000000000 ) ) ;
#6244 = VERTEX_POINT ( 'NONE', #27844 ) ;
#6245 = ORIENTED_EDGE ( 'NONE', *, *, #8716, .F. ) ;
#6246 = CARTESIAN_POINT ( 'NONE',  ( 59.13646009116148150, -70.47608876694609137, -4.999999999999997335 ) ) ;
#6247 = VERTEX_POINT ( 'NONE', #25616 ) ;
#6248 = DIRECTION ( 'NONE',  ( 1.000000000000000000, 0.000000000000000000, 0.000000000000000000 ) ) ;
#6249 = CIRCLE ( 'NONE', #24209, 2.000000000000001776 ) ;
#6250 = ORIENTED_EDGE ( 'NONE', *, *, #15320, .T. ) ;
#6251 = CYLINDRICAL_SURFACE ( 'NONE', #21334, 3.000000000000005773 ) ;
#6252 = VERTEX_POINT ( 'NONE', #22808 ) ;
#6253 = VERTEX_POINT ( 'NONE', #8543 ) ;
#6254 = VECTOR ( 'NONE', #23830, 1000.000000000000000 ) ;
#6255 = DIRECTION ( 'NONE',  ( 1.000000000000000000, 0.000000000000000000, 0.000000000000000000 ) ) ;
#6256 = CARTESIAN_POINT ( 'NONE',  ( 0.3487148583350060949, -5.572172074566128508, -1.686035282245279765 ) ) ;
#6257 = DIRECTION ( 'NONE',  ( 0.000000000000000000, 0.000000000000000000, -1.000000000000000000 ) ) ;
#6258 = ORIENTED_EDGE ( 'NONE', *, *, #31855, .F. ) ;
#6259 = FACE_OUTER_BOUND ( 'NONE', #28318, .T. ) ;
#6260 = EDGE_CURVE ( 'NONE', #35608, #35112, #7054, .T. ) ;
#6261 = AXIS2_PLACEMENT_3D ( 'NONE', #30337, #30145, #13273 ) ;
#6262 = CARTESIAN_POINT ( 'NONE',  ( -68.00000337463100664, -17.32050807568882078, 12.50000000000000000 ) ) ;
#6263 = CIRCLE ( 'NONE', #8647, 95.00000000000001421 ) ;
#6264 = DIRECTION ( 'NONE',  ( 0.000000000000000000, 0.000000000000000000, 1.000000000000000000 ) ) ;
#6265 = ORIENTED_EDGE ( 'NONE', *, *, #12344, .T. ) ;
#6266 = CIRCLE ( 'NONE', #27216, 2.000000000000001776 ) ;
#6267 = CYLINDRICAL_SURFACE ( 'NONE', #2153, 1.999999999999998224 ) ;
#6268 = DIRECTION ( 'NONE',  ( 1.000000000000000000, 0.000000000000000000, 0.000000000000000000 ) ) ;
#6269 = VERTEX_POINT ( 'NONE', #16615 ) ;
#6270 = CARTESIAN_POINT ( 'NONE',  ( -58.88972745734203329, -33.99999999999965894, -49.86561046011506448 ) ) ;
#6271 = DIRECTION ( 'NONE',  ( 1.000000000000000000, 0.000000000000000000, 0.000000000000000000 ) ) ;
#6272 = FACE_OUTER_BOUND ( 'NONE', #31179, .T. ) ;
#6273 = CARTESIAN_POINT ( 'NONE',  ( -6.069707180676227632E-15, 5.773502691896268857, -3.984345921091771547 ) ) ;
#6274 = DIRECTION ( 'NONE',  ( 0.000000000000000000, 0.000000000000000000, 1.000000000000000000 ) ) ;
#6275 = AXIS2_PLACEMENT_3D ( 'NONE', #31794, #25998, #17390 ) ;
#6276 = CARTESIAN_POINT ( 'NONE',  ( -63.00000337463102085, 25.98076211353317433, -9.999999999999998224 ) ) ;
#6277 = EDGE_LOOP ( 'NONE', ( #17235, #4884, #33763, #23087 ) ) ;
#6279 = AXIS2_PLACEMENT_3D ( 'NONE', #29148, #14912, #26350 ) ;
#6278 = CARTESIAN_POINT ( 'NONE',  ( 95.00000000000001421, 0.000000000000000000, -5.000000000000000000 ) ) ;
#6280 = DIRECTION ( 'NONE',  ( 0.000000000000000000, 0.000000000000000000, 1.000000000000000000 ) ) ;
#6281 = CARTESIAN_POINT ( 'NONE',  ( -80.00000337463094979, -2.428612866367529932E-14, -9.999999999999998224 ) ) ;
#6282 = VERTEX_POINT ( 'NONE', #28047 ) ;
#6283 = CIRCLE ( 'NONE', #8692, 150.0000000000000284 ) ;
#6284 = ORIENTED_EDGE ( 'NONE', *, *, #31945, .F. ) ;
#6285 = ORIENTED_EDGE ( 'NONE', *, *, #11000, .T. ) ;
#6286 = ADVANCED_FACE ( 'NONE', ( #25968 ), #2931, .F. ) ;
#6287 = CYLINDRICAL_SURFACE ( 'NONE', #36192, 2.000000000000001776 ) ;
#6288 = CARTESIAN_POINT ( 'NONE',  ( 2.449999999999998845, 0.000000000000000000, -0.3851141460153411078 ) ) ;
#6289 = DIRECTION ( 'NONE',  ( 0.000000000000000000, 0.000000000000000000, 1.000000000000000000 ) ) ;
#6290 = AXIS2_PLACEMENT_3D ( 'NONE', #6125, #15118, #2963 ) ;
#6291 = CIRCLE ( 'NONE', #25461, 2.000000000000001776 ) ;
#6292 = CYLINDRICAL_SURFACE ( 'NONE', #11675, 3.499999999999989342 ) ;
#6293 = ORIENTED_EDGE ( 'NONE', *, *, #18999, .T. ) ;
#6294 = DIRECTION ( 'NONE',  ( -1.000000000000000000, 0.000000000000000000, 0.000000000000000000 ) ) ;
#6295 = ORIENTED_EDGE ( 'NONE', *, *, #31394, .F. ) ;
#6296 = FACE_BOUND ( 'NONE', #30432, .T. ) ;
#6297 = CARTESIAN_POINT ( 'NONE',  ( 32.99999662536855283, -77.94228634059960825, -9.999999999999998224 ) ) ;
#6298 = VECTOR ( 'NONE', #28389, 1000.000000000000000 ) ;
#6299 = DIRECTION ( 'NONE',  ( 0.000000000000000000, -0.8660254037844420383, -0.4999999999999945599 ) ) ;
#6300 = AXIS2_PLACEMENT_3D ( 'NONE', #5339, #11113, #22932 ) ;
#6301 = ORIENTED_EDGE ( 'NONE', *, *, #17558, .T. ) ;
#6302 = CARTESIAN_POINT ( 'NONE',  ( -67.00000337463102085, 25.98076211353317433, -9.999999999999998224 ) ) ;
#6303 = EDGE_CURVE ( 'NONE', #6715, #4682, #12435, .T. ) ;
#6304 = SHAPE_DEFINITION_REPRESENTATION ( #16936, #35440 ) ;
#6305 = AXIS2_PLACEMENT_3D ( 'NONE', #19824, #8931, #28423 ) ;
#6306 = CIRCLE ( 'NONE', #14681, 33.00000000000002132 ) ;
#6307 = CARTESIAN_POINT ( 'NONE',  ( 29.99999662536857770, -69.28203230275519786, -5.000000000000000000 ) ) ;
#6308 = DIRECTION ( 'NONE',  ( 0.000000000000000000, 0.000000000000000000, 1.000000000000000000 ) ) ;
#6309 = LINE ( 'NONE', #29185, #17337 ) ;
#6310 = ORIENTED_EDGE ( 'NONE', *, *, #2305, .T. ) ;
#6311 = FACE_OUTER_BOUND ( 'NONE', #34335, .T. ) ;
#6312 = DIRECTION ( 'NONE',  ( 0.000000000000000000, 0.4999999999999953926, -0.8660254037844412611 ) ) ;
#6313 = CARTESIAN_POINT ( 'NONE',  ( -35.00000337463116296, -60.62177826491080168, -5.000000000000000000 ) ) ;
#6314 = AXIS2_PLACEMENT_3D ( 'NONE', #31923, #453, #8903 ) ;
#6315 = ORIENTED_EDGE ( 'NONE', *, *, #25901, .F. ) ;
#6316 = EDGE_CURVE ( 'NONE', #12117, #7645, #35807, .T. ) ;
#6317 = ORIENTED_EDGE ( 'NONE', *, *, #22779, .T. ) ;
#6318 = ORIENTED_EDGE ( 'NONE', *, *, #16318, .T. ) ;
#6319 = DIRECTION ( 'NONE',  ( 0.000000000000000000, 0.000000000000000000, -1.000000000000000000 ) ) ;
#6320 = CARTESIAN_POINT ( 'NONE',  ( -90.60231327712325822, -15.97563234535699017, -4.999999999999997335 ) ) ;
#6321 = CIRCLE ( 'NONE', #8741, 2.000000000000001776 ) ;
#6322 = EDGE_CURVE ( 'NONE', #16351, #29605, #26829, .T. ) ;
#6323 = DIRECTION ( 'NONE',  ( 0.000000000000000000, 0.000000000000000000, -1.000000000000000000 ) ) ;
#6324 = DIRECTION ( 'NONE',  ( 1.000000000000000000, 0.000000000000000000, 0.000000000000000000 ) ) ;
#6325 = AXIS2_PLACEMENT_3D ( 'NONE', #4536, #3974, #24214 ) ;
#6326 = LINE ( 'NONE', #11411, #26204 ) ;
#6327 = AXIS2_PLACEMENT_3D ( 'NONE', #29390, #23022, #6324 ) ;
#6328 = VECTOR ( 'NONE', #24192, 1000.000000000000000 ) ;
#6329 = CYLINDRICAL_SURFACE ( 'NONE', #23363, 2.000000000000001776 ) ;
#6330 = CIRCLE ( 'NONE', #5145, 2.000000000000001776 ) ;
#6331 = ORIENTED_EDGE ( 'NONE', *, *, #2648, .F. ) ;
#6332 = ORIENTED_EDGE ( 'NONE', *, *, #8672, .F. ) ;
#6333 = CARTESIAN_POINT ( 'NONE',  ( -73.00000337463099243, -25.98076211353322051, -5.000000000000000000 ) ) ;
#6334 = DIRECTION ( 'NONE',  ( 0.000000000000000000, 0.000000000000000000, 1.000000000000000000 ) ) ;
#6335 = CARTESIAN_POINT ( 'NONE',  ( 68.66839587347284635, 56.74224907228958870, 12.49999999999999645 ) ) ;
#6336 = ORIENTED_EDGE ( 'NONE', *, *, #5772, .F. ) ;
#6337 = CIRCLE ( 'NONE', #32066, 2.000000000000001776 ) ;
#6338 = VECTOR ( 'NONE', #30531, 1000.000000000000114 ) ;
#6339 = FACE_BOUND ( 'NONE', #12691, .T. ) ;
#6340 = ORIENTED_EDGE ( 'NONE', *, *, #31569, .T. ) ;
#6341 = ORIENTED_EDGE ( 'NONE', *, *, #9315, .F. ) ;
#6342 = EDGE_CURVE ( 'NONE', #20659, #12315, #10667, .T. ) ;
#6343 = CARTESIAN_POINT ( 'NONE',  ( 0.8192951148925871063, -5.300482436767286920, -5.801655677627835850 ) ) ;
#6344 = ORIENTED_EDGE ( 'NONE', *, *, #31869, .T. ) ;
#6345 = CIRCLE ( 'NONE', #9942, 2.000000000000000000 ) ;
#6346 = CYLINDRICAL_SURFACE ( 'NONE', #17625, 1.999999999999998224 ) ;
#6347 = AXIS2_PLACEMENT_3D ( 'NONE', #14659, #9414, #29459 ) ;
#6348 = CARTESIAN_POINT ( 'NONE',  ( -101.4252628994512833, -31.43180897937256191, 32.50001250000000397 ) ) ;
#6349 = CARTESIAN_POINT ( 'NONE',  ( 69.13212189986965939, 2.778182860042805125, 12.49999999999999645 ) ) ;
#6350 = VERTEX_POINT ( 'NONE', #14359 ) ;
#6351 = VERTEX_POINT ( 'NONE', #462 ) ;
#6352 = EDGE_CURVE ( 'NONE', #26240, #24381, #25055, .T. ) ;
#6353 = COLOUR_RGB ( '', 0.72549020, 0.75294118, 0.79215686) ;
#6354 = AXIS2_PLACEMENT_3D ( 'NONE', #29109, #32302, #9230 ) ;
#6355 = VECTOR ( 'NONE', #10006, 1000.000000000000000 ) ;
#6356 = ORIENTED_EDGE ( 'NONE', *, *, #26715, .T. ) ;
#6357 = VECTOR ( 'NONE', #20558, 1000.000000000000000 ) ;
#6358 = AXIS2_PLACEMENT_3D ( 'NONE', #16942, #6425, #12031 ) ;
#6359 = ORIENTED_EDGE ( 'NONE', *, *, #14558, .F. ) ;
#6360 = AXIS2_PLACEMENT_3D ( 'NONE', #6601, #32454, #24559 ) ;
#6361 = EDGE_CURVE ( 'NONE', #2049, #40, #31930, .T. ) ;
#6362 = EDGE_LOOP ( 'NONE', ( #15130, #31334 ) ) ;
#6363 = LINE ( 'NONE', #9361, #6867 ) ;
#6364 = ORIENTED_EDGE ( 'NONE', *, *, #5078, .T. ) ;
#6365 = DIRECTION ( 'NONE',  ( 0.000000000000000000, 0.000000000000000000, 1.000000000000000000 ) ) ;
#6366 = DIRECTION ( 'NONE',  ( 0.000000000000000000, 0.000000000000000000, 1.000000000000000000 ) ) ;
#6367 = PLANE ( 'NONE',  #35116 ) ;
#6368 = ORIENTED_EDGE ( 'NONE', *, *, #26539, .T. ) ;
#6369 = FACE_OUTER_BOUND ( 'NONE', #23523, .T. ) ;
#6370 = AXIS2_PLACEMENT_3D ( 'NONE', #20138, #26684, #34394 ) ;
#6371 = CARTESIAN_POINT ( 'NONE',  ( -31.09745072740852123, -83.47442710120344600, -49.86348611802629449 ) ) ;
#6372 = DIRECTION ( 'NONE',  ( 0.000000000000000000, 0.000000000000000000, 1.000000000000000000 ) ) ;
#6373 = ORIENTED_EDGE ( 'NONE', *, *, #1387, .T. ) ;
#6374 = CARTESIAN_POINT ( 'NONE',  ( 79.99999662536832545, -17.32050807568879591, 17.49999999999999645 ) ) ;
#6375 = CYLINDRICAL_SURFACE ( 'NONE', #25599, 2.000000000000001776 ) ;
#6376 = EDGE_LOOP ( 'NONE', ( #1541, #8143 ) ) ;
#6377 = AXIS2_PLACEMENT_3D ( 'NONE', #2325, #5671, #30793 ) ;
#6378 = ORIENTED_EDGE ( 'NONE', *, *, #15982, .T. ) ;
#6379 = ADVANCED_FACE ( 'NONE', ( #17359 ), #3274, .F. ) ;
#6380 = CARTESIAN_POINT ( 'NONE',  ( 0.000000000000000000, 0.000000000000000000, -25.03750572909317285 ) ) ;
#6381 = AXIS2_PLACEMENT_3D ( 'NONE', #12716, #6926, #27159 ) ;
#6382 = CYLINDRICAL_SURFACE ( 'NONE', #4340, 2.000000000000001776 ) ;
#6383 = DIRECTION ( 'NONE',  ( 0.5000000000000039968, 0.8660254037844363761, 0.000000000000000000 ) ) ;
#6384 = CARTESIAN_POINT ( 'NONE',  ( -5.750000000000000000, 89.94802294027094547, -24.99999999999999645 ) ) ;
#6385 = AXIS2_PLACEMENT_3D ( 'NONE', #28433, #31254, #8757 ) ;
#6386 = ORIENTED_EDGE ( 'NONE', *, *, #11837, .F. ) ;
#6387 = AXIS2_PLACEMENT_3D ( 'NONE', #400, #14480, #11474 ) ;
#6388 = ADVANCED_FACE ( 'NONE', ( #9471 ), #3104, .F. ) ;
#6389 = CARTESIAN_POINT ( 'NONE',  ( 0.000000000000000000, 0.000000000000000000, 32.50000000000000000 ) ) ;
#6390 = LINE ( 'NONE', #15759, #6328 ) ;
#6391 = ORIENTED_EDGE ( 'NONE', *, *, #4969, .T. ) ;
#6392 = EDGE_CURVE ( 'NONE', #35809, #14334, #23160, .T. ) ;
#6393 = FACE_OUTER_BOUND ( 'NONE', #12162, .T. ) ;
#6394 = VERTEX_POINT ( 'NONE', #11701 ) ;
#6395 = CARTESIAN_POINT ( 'NONE',  ( -57.00000337463107059, 43.30127018922197379, -9.999999999999998224 ) ) ;
#6396 = SHAPE_REPRESENTATION ( 'mounting backplate', ( #21385 ), #25533 ) ;
#6397 = VECTOR ( 'NONE', #31518, 1000.000000000000000 ) ;
#6398 = DIRECTION ( 'NONE',  ( 1.000000000000000000, 0.000000000000000000, 0.000000000000000000 ) ) ;
#6399 = CARTESIAN_POINT ( 'NONE',  ( 14.99999662536863632, -77.94228634059960825, -9.999999999999998224 ) ) ;
#6400 = ORIENTED_EDGE ( 'NONE', *, *, #5529, .F. ) ;
#6401 = EDGE_LOOP ( 'NONE', ( #35869, #23628, #27979, #36185 ) ) ;
#6402 = CARTESIAN_POINT ( 'NONE',  ( 72.99999662536836809, 43.30127018922198801, -9.999999999999998224 ) ) ;
#6403 = AXIS2_PLACEMENT_3D ( 'NONE', #15703, #1640, #13425 ) ;
#6404 = CIRCLE ( 'NONE', #25587, 27.00000000000001421 ) ;
#6405 = CARTESIAN_POINT ( 'NONE',  ( 79.99999662536832545, -34.64101615137759183, 17.49999999999999645 ) ) ;
#6406 = CARTESIAN_POINT ( 'NONE',  ( 69.99999662536839651, 34.64101615137758472, -5.000000000000000000 ) ) ;
#6407 = EDGE_CURVE ( 'NONE', #22954, #12040, #14530, .T. ) ;
#6408 = AXIS2_PLACEMENT_3D ( 'NONE', #33263, #7582, #13018 ) ;
#6409 = ORIENTED_EDGE ( 'NONE', *, *, #22546, .F. ) ;
#6410 = DIRECTION ( 'NONE',  ( 1.000000000000000000, 0.000000000000000000, 0.000000000000000000 ) ) ;
#6411 = FACE_BOUND ( 'NONE', #2528, .T. ) ;
#6412 = DIRECTION ( 'NONE',  ( 1.000000000000000000, 0.000000000000000000, 0.000000000000000000 ) ) ;
#6413 = CARTESIAN_POINT ( 'NONE',  ( 37.50000000000000000, 103.4105893997321743, 27.49999999999999645 ) ) ;
#6414 = PLANE ( 'NONE',  #18701 ) ;
#6415 = DIRECTION ( 'NONE',  ( -0.000000000000000000, -0.000000000000000000, 1.000000000000000000 ) ) ;
#6416 = AXIS2_PLACEMENT_3D ( 'NONE', #10407, #21847, #16410 ) ;
#6417 = ORIENTED_EDGE ( 'NONE', *, *, #14088, .F. ) ;
#6418 = LINE ( 'NONE', #36217, #20088 ) ;
#6419 = AXIS2_PLACEMENT_3D ( 'NONE', #10484, #16859, #8240 ) ;
#6420 = AXIS2_PLACEMENT_3D ( 'NONE', #7572, #33071, #13206 ) ;
#6421 = CARTESIAN_POINT ( 'NONE',  ( -83.10591231744739105, 8.018055418181152305, 12.50000000000000000 ) ) ;
#6422 = DIRECTION ( 'NONE',  ( -0.000000000000000000, -0.000000000000000000, -1.000000000000000000 ) ) ;
#6423 = ORIENTED_EDGE ( 'NONE', *, *, #34988, .T. ) ;
#6424 = DIRECTION ( 'NONE',  ( -0.000000000000000000, -0.000000000000000000, 1.000000000000000000 ) ) ;
#6425 = DIRECTION ( 'NONE',  ( 0.000000000000000000, 0.000000000000000000, 1.000000000000000000 ) ) ;
#6426 = DIRECTION ( 'NONE',  ( 0.000000000000000000, -0.000000000000000000, 1.000000000000000000 ) ) ;
#6427 = AXIS2_PLACEMENT_3D ( 'NONE', #3139, #6514, #12493 ) ;
#6428 = EDGE_LOOP ( 'NONE', ( #32363, #25815, #6011, #31074, #29642 ) ) ;
#6429 = ORIENTED_EDGE ( 'NONE', *, *, #27251, .T. ) ;
#6430 = EDGE_CURVE ( 'NONE', #8770, #23345, #5265, .T. ) ;
#6431 = ORIENTED_EDGE ( 'NONE', *, *, #15358, .F. ) ;
#6432 = AXIS2_PLACEMENT_3D ( 'NONE', #6988, #10187, #29863 ) ;
#6433 = DIRECTION ( 'NONE',  ( 0.000000000000000000, 0.000000000000000000, -1.000000000000000000 ) ) ;
#6434 = DIRECTION ( 'NONE',  ( 0.000000000000000000, 0.000000000000000000, 1.000000000000000000 ) ) ;
#6435 = EDGE_CURVE ( 'NONE', #22752, #17730, #22044, .T. ) ;
#6436 = DIRECTION ( 'NONE',  ( 0.000000000000000000, 0.000000000000000000, 1.000000000000000000 ) ) ;
#6437 = ORIENTED_EDGE ( 'NONE', *, *, #13618, .T. ) ;
#6438 = ORIENTED_EDGE ( 'NONE', *, *, #19640, .T. ) ;
#6439 = AXIS2_PLACEMENT_3D ( 'NONE', #19759, #30451, #7942 ) ;
#6440 = ORIENTED_EDGE ( 'NONE', *, *, #32078, .T. ) ;
#6441 = EDGE_CURVE ( 'NONE', #33332, #29281, #20506, .T. ) ;
#6442 = DIRECTION ( 'NONE',  ( 0.000000000000000000, 0.000000000000000000, 1.000000000000000000 ) ) ;
#6443 = AXIS2_PLACEMENT_3D ( 'NONE', #18983, #21418, #30209 ) ;
#6444 = ORIENTED_EDGE ( 'NONE', *, *, #33031, .F. ) ;
#6445 = CARTESIAN_POINT ( 'NONE',  ( 0.000000000000000000, 0.000000000000000000, 27.50000000000000000 ) ) ;
#6447 = ADVANCED_FACE ( 'NONE', ( #28948 ), #9084, .T. ) ;
#6446 = ORIENTED_EDGE ( 'NONE', *, *, #7277, .T. ) ;
#6448 = CARTESIAN_POINT ( 'NONE',  ( 1.999996625368672287, 86.60254037844397601, 12.50000000000000000 ) ) ;
#6449 = ORIENTED_EDGE ( 'NONE', *, *, #31999, .T. ) ;
#6450 = EDGE_CURVE ( 'NONE', #9234, #15626, #28615, .T. ) ;
#6451 = VERTEX_POINT ( 'NONE', #26347 ) ;
#6452 = VECTOR ( 'NONE', #30086, 1000.000000000000000 ) ;
#6453 = CIRCLE ( 'NONE', #1043, 2.000000000000001776 ) ;
#6454 = CARTESIAN_POINT ( 'NONE',  ( -145.0000000000001137, -5.999999999998481215, 32.50000000000000000 ) ) ;
#6455 = LINE ( 'NONE', #4004, #22007 ) ;
#6456 = DIRECTION ( 'NONE',  ( 0.000000000000000000, 0.000000000000000000, 1.000000000000000000 ) ) ;
#6457 = EDGE_LOOP ( 'NONE', ( #22170, #34256 ) ) ;
#6458 = VERTEX_POINT ( 'NONE', #23525 ) ;
#6459 = DIRECTION ( 'NONE',  ( 0.000000000000000000, 0.000000000000000000, 1.000000000000000000 ) ) ;
#6460 = CIRCLE ( 'NONE', #2884, 30.00000000000000000 ) ;
#6461 = EDGE_CURVE ( 'NONE', #17975, #36602, #34965, .T. ) ;
#6462 = CARTESIAN_POINT ( 'NONE',  ( 52.39915983220795681, 35.19434990244919703, -49.22241343995293761 ) ) ;
#6463 = EDGE_CURVE ( 'NONE', #12329, #26842, #13039, .T. ) ;
#6464 = DIRECTION ( 'NONE',  ( 1.000000000000000000, 0.000000000000000000, 0.000000000000000000 ) ) ;
#6465 = EDGE_CURVE ( 'NONE', #33068, #3582, #28003, .T. ) ;
#6466 = EDGE_LOOP ( 'NONE', ( #16468, #16631, #1260, #30822 ) ) ;
#6467 = DIRECTION ( 'NONE',  ( 1.000000000000000000, 0.000000000000000000, 0.000000000000000000 ) ) ;
#6469 = VECTOR ( 'NONE', #17471, 1000.000000000000000 ) ;
#6468 = DIRECTION ( 'NONE',  ( 0.8660254037844382635, 0.5000000000000005551, 0.000000000000000000 ) ) ;
#6470 = ADVANCED_FACE ( 'NONE', ( #15820 ), #26700, .F. ) ;
#6471 = ORIENTED_EDGE ( 'NONE', *, *, #30727, .T. ) ;
#6472 = DIRECTION ( 'NONE',  ( -1.000000000000000000, -0.000000000000000000, -0.000000000000000000 ) ) ;
#6473 = AXIS2_PLACEMENT_3D ( 'NONE', #4837, #33877, #30517 ) ;
#6474 = CIRCLE ( 'NONE', #7677, 3.000000000000007105 ) ;
#6475 = FACE_OUTER_BOUND ( 'NONE', #27330, .T. ) ;
#6476 = CARTESIAN_POINT ( 'NONE',  ( -5.000000000000000000, 2.886751345948126879, -2.079999999999992077 ) ) ;
#6478 = CIRCLE ( 'NONE', #2270, 2.000000000000001776 ) ;
#6477 = CARTESIAN_POINT ( 'NONE',  ( -4.279621169095561228, 62.97617850287782915, -4.999999999999997335 ) ) ;
#6479 = DIRECTION ( 'NONE',  ( 1.000000000000000000, 0.000000000000000000, 0.000000000000000000 ) ) ;
#6480 = CIRCLE ( 'NONE', #14876, 5.750000000000002665 ) ;
#6481 = CARTESIAN_POINT ( 'NONE',  ( 37.50000000000000000, 103.4105893997321743, -19.99999999999999645 ) ) ;
#6482 = ORIENTED_EDGE ( 'NONE', *, *, #20485, .F. ) ;
#6483 = DIRECTION ( 'NONE',  ( 0.000000000000000000, 0.000000000000000000, 1.000000000000000000 ) ) ;
#6484 = CARTESIAN_POINT ( 'NONE',  ( 59.13646009116148150, -70.47608876694609137, 12.49999999999999822 ) ) ;
#6485 = CARTESIAN_POINT ( 'NONE',  ( -90.00000337463090716, -1.040834085586084257E-14, -9.999999999999998224 ) ) ;
#6486 = ORIENTED_EDGE ( 'NONE', *, *, #4264, .T. ) ;
#6487 = VECTOR ( 'NONE', #16683, 1000.000000000000000 ) ;
#6488 = ORIENTED_EDGE ( 'NONE', *, *, #18601, .F. ) ;
#6489 = ORIENTED_EDGE ( 'NONE', *, *, #19945, .T. ) ;
#6490 = CARTESIAN_POINT ( 'NONE',  ( -5.750000000000000000, 89.94802294027094547, -24.99999999999999645 ) ) ;
#6491 = DIRECTION ( 'NONE',  ( 1.000000000000000000, 0.000000000000000000, 0.000000000000000000 ) ) ;
#6492 = CARTESIAN_POINT ( 'NONE',  ( 44.99999662536851019, -60.62177826491080168, -9.999999999999998224 ) ) ;
#6493 = CARTESIAN_POINT ( 'NONE',  ( -80.00000337463094979, -2.428612866367529932E-14, -9.999999999999998224 ) ) ;
#6494 = AXIS2_PLACEMENT_3D ( 'NONE', #17427, #17986, #34693 ) ;
#6495 = DIRECTION ( 'NONE',  ( 0.000000000000000000, 0.000000000000000000, 1.000000000000000000 ) ) ;
#6496 = EDGE_LOOP ( 'NONE', ( #28432, #29880 ) ) ;
#6497 = DIRECTION ( 'NONE',  ( 0.000000000000000000, 0.000000000000000000, 1.000000000000000000 ) ) ;
#6498 = EDGE_LOOP ( 'NONE', ( #10311, #30224 ) ) ;
#6499 = VECTOR ( 'NONE', #26053, 1000.000000000000000 ) ;
#6500 = FACE_BOUND ( 'NONE', #12889, .T. ) ;
#6501 = VECTOR ( 'NONE', #19806, 1000.000000000000000 ) ;
#6502 = AXIS2_PLACEMENT_3D ( 'NONE', #21925, #18378, #15571 ) ;
#6503 = DIRECTION ( 'NONE',  ( 1.000000000000000000, 0.000000000000000000, 0.000000000000000000 ) ) ;
#6504 = CARTESIAN_POINT ( 'NONE',  ( -87.00000337463093558, -8.660254037844422825, 17.49999999999999645 ) ) ;
#6505 = ORIENTED_EDGE ( 'NONE', *, *, #10425, .T. ) ;
#6506 = DIRECTION ( 'NONE',  ( 0.000000000000000000, 0.000000000000000000, 1.000000000000000000 ) ) ;
#6507 = DIRECTION ( 'NONE',  ( 0.000000000000000000, 0.000000000000000000, 1.000000000000000000 ) ) ;
#6508 = DIRECTION ( 'NONE',  ( 0.000000000000000000, 0.000000000000000000, 1.000000000000000000 ) ) ;
#6509 = VECTOR ( 'NONE', #6264, 1000.000000000000000 ) ;
#6510 = CARTESIAN_POINT ( 'NONE',  ( 3.000000000000000000, -1.467624384280027172, 2.542000000000001592 ) ) ;
#6511 = DIRECTION ( 'NONE',  ( 1.000000000000000000, 0.000000000000000000, 0.000000000000000000 ) ) ;
#6512 = EDGE_CURVE ( 'NONE', #28925, #35441, #1668, .T. ) ;
#6513 = EDGE_LOOP ( 'NONE', ( #23879, #27884, #7382, #28237 ) ) ;
#6514 = DIRECTION ( 'NONE',  ( 0.000000000000000000, -0.8660254037844419273, -0.4999999999999945599 ) ) ;
#6515 = DIRECTION ( 'NONE',  ( 0.1391731009600657432, 1.704378926181559679E-17, -0.9902680687415703620 ) ) ;
#6516 = CARTESIAN_POINT ( 'NONE',  ( -5.000003374631307729, 77.94228634059957983, 17.49999999999999645 ) ) ;
#6517 = ORIENTED_EDGE ( 'NONE', *, *, #36910, .F. ) ;
#6518 = ORIENTED_EDGE ( 'NONE', *, *, #27943, .F. ) ;
#6519 = AXIS2_PLACEMENT_3D ( 'NONE', #14796, #31473, #23428 ) ;
#6520 = VERTEX_POINT ( 'NONE', #21811 ) ;
#6521 = AXIS2_PLACEMENT_3D ( 'NONE', #17201, #20537, #9294 ) ;
#6522 = DIRECTION ( 'NONE',  ( 0.000000000000000000, 0.000000000000000000, 1.000000000000000000 ) ) ;
#6523 = PLANE ( 'NONE',  #27287 ) ;
#6524 = CARTESIAN_POINT ( 'NONE',  ( 67.30619744048945563, -84.18124734178287838, 27.50000000000000000 ) ) ;
#6525 = CIRCLE ( 'NONE', #2335, 2.000000000000001776 ) ;
#6526 = CARTESIAN_POINT ( 'NONE',  ( -92.00000337463090716, -1.016341149603137227E-14, 12.50000000000000000 ) ) ;
#6527 = DIRECTION ( 'NONE',  ( 0.000000000000000000, 0.000000000000000000, 1.000000000000000000 ) ) ;
#6528 = EDGE_CURVE ( 'NONE', #32462, #16311, #6460, .T. ) ;
#6530 = DIRECTION ( 'NONE',  ( 0.000000000000000000, 0.000000000000000000, 1.000000000000000000 ) ) ;
#6529 = VECTOR ( 'NONE', #24588, 1000.000000000000000 ) ;
#6531 = EDGE_CURVE ( 'NONE', #12570, #13186, #32189, .T. ) ;
#6532 = VERTEX_POINT ( 'NONE', #1569 ) ;
#6533 = VERTEX_POINT ( 'NONE', #35527 ) ;
#6534 = FACE_OUTER_BOUND ( 'NONE', #749, .T. ) ;
#6535 = CIRCLE ( 'NONE', #5955, 2.000000000000001776 ) ;
#6536 = DIRECTION ( 'NONE',  ( 1.000000000000000000, 0.000000000000000000, 0.000000000000000000 ) ) ;
#6537 = ORIENTED_EDGE ( 'NONE', *, *, #27528, .F. ) ;
#6538 = AXIS2_PLACEMENT_3D ( 'NONE', #23361, #20512, #3482 ) ;
#6539 = FACE_OUTER_BOUND ( 'NONE', #20336, .T. ) ;
#6540 = ORIENTED_EDGE ( 'NONE', *, *, #11667, .F. ) ;
#6541 = ADVANCED_FACE ( 'NONE', ( #29504 ), #18829, .F. ) ;
#6542 = ADVANCED_FACE ( 'NONE', ( #21255 ), #1768, .F. ) ;
#6543 = FACE_BOUND ( 'NONE', #15314, .T. ) ;
#6544 = CIRCLE ( 'NONE', #8350, 27.00000000000001421 ) ;
#6545 = ORIENTED_EDGE ( 'NONE', *, *, #6361, .F. ) ;
#6546 = VERTEX_POINT ( 'NONE', #35905 ) ;
#6547 = CIRCLE ( 'NONE', #8354, 27.00000000000001421 ) ;
#6548 = FACE_OUTER_BOUND ( 'NONE', #7493, .T. ) ;
#6549 = ORIENTED_EDGE ( 'NONE', *, *, #8641, .T. ) ;
#6550 = CARTESIAN_POINT ( 'NONE',  ( 6.000000000000000000, 5.000000000000000000, 0.000000000000000000 ) ) ;
#6551 = DIRECTION ( 'NONE',  ( 0.000000000000000000, 0.000000000000000000, 1.000000000000000000 ) ) ;
#6552 = DIRECTION ( 'NONE',  ( 0.000000000000000000, 1.000000000000000000, -1.034244904716769672E-15 ) ) ;
#6553 = AXIS2_PLACEMENT_3D ( 'NONE', #35733, #32526, #7411 ) ;
#6554 = EDGE_CURVE ( 'NONE', #20492, #15386, #7668, .T. ) ;
#6555 = ORIENTED_EDGE ( 'NONE', *, *, #17358, .T. ) ;
#6556 = ORIENTED_EDGE ( 'NONE', *, *, #27, .F. ) ;
#6557 = CIRCLE ( 'NONE', #14351, 3.499999999999991562 ) ;
#6558 = ORIENTED_EDGE ( 'NONE', *, *, #486, .F. ) ;
#6559 = ORIENTED_EDGE ( 'NONE', *, *, #23183, .T. ) ;
#6560 = AXIS2_PLACEMENT_3D ( 'NONE', #26739, #23749, #11925 ) ;
#6561 = VERTEX_POINT ( 'NONE', #27448 ) ;
#6562 = CARTESIAN_POINT ( 'NONE',  ( 59.99999662536842493, -51.96152422706639840, 12.50000000000000000 ) ) ;
#6563 = PLANE ( 'NONE',  #23970 ) ;
#6564 = ORIENTED_EDGE ( 'NONE', *, *, #32083, .T. ) ;
#6565 = CARTESIAN_POINT ( 'NONE',  ( 64.99999662536842493, 43.30127018922200222, -9.999999999999998224 ) ) ;
#6566 = DIRECTION ( 'NONE',  ( 1.000000000000000000, 0.000000000000000000, 0.000000000000000000 ) ) ;
#6567 = CARTESIAN_POINT ( 'NONE',  ( 17.99999662536858835, 69.28203230275516944, -9.999999999999998224 ) ) ;
#6568 = VERTEX_POINT ( 'NONE', #7215 ) ;
#6569 = DIRECTION ( 'NONE',  ( 0.000000000000000000, 0.000000000000000000, 1.000000000000000000 ) ) ;
#6570 = CARTESIAN_POINT ( 'NONE',  ( -78.00000337463094979, -17.32050807568882078, -5.000000000000000000 ) ) ;
#6571 = CIRCLE ( 'NONE', #14336, 2.000000000000001776 ) ;
#6572 = ADVANCED_FACE ( 'NONE', ( #4391 ), #18466, .F. ) ;
#6573 = ORIENTED_EDGE ( 'NONE', *, *, #27053, .T. ) ;
#6574 = DIRECTION ( 'NONE',  ( -1.047444401652940007E-14, -1.000000000000000000, 0.000000000000000000 ) ) ;
#6575 = FACE_OUTER_BOUND ( 'NONE', #11995, .T. ) ;
#6576 = ADVANCED_FACE ( 'NONE', ( #4580, #30066 ), #35367, .T. ) ;
#6577 = ORIENTED_EDGE ( 'NONE', *, *, #24598, .T. ) ;
#6578 = ORIENTED_EDGE ( 'NONE', *, *, #30808, .T. ) ;
#6579 = DIRECTION ( 'NONE',  ( 1.000000000000000000, 0.000000000000000000, 0.000000000000000000 ) ) ;
#6580 = DIRECTION ( 'NONE',  ( 1.000000000000000000, 0.000000000000000000, 0.000000000000000000 ) ) ;
#6581 = CARTESIAN_POINT ( 'NONE',  ( 49.99999662536846756, 51.96152422706637708, 12.50000000000000000 ) ) ;
#6582 = CARTESIAN_POINT ( 'NONE',  ( -52.39915983220772233, -35.19434990244957362, 12.49999999999999822 ) ) ;
#6583 = EDGE_CURVE ( 'NONE', #3455, #15010, #7385, .T. ) ;
#6584 = EDGE_LOOP ( 'NONE', ( #17012, #4356 ) ) ;
#6585 = VECTOR ( 'NONE', #4712, 1000.000000000000000 ) ;
#6586 = FACE_BOUND ( 'NONE', #11584, .T. ) ;
#6587 = CARTESIAN_POINT ( 'NONE',  ( -6.000000000000000000, 145.0000000000000568, 32.55002500000000509 ) ) ;
#6588 = EDGE_CURVE ( 'NONE', #3448, #14395, #16778, .T. ) ;
#6589 = ORIENTED_EDGE ( 'NONE', *, *, #36000, .F. ) ;
#6590 = CIRCLE ( 'NONE', #23967, 2.000000000000001776 ) ;
#6591 = CYLINDRICAL_SURFACE ( 'NONE', #15402, 2.000000000000001776 ) ;
#6592 = AXIS2_PLACEMENT_3D ( 'NONE', #1166, #9605, #24038 ) ;
#6593 = ORIENTED_EDGE ( 'NONE', *, *, #1479, .T. ) ;
#6594 = DIRECTION ( 'NONE',  ( 0.000000000000000000, 0.000000000000000000, 1.000000000000000000 ) ) ;
#6595 = CARTESIAN_POINT ( 'NONE',  ( -61.25926521283079751, 32.16008401677975570, -49.22241343995295892 ) ) ;
#6596 = CARTESIAN_POINT ( 'NONE',  ( -53.00000337463106348, 60.62177826491078747, -9.999999999999998224 ) ) ;
#6597 = VERTEX_POINT ( 'NONE', #15264 ) ;
#6598 = ORIENTED_EDGE ( 'NONE', *, *, #578, .T. ) ;
#6599 = AXIS2_PLACEMENT_3D ( 'NONE', #18511, #32740, #15868 ) ;
#6600 = DIRECTION ( 'NONE',  ( 0.000000000000000000, 0.000000000000000000, -1.000000000000000000 ) ) ;
#6601 = CARTESIAN_POINT ( 'NONE',  ( -55.00000337463109901, -60.62177826491083010, 17.49999999999999645 ) ) ;
#6602 = EDGE_CURVE ( 'NONE', #15126, #18489, #23358, .T. ) ;
#6603 = VERTEX_POINT ( 'NONE', #15463 ) ;
#6604 = DIRECTION ( 'NONE',  ( 1.000000000000000000, 0.000000000000000000, 0.000000000000000000 ) ) ;
#6605 = DIRECTION ( 'NONE',  ( -1.000000000000000000, 0.000000000000000000, -0.000000000000000000 ) ) ;
#6606 = VECTOR ( 'NONE', #13294, 1000.000000000000227 ) ;
#6607 = CARTESIAN_POINT ( 'NONE',  ( 42.97377950131527058, 96.90768712682506703, -19.99999999999999645 ) ) ;
#6608 = CARTESIAN_POINT ( 'NONE',  ( -5.236872748402766398, -8.269757189038523917E-14, -4.057689166958448723 ) ) ;
#6609 = DIRECTION ( 'NONE',  ( 0.000000000000000000, 0.000000000000000000, 1.000000000000000000 ) ) ;
#6610 = EDGE_LOOP ( 'NONE', ( #5967, #31234 ) ) ;
#6611 = CARTESIAN_POINT ( 'NONE',  ( -15.00000337463126066, 77.94228634059957983, -9.999999999999998224 ) ) ;
#6612 = EDGE_CURVE ( 'NONE', #30149, #20872, #11956, .T. ) ;
#6613 = EDGE_CURVE ( 'NONE', #22407, #9038, #28723, .T. ) ;
#6614 = CIRCLE ( 'NONE', #16210, 2.000000000000001776 ) ;
#6615 = CARTESIAN_POINT ( 'NONE',  ( -65.00000337463104927, -43.30127018922202353, -9.999999999999998224 ) ) ;
#6616 = ORIENTED_EDGE ( 'NONE', *, *, #8297, .F. ) ;
#6617 = CARTESIAN_POINT ( 'NONE',  ( -57.00000337463107059, 60.62177826491078747, -5.000000000000000000 ) ) ;
#6618 = DIRECTION ( 'NONE',  ( -0.7650473262243666639, 0.6439740589782693148, 0.000000000000000000 ) ) ;
#6619 = CIRCLE ( 'NONE', #10799, 2.000000000000000000 ) ;
#6620 = CARTESIAN_POINT ( 'NONE',  ( 4.279621169095998212, -62.97617850287780072, -4.999999999999997335 ) ) ;
#6621 = ORIENTED_EDGE ( 'NONE', *, *, #11776, .T. ) ;
#6622 = ORIENTED_EDGE ( 'NONE', *, *, #4961, .T. ) ;
#6623 = DIRECTION ( 'NONE',  ( 0.000000000000000000, 0.000000000000000000, 1.000000000000000000 ) ) ;
#6624 = DIRECTION ( 'NONE',  ( 0.000000000000000000, 0.000000000000000000, 1.000000000000000000 ) ) ;
#6625 = CARTESIAN_POINT ( 'NONE',  ( -40.00000337463113453, -69.28203230275519786, 12.50000000000000000 ) ) ;
#6626 = VERTEX_POINT ( 'NONE', #13559 ) ;
#6627 = EDGE_LOOP ( 'NONE', ( #29741, #4091 ) ) ;
#6628 = ORIENTED_EDGE ( 'NONE', *, *, #13188, .T. ) ;
#6629 = FACE_OUTER_BOUND ( 'NONE', #29157, .T. ) ;
#6630 = ADVANCED_FACE ( 'NONE', ( #14108, #22557, #25561, #2120, #22010, #28354, #2503, #22368, #37004, #11311, #4942, #31188, #7769, #8326, #16211, #10929, #27628, #34014, #5129, #30794, #31000, #5332, #10764, #33812, #19758, #5501, #16929, #16568, #28000, #1939, #13365, #2327, #33638, #16378, #16765, #22760, #13757, #36454, #34202, #25373, #19212, #19021, #22201, #8124, #7941, #19567, #28185, #13927, #24824, #36260, #30449, #4775, #27801, #19375, #10570, #36805, #33455, #25208, #36635, #11109, #20300, #3066, #6054, #29283, #6411, #25760, #26102, #9212, #34918, #17479, #31722, #28546, #23478, #12188, #8859, #14311, #8496, #28899, #23301, #15039, #3227, #6219, #20643, #20107, #28738, #3611, #23658, #19924, #5673, #605, #32074, #17850, #26466, #8667, #11844, #775, #20465, #218, #31534, #12021, #14656, #31349, #17115, #2881, #54, #5875, #34750, #11480, #31886, #11648, #17312, #22927, #409, #9042, #14485, #34365, #25920, #23104, #14856, #34556, #17652, #29086, #3422, #26297, #6965, #12585, #21030, #21406, #1722, #32640, #18205, #24414, #4344, #23858, #15776, #32458, #27196, #32280, #4531, #32849, #13156, #35856, #6770, #10169, #27023, #21601 ), #29455, .T. ) ;
#6631 = ORIENTED_EDGE ( 'NONE', *, *, #22729, .T. ) ;
#6632 = CARTESIAN_POINT ( 'NONE',  ( -2.577278915392902991, -120.0000464694457776, 32.50000000000000711 ) ) ;
#6633 = ORIENTED_EDGE ( 'NONE', *, *, #1259, .F. ) ;
#6634 = CARTESIAN_POINT ( 'NONE',  ( 35.99999999999999289, 0.000000000000000000, 0.000000000000000000 ) ) ;
#6635 = VERTEX_POINT ( 'NONE', #21205 ) ;
#6636 = ORIENTED_EDGE ( 'NONE', *, *, #2323, .T. ) ;
#6637 = FACE_BOUND ( 'NONE', #17400, .T. ) ;
#6639 = CIRCLE ( 'NONE', #34201, 2.000000000000001776 ) ;
#6638 = CARTESIAN_POINT ( 'NONE',  ( 47.63139720814400846, -27.50000000000022737, -10.00000000000000000 ) ) ;
#6640 = VERTEX_POINT ( 'NONE', #26849 ) ;
#6641 = ORIENTED_EDGE ( 'NONE', *, *, #2245, .T. ) ;
#6642 = DIRECTION ( 'NONE',  ( 1.000000000000000000, 0.000000000000000000, 0.000000000000000000 ) ) ;
#6643 = CARTESIAN_POINT ( 'NONE',  ( -87.00000337463093558, 25.98076211353317433, -5.000000000000000000 ) ) ;
#6644 = DIRECTION ( 'NONE',  ( 0.000000000000000000, 0.000000000000000000, -1.000000000000000000 ) ) ;
#6645 = CARTESIAN_POINT ( 'NONE',  ( -5.236775518523551831, -1.021013561554246607, -4.056148586100849052 ) ) ;
#6646 = ADVANCED_FACE ( 'NONE', ( #18416 ), #15601, .F. ) ;
#6647 = ORIENTED_EDGE ( 'NONE', *, *, #16968, .F. ) ;
#6648 = DIRECTION ( 'NONE',  ( 1.000000000000000000, 0.000000000000000000, 0.000000000000000000 ) ) ;
#6649 = DIRECTION ( 'NONE',  ( 1.000000000000000000, 0.000000000000000000, 0.000000000000000000 ) ) ;
#6650 = ORIENTED_EDGE ( 'NONE', *, *, #29801, .T. ) ;
#6651 = EDGE_CURVE ( 'NONE', #29787, #4982, #4198, .T. ) ;
#6652 = DIRECTION ( 'NONE',  ( 0.000000000000000000, 0.000000000000000000, 1.000000000000000000 ) ) ;
#6653 = CARTESIAN_POINT ( 'NONE',  ( -70.80619744049063513, -84.18124734178186941, 32.50000000000000000 ) ) ;
#6654 = DIRECTION ( 'NONE',  ( 1.000000000000000000, 0.000000000000000000, 0.000000000000000000 ) ) ;
#6655 = CARTESIAN_POINT ( 'NONE',  ( -5.000000000000000888, 2.886751345948107783, -3.984345921091764886 ) ) ;
#6656 = EDGE_CURVE ( 'NONE', #17608, #29309, #25744, .T. ) ;
#6657 = CARTESIAN_POINT ( 'NONE',  ( 24.99999662536857059, 77.94228634059957983, -5.000000000000000000 ) ) ;
#6658 = CARTESIAN_POINT ( 'NONE',  ( -44.13139720814439215, -27.49999999999955591, -10.00000000000000178 ) ) ;
#6659 = ORIENTED_EDGE ( 'NONE', *, *, #29871, .F. ) ;
#6660 = CARTESIAN_POINT ( 'NONE',  ( 0.000000000000000000, 0.000000000000000000, -6.000000000000001776 ) ) ;
#6661 = EDGE_CURVE ( 'NONE', #23345, #2049, #35334, .T. ) ;
#6662 = DIRECTION ( 'NONE',  ( 1.000000000000000000, 0.000000000000000000, 0.000000000000000000 ) ) ;
#6663 = DIRECTION ( 'NONE',  ( 1.000000000000000000, 0.000000000000000000, 0.000000000000000000 ) ) ;
#6664 = EDGE_CURVE ( 'NONE', #23562, #22366, #19161, .T. ) ;
#6665 = EDGE_LOOP ( 'NONE', ( #19613, #27048, #8348, #12982 ) ) ;
#6666 = VERTEX_POINT ( 'NONE', #7342 ) ;
#6667 = ORIENTED_EDGE ( 'NONE', *, *, #13683, .F. ) ;
#6668 = CARTESIAN_POINT ( 'NONE',  ( -70.47608876694631874, -59.13646009116124702, -4.999999999999997335 ) ) ;
#6669 = DIRECTION ( 'NONE',  ( 1.000000000000000000, 0.000000000000000000, 0.000000000000000000 ) ) ;
#6670 = DIRECTION ( 'NONE',  ( -1.000000000000000000, 0.000000000000000000, 0.000000000000000000 ) ) ;
#6671 = EDGE_CURVE ( 'NONE', #25751, #5018, #15412, .T. ) ;
#6672 = EDGE_CURVE ( 'NONE', #20316, #8483, #12548, .T. ) ;
#6673 = CARTESIAN_POINT ( 'NONE',  ( 66.99999662536842493, 43.30127018922200222, -5.000000000000000000 ) ) ;
#6674 = EDGE_CURVE ( 'NONE', #27152, #16822, #8397, .T. ) ;
#6675 = CARTESIAN_POINT ( 'NONE',  ( -108.3061974404896262, 19.22934205795090534, 32.50000000000000000 ) ) ;
#6676 = ORIENTED_EDGE ( 'NONE', *, *, #20106, .F. ) ;
#6677 = EDGE_CURVE ( 'NONE', #29194, #17753, #33542, .T. ) ;
#6678 = LINE ( 'NONE', #26730, #35355 ) ;
#6679 = ORIENTED_EDGE ( 'NONE', *, *, #3650, .T. ) ;
#6680 = FACE_BOUND ( 'NONE', #31484, .T. ) ;
#6681 = DIRECTION ( 'NONE',  ( -0.000000000000000000, -0.000000000000000000, 1.000000000000000000 ) ) ;
#6682 = VECTOR ( 'NONE', #34237, 1000.000000000000000 ) ;
#6683 = LINE ( 'NONE', #21670, #5621 ) ;
#6684 = ORIENTED_EDGE ( 'NONE', *, *, #21793, .T. ) ;
#6685 = DIRECTION ( 'NONE',  ( 0.8660254037844415942, 0.4999999999999949485, 0.000000000000000000 ) ) ;
#6686 = AXIS2_PLACEMENT_3D ( 'NONE', #33932, #20720, #34296 ) ;
#6687 = DIRECTION ( 'NONE',  ( 3.491481338843133355E-15, 1.000000000000000000, 0.000000000000000000 ) ) ;
#6688 = EDGE_CURVE ( 'NONE', #17057, #24286, #32935, .T. ) ;
#6689 = CARTESIAN_POINT ( 'NONE',  ( -2.374207310413330682E-13, -68.00000000000000000, 12.49999999999999822 ) ) ;
#6690 = CARTESIAN_POINT ( 'NONE',  ( -37.00000337463116296, 60.62177826491077326, 12.50000000000000000 ) ) ;
#6691 = ORIENTED_EDGE ( 'NONE', *, *, #30948, .F. ) ;
#6692 = DIRECTION ( 'NONE',  ( 0.000000000000000000, 0.000000000000000000, 1.000000000000000000 ) ) ;
#6693 = CARTESIAN_POINT ( 'NONE',  ( 64.99999662536839651, 60.62177826491078747, 17.49999999999999645 ) ) ;
#6694 = CARTESIAN_POINT ( 'NONE',  ( -70.00000337463102085, -34.64101615137762025, -9.999999999999998224 ) ) ;
#6695 = VERTEX_POINT ( 'NONE', #27402 ) ;
#6696 = ORIENTED_EDGE ( 'NONE', *, *, #22776, .F. ) ;
#6697 = ORIENTED_EDGE ( 'NONE', *, *, #28221, .T. ) ;
#6698 = EDGE_CURVE ( 'NONE', #21989, #12964, #24570, .T. ) ;
#6699 = CYLINDRICAL_SURFACE ( 'NONE', #17736, 2.000000000000001776 ) ;
#6700 = DIRECTION ( 'NONE',  ( 1.000000000000000000, 0.000000000000000000, 0.000000000000000000 ) ) ;
#6701 = LINE ( 'NONE', #29554, #9311 ) ;
#6702 = CIRCLE ( 'NONE', #24701, 2.000000000000001776 ) ;
#6703 = DIRECTION ( 'NONE',  ( 0.000000000000000000, 0.000000000000000000, 1.000000000000000000 ) ) ;
#6704 = DIRECTION ( 'NONE',  ( -0.000000000000000000, -0.000000000000000000, 1.000000000000000000 ) ) ;
#6705 = DIRECTION ( 'NONE',  ( 1.000000000000000000, 0.000000000000000000, 0.000000000000000000 ) ) ;
#6706 = ORIENTED_EDGE ( 'NONE', *, *, #35454, .T. ) ;
#6708 = ORIENTED_EDGE ( 'NONE', *, *, #5491, .F. ) ;
#6707 = EDGE_CURVE ( 'NONE', #15541, #30886, #8277, .T. ) ;
#6709 = FACE_OUTER_BOUND ( 'NONE', #26783, .T. ) ;
#6710 = EDGE_CURVE ( 'NONE', #6874, #5579, #15562, .T. ) ;
#6711 = DIRECTION ( 'NONE',  ( -0.8660254037844379305, 0.5000000000000011102, 0.000000000000000000 ) ) ;
#6713 = EDGE_CURVE ( 'NONE', #3771, #31778, #590, .T. ) ;
#6712 = ORIENTED_EDGE ( 'NONE', *, *, #12096, .F. ) ;
#6714 = DIRECTION ( 'NONE',  ( 1.000000000000000000, 0.000000000000000000, 0.000000000000000000 ) ) ;
#6715 = VERTEX_POINT ( 'NONE', #36592 ) ;
#6716 = FACE_BOUND ( 'NONE', #23174, .T. ) ;
#6717 = ORIENTED_EDGE ( 'NONE', *, *, #30503, .F. ) ;
#6718 = EDGE_LOOP ( 'NONE', ( #5484, #35460, #16708, #16605 ) ) ;
#6719 = CARTESIAN_POINT ( 'NONE',  ( -68.00000337463102085, -34.64101615137762025, -9.999999999999998224 ) ) ;
#6720 = ORIENTED_EDGE ( 'NONE', *, *, #16086, .T. ) ;
#6721 = DIRECTION ( 'NONE',  ( 0.000000000000000000, 0.000000000000000000, 1.000000000000000000 ) ) ;
#6722 = AXIS2_PLACEMENT_3D ( 'NONE', #34159, #28857, #8455 ) ;
#6723 = CARTESIAN_POINT ( 'NONE',  ( 52.39915983220795681, 35.19434990244919703, -4.999999999999997335 ) ) ;
#6724 = DIRECTION ( 'NONE',  ( 0.000000000000000000, 0.000000000000000000, -1.000000000000000000 ) ) ;
#6725 = EDGE_LOOP ( 'NONE', ( #17371, #2574, #6916, #34177 ) ) ;
#6726 = ORIENTED_EDGE ( 'NONE', *, *, #12081, .F. ) ;
#6727 = EDGE_LOOP ( 'NONE', ( #33995, #36190 ) ) ;
#6728 = EDGE_CURVE ( 'NONE', #8890, #12147, #21559, .T. ) ;
#6729 = ORIENTED_EDGE ( 'NONE', *, *, #16090, .T. ) ;
#6730 = ORIENTED_EDGE ( 'NONE', *, *, #18137, .T. ) ;
#6731 = CARTESIAN_POINT ( 'NONE',  ( -25.30168483247182820, 79.91940249752995840, 12.50000000000000000 ) ) ;
#6732 = DIRECTION ( 'NONE',  ( 1.000000000000000000, 0.000000000000000000, 0.000000000000000000 ) ) ;
#6733 = VERTEX_POINT ( 'NONE', #30588 ) ;
#6734 = CARTESIAN_POINT ( 'NONE',  ( -62.97617850287781494, -4.279621169095772615, 12.49999999999999822 ) ) ;
#6735 = CARTESIAN_POINT ( 'NONE',  ( 101.8359879928019893, 31.92197653850545436, 32.50000000000000000 ) ) ;
#6736 = LINE ( 'NONE', #18169, #2212 ) ;
#6737 = ORIENTED_EDGE ( 'NONE', *, *, #13435, .T. ) ;
#6738 = CYLINDRICAL_SURFACE ( 'NONE', #7486, 3.000000000000002665 ) ;
#6739 = CIRCLE ( 'NONE', #33683, 3.499999999999996003 ) ;
#6740 = DIRECTION ( 'NONE',  ( 0.000000000000000000, 0.000000000000000000, 1.000000000000000000 ) ) ;
#6741 = CARTESIAN_POINT ( 'NONE',  ( -30.00000337463118427, 69.28203230275516944, 12.50000000000000000 ) ) ;
#6742 = ORIENTED_EDGE ( 'NONE', *, *, #19830, .T. ) ;
#6743 = DIRECTION ( 'NONE',  ( 1.000000000000000000, 0.000000000000000000, 0.000000000000000000 ) ) ;
#6744 = CARTESIAN_POINT ( 'NONE',  ( -78.00000337463094979, 17.32050807568878525, 12.50000000000000000 ) ) ;
#6745 = EDGE_LOOP ( 'NONE', ( #1671, #26277, #16426, #9957 ) ) ;
#6746 = VERTEX_POINT ( 'NONE', #33200 ) ;
#6747 = DIRECTION ( 'NONE',  ( 1.000000000000000000, 0.000000000000000000, 0.000000000000000000 ) ) ;
#6748 = AXIS2_PLACEMENT_3D ( 'NONE', #19303, #4308, #7304 ) ;
#6749 = DIRECTION ( 'NONE',  ( 0.000000000000000000, 0.000000000000000000, 1.000000000000000000 ) ) ;
#6750 = EDGE_CURVE ( 'NONE', #29589, #12416, #8971, .T. ) ;
#6751 = DIRECTION ( 'NONE',  ( 0.000000000000000000, 0.000000000000000000, 1.000000000000000000 ) ) ;
#6752 = AXIS2_PLACEMENT_3D ( 'NONE', #2133, #16581, #22211 ) ;
#6753 = CARTESIAN_POINT ( 'NONE',  ( -5.750000000000000000, 96.68456697298042002, -25.00000000000000000 ) ) ;
#6754 = EDGE_LOOP ( 'NONE', ( #12308, #24533, #20269, #8106 ) ) ;
#6755 = CARTESIAN_POINT ( 'NONE',  ( -67.30619744048885877, 84.18124734178336155, 32.50000000000000000 ) ) ;
#6756 = CYLINDRICAL_SURFACE ( 'NONE', #17131, 2.000000000000001776 ) ;
#6757 = ORIENTED_EDGE ( 'NONE', *, *, #20735, .F. ) ;
#6758 = PLANE ( 'NONE',  #35777 ) ;
#6759 = EDGE_LOOP ( 'NONE', ( #6245, #28296 ) ) ;
#6760 = CARTESIAN_POINT ( 'NONE',  ( 17.99999662536861678, -86.60254037844400443, -5.000000000000000000 ) ) ;
#6761 = AXIS2_PLACEMENT_3D ( 'NONE', #28875, #17453, #3197 ) ;
#6762 = CARTESIAN_POINT ( 'NONE',  ( 0.000000000000000000, 0.000000000000000000, 0.000000000000000000 ) ) ;
#6763 = CARTESIAN_POINT ( 'NONE',  ( 7.999996625368656744, -69.28203230275519786, -5.000000000000000000 ) ) ;
#6764 = VERTEX_POINT ( 'NONE', #16166 ) ;
#6765 = ORIENTED_EDGE ( 'NONE', *, *, #2045, .F. ) ;
#6766 = ADVANCED_FACE ( 'NONE', ( #31142 ), #8079, .F. ) ;
#6767 = CARTESIAN_POINT ( 'NONE',  ( -62.00000337463107769, -34.64101615137762025, 17.49999999999999645 ) ) ;
#6768 = ORIENTED_EDGE ( 'NONE', *, *, #6392, .F. ) ;
#6769 = DIRECTION ( 'NONE',  ( -0.8660254037844381525, 0.5000000000000009992, 0.000000000000000000 ) ) ;
#6770 = FACE_BOUND ( 'NONE', #16614, .T. ) ;
#6771 = ADVANCED_FACE ( 'NONE', ( #10518 ), #16888, .F. ) ;
#6772 = CARTESIAN_POINT ( 'NONE',  ( 44.99999662536849598, 60.62177826491077326, -9.999999999999998224 ) ) ;
#6773 = DIRECTION ( 'NONE',  ( 1.000000000000000000, 0.000000000000000000, 0.000000000000000000 ) ) ;
#6774 = PLANE ( 'NONE',  #31472 ) ;
#6775 = VERTEX_POINT ( 'NONE', #33597 ) ;
#6776 = CARTESIAN_POINT ( 'NONE',  ( -78.00000337463094979, -17.32050807568882078, -9.999999999999998224 ) ) ;
#6777 = CARTESIAN_POINT ( 'NONE',  ( -40.00000337463113453, -69.28203230275519786, -9.999999999999998224 ) ) ;
#6778 = EDGE_CURVE ( 'NONE', #36669, #16909, #5403, .T. ) ;
#6779 = EDGE_LOOP ( 'NONE', ( #5499, #23508 ) ) ;
#6780 =( REPRESENTATION_RELATIONSHIP ('NONE','NONE', #15268, #35440 ) REPRESENTATION_RELATIONSHIP_WITH_TRANSFORMATION ( #13603 )SHAPE_REPRESENTATION_RELATIONSHIP( ) );
#6781 = CARTESIAN_POINT ( 'NONE',  ( -4.279621169095561228, 62.97617850287782915, -4.999999999999997335 ) ) ;
#6782 = CARTESIAN_POINT ( 'NONE',  ( -44.13139720814381661, 27.50000000000055422, -10.00000000000000178 ) ) ;
#6783 = AXIS2_PLACEMENT_3D ( 'NONE', #20130, #5696, #14674 ) ;
#6784 = DIRECTION ( 'NONE',  ( 0.000000000000000000, 0.000000000000000000, 1.000000000000000000 ) ) ;
#6785 = ORIENTED_EDGE ( 'NONE', *, *, #29637, .F. ) ;
#6786 = CIRCLE ( 'NONE', #16384, 2.000000000000001776 ) ;
#6787 = ORIENTED_EDGE ( 'NONE', *, *, #15522, .T. ) ;
#6788 = LINE ( 'NONE', #430, #11150 ) ;
#6789 = EDGE_CURVE ( 'NONE', #34315, #25502, #5284, .T. ) ;
#6790 = CARTESIAN_POINT ( 'NONE',  ( 79.99999662536832545, -17.32050807568879591, -9.999999999999998224 ) ) ;
#6791 = DIRECTION ( 'NONE',  ( 0.000000000000000000, 0.000000000000000000, 1.000000000000000000 ) ) ;
#6792 = ORIENTED_EDGE ( 'NONE', *, *, #16782, .F. ) ;
#6793 = VERTEX_POINT ( 'NONE', #24610 ) ;
#6794 = ORIENTED_EDGE ( 'NONE', *, *, #30284, .F. ) ;
#6795 = COLOUR_RGB ( '', 0.08235294, 0.09019608, 0.10196078) ;
#6796 = CARTESIAN_POINT ( 'NONE',  ( -27.78182860042817026, -56.67878100130359087, -4.999999999999997335 ) ) ;
#6797 = AXIS2_PLACEMENT_3D ( 'NONE', #5137, #19031, #16219 ) ;
#6798 = ORIENTED_EDGE ( 'NONE', *, *, #22160, .F. ) ;
#6799 = VERTEX_POINT ( 'NONE', #4906 ) ;
#6800 = CYLINDRICAL_SURFACE ( 'NONE', #2234, 2.000000000000000000 ) ;
#6801 = VERTEX_POINT ( 'NONE', #2462 ) ;
#6802 = AXIS2_PLACEMENT_3D ( 'NONE', #6485, #24269, #664 ) ;
#6803 = ORIENTED_EDGE ( 'NONE', *, *, #33121, .F. ) ;
#6804 = ADVANCED_FACE ( 'NONE', ( #36040 ), #10332, .F. ) ;
#6805 = DIRECTION ( 'NONE',  ( -0.000000000000000000, -0.000000000000000000, 1.000000000000000000 ) ) ;
#6806 = ADVANCED_FACE ( 'NONE', ( #30398 ), #1902, .T. ) ;
#6807 = FACE_OUTER_BOUND ( 'NONE', #29528, .T. ) ;
#6808 = ORIENTED_EDGE ( 'NONE', *, *, #27193, .F. ) ;
#6809 = ORIENTED_EDGE ( 'NONE', *, *, #8541, .F. ) ;
#6810 = CARTESIAN_POINT ( 'NONE',  ( 66.99999662536839651, -60.62177826491080168, -9.999999999999998224 ) ) ;
#6811 = DIRECTION ( 'NONE',  ( 1.000000000000000000, 0.000000000000000000, 0.000000000000000000 ) ) ;
#6812 = EDGE_CURVE ( 'NONE', #6228, #19610, #7900, .T. ) ;
#6813 = FACE_OUTER_BOUND ( 'NONE', #132, .T. ) ;
#6814 = CARTESIAN_POINT ( 'NONE',  ( 12.99999662536863632, -77.94228634059960825, 12.50000000000000000 ) ) ;
#6815 = CIRCLE ( 'NONE', #8027, 8.500000000000007105 ) ;
#6816 = ORIENTED_EDGE ( 'NONE', *, *, #35793, .T. ) ;
#6817 = DIRECTION ( 'NONE',  ( 0.000000000000000000, 0.000000000000000000, 1.000000000000000000 ) ) ;
#6818 = DIRECTION ( 'NONE',  ( 0.000000000000000000, 0.000000000000000000, 1.000000000000000000 ) ) ;
#6819 = VERTEX_POINT ( 'NONE', #13710 ) ;
#6820 = CARTESIAN_POINT ( 'NONE',  ( -60.00000337463107059, -34.64101615137762025, -9.999999999999998224 ) ) ;
#6821 = EDGE_CURVE ( 'NONE', #12416, #22484, #25166, .T. ) ;
#6822 = DIRECTION ( 'NONE',  ( 0.000000000000000000, 0.000000000000000000, 1.000000000000000000 ) ) ;
#6823 = DIRECTION ( 'NONE',  ( -1.000000000000000000, -0.000000000000000000, -0.000000000000000000 ) ) ;
#6824 = CARTESIAN_POINT ( 'NONE',  ( 39.99999662536853151, 69.28203230275518365, 17.49999999999999645 ) ) ;
#6825 = CIRCLE ( 'NONE', #21817, 2.000000000000001776 ) ;
#6826 = DIRECTION ( 'NONE',  ( 0.000000000000000000, 0.000000000000000000, 1.000000000000000000 ) ) ;
#6827 = EDGE_CURVE ( 'NONE', #5822, #1919, #2989, .T. ) ;
#6828 =( GEOMETRIC_REPRESENTATION_CONTEXT ( 3 ) GLOBAL_UNCERTAINTY_ASSIGNED_CONTEXT ( ( #5804 ) ) GLOBAL_UNIT_ASSIGNED_CONTEXT ( ( #29293, #26475, #3783 ) ) REPRESENTATION_CONTEXT ( 'NONE', 'WORKASPACE' ) );
#6829 = CARTESIAN_POINT ( 'NONE',  ( 74.99999662536836809, 43.30127018922198801, 17.49999999999999645 ) ) ;
#6830 = ORIENTED_EDGE ( 'NONE', *, *, #34904, .T. ) ;
#6831 = CARTESIAN_POINT ( 'NONE',  ( -95.00000000000000000, 0.000000000000000000, 17.49999999999999645 ) ) ;
#6832 = DIRECTION ( 'NONE',  ( 1.000000000000000000, 0.000000000000000000, 0.000000000000000000 ) ) ;
#6833 = CARTESIAN_POINT ( 'NONE',  ( 77.99999662536833966, 17.32050807568879236, -9.999999999999998224 ) ) ;
#6834 = ORIENTED_EDGE ( 'NONE', *, *, #28434, .T. ) ;
#6835 =( BOUNDED_CURVE ( )  B_SPLINE_CURVE ( 3, ( #21877, #16092, #24328, #1999 ),
 .UNSPECIFIED., .F., .F. ) 
 B_SPLINE_CURVE_WITH_KNOTS ( ( 4, 4 ),
 ( 3.141592653589793116, 4.712388980384689674 ),
 .UNSPECIFIED. ) 
 CURVE ( )  GEOMETRIC_REPRESENTATION_ITEM ( )  RATIONAL_B_SPLINE_CURVE ( ( 1.000000000000000000, 0.8047378541243649375, 0.8047378541243649375, 1.000000000000000000 ) ) 
 REPRESENTATION_ITEM ( '' )  );
#6836 = VERTEX_POINT ( 'NONE', #2275 ) ;
#6837 = ORIENTED_EDGE ( 'NONE', *, *, #2091, .T. ) ;
#6838 = DIRECTION ( 'NONE',  ( 0.000000000000000000, 0.000000000000000000, 1.000000000000000000 ) ) ;
#6839 = DIRECTION ( 'NONE',  ( 1.000000000000000000, 0.000000000000000000, 0.000000000000000000 ) ) ;
#6840 = CARTESIAN_POINT ( 'NONE',  ( -33.00000337463116296, 60.62177826491077326, -9.999999999999998224 ) ) ;
#6841 = CIRCLE ( 'NONE', #11616, 8.500000000000007105 ) ;
#6842 = DIRECTION ( 'NONE',  ( 1.000000000000000000, 0.000000000000000000, 0.000000000000000000 ) ) ;
#6843 = EDGE_CURVE ( 'NONE', #4052, #27516, #33770, .T. ) ;
#6844 = DIRECTION ( 'NONE',  ( 1.000000000000000000, 0.000000000000000000, 0.000000000000000000 ) ) ;
#6845 = ORIENTED_EDGE ( 'NONE', *, *, #6854, .F. ) ;
#6846 = CYLINDRICAL_SURFACE ( 'NONE', #19762, 30.00000000000001421 ) ;
#6847 = ORIENTED_EDGE ( 'NONE', *, *, #33150, .F. ) ;
#6848 = FACE_BOUND ( 'NONE', #997, .T. ) ;
#6849 = EDGE_CURVE ( 'NONE', #691, #25535, #19775, .T. ) ;
#6850 = AXIS2_PLACEMENT_3D ( 'NONE', #21539, #30140, #32972 ) ;
#6851 = DIRECTION ( 'NONE',  ( -1.000000000000000000, 0.000000000000000000, 0.000000000000000000 ) ) ;
#6852 = CYLINDRICAL_SURFACE ( 'NONE', #1774, 2.000000000000001776 ) ;
#6853 = AXIS2_PLACEMENT_3D ( 'NONE', #1866, #24743, #30559 ) ;
#6854 = EDGE_CURVE ( 'NONE', #6733, #2698, #32335, .T. ) ;
#6855 = CARTESIAN_POINT ( 'NONE',  ( 41.99999662536853151, -69.28203230275519786, -9.999999999999998224 ) ) ;
#6856 = EDGE_CURVE ( 'NONE', #31054, #29609, #32308, .T. ) ;
#6857 = EDGE_LOOP ( 'NONE', ( #21201, #21810 ) ) ;
#6858 = DIRECTION ( 'NONE',  ( 0.000000000000000000, 0.000000000000000000, 1.000000000000000000 ) ) ;
#6859 = MANIFOLD_SOLID_BREP ( 'Hex', #19594 ) ;
#6860 = DIRECTION ( 'NONE',  ( 0.000000000000000000, 0.000000000000000000, 1.000000000000000000 ) ) ;
#6861 = DIRECTION ( 'NONE',  ( 0.8660254037844360431, 0.5000000000000045519, 0.000000000000000000 ) ) ;
#6862 = CIRCLE ( 'NONE', #24866, 2.000000000000001776 ) ;
#6863 = DIRECTION ( 'NONE',  ( 3.491481338843135327E-15, 1.000000000000000000, 0.000000000000000000 ) ) ;
#6864 = CARTESIAN_POINT ( 'NONE',  ( 5.000000000000000000, 2.886751345948134428, -2.080000000000000071 ) ) ;
#6865 = ORIENTED_EDGE ( 'NONE', *, *, #29588, .T. ) ;
#6866 = CYLINDRICAL_SURFACE ( 'NONE', #25027, 2.000000000000001776 ) ;
#6867 = VECTOR ( 'NONE', #28691, 1000.000000000000000 ) ;
#6868 = DIRECTION ( 'NONE',  ( 1.000000000000000000, 0.000000000000000000, 0.000000000000000000 ) ) ;
#6869 = CARTESIAN_POINT ( 'NONE',  ( -70.00000337463102085, -51.96152422706641971, 12.50000000000000000 ) ) ;
#6870 = ORIENTED_EDGE ( 'NONE', *, *, #21361, .F. ) ;
#6871 = AXIS2_PLACEMENT_3D ( 'NONE', #26072, #8829, #6030 ) ;
#6872 = EDGE_LOOP ( 'NONE', ( #6196, #10026 ) ) ;
#6873 = EDGE_CURVE ( 'NONE', #11785, #11646, #22180, .T. ) ;
#6874 = VERTEX_POINT ( 'NONE', #31839 ) ;
#6875 = CARTESIAN_POINT ( 'NONE',  ( 42.99999662536850309, 77.94228634059959404, -5.000000000000000000 ) ) ;
#6876 = CARTESIAN_POINT ( 'NONE',  ( 34.99999662536855283, -77.94228634059960825, -9.999999999999998224 ) ) ;
#6877 = CIRCLE ( 'NONE', #12260, 2.000000000000001776 ) ;
#6878 = AXIS2_PLACEMENT_3D ( 'NONE', #16199, #19201, #30436 ) ;
#6879 = AXIS2_PLACEMENT_3D ( 'NONE', #34630, #16827, #19634 ) ;
#6880 = DIRECTION ( 'NONE',  ( -0.000000000000000000, -0.000000000000000000, 1.000000000000000000 ) ) ;
#6881 = DIRECTION ( 'NONE',  ( 0.000000000000000000, 0.000000000000000000, -1.000000000000000000 ) ) ;
#6882 = DIRECTION ( 'NONE',  ( 1.000000000000000000, 0.000000000000000000, 0.000000000000000000 ) ) ;
#6883 = DIRECTION ( 'NONE',  ( 0.000000000000000000, 0.000000000000000000, -1.000000000000000000 ) ) ;
#6884 = ORIENTED_EDGE ( 'NONE', *, *, #9666, .F. ) ;
#6885 = ORIENTED_EDGE ( 'NONE', *, *, #26374, .T. ) ;
#6886 = CARTESIAN_POINT ( 'NONE',  ( 26.99999662536859546, -77.94228634059960825, -9.999999999999998224 ) ) ;
#6887 = EDGE_CURVE ( 'NONE', #19642, #30141, #24596, .T. ) ;
#6888 = AXIS2_PLACEMENT_3D ( 'NONE', #8531, #22798, #22402 ) ;
#6889 = CARTESIAN_POINT ( 'NONE',  ( 0.000000000000000000, 0.000000000000000000, -5.000000000000000000 ) ) ;
#6890 = VERTEX_POINT ( 'NONE', #7 ) ;
#6891 = ADVANCED_FACE ( 'NONE', ( #19881 ), #29367, .T. ) ;
#6892 = AXIS2_PLACEMENT_3D ( 'NONE', #20911, #12450, #18084 ) ;
#6893 = FACE_OUTER_BOUND ( 'NONE', #14873, .T. ) ;
#6894 = VERTEX_POINT ( 'NONE', #32020 ) ;
#6895 = DIRECTION ( 'NONE',  ( 0.000000000000000000, 0.000000000000000000, 1.000000000000000000 ) ) ;
#6896 = VECTOR ( 'NONE', #28799, 1000.000000000000000 ) ;
#6897 = ADVANCED_FACE ( 'NONE', ( #22884 ), #6175, .F. ) ;
#6898 = CARTESIAN_POINT ( 'NONE',  ( -35.00000337463116296, 77.94228634059957983, 17.49999999999999645 ) ) ;
#6899 = ORIENTED_EDGE ( 'NONE', *, *, #31314, .F. ) ;
#6900 = ORIENTED_EDGE ( 'NONE', *, *, #9596, .F. ) ;
#6901 = EDGE_CURVE ( 'NONE', #15350, #35412, #8995, .T. ) ;
#6902 = CARTESIAN_POINT ( 'NONE',  ( 2.500000000000003109, -4.330127018922192761, -6.000000000000000000 ) ) ;
#6903 = ORIENTED_EDGE ( 'NONE', *, *, #29976, .F. ) ;
#6904 = CIRCLE ( 'NONE', #29048, 3.000000000000001332 ) ;
#6905 = ADVANCED_FACE ( 'NONE', ( #11262 ), #3018, .T. ) ;
#6906 = AXIS2_PLACEMENT_3D ( 'NONE', #13403, #25065, #5171 ) ;
#6907 = CARTESIAN_POINT ( 'NONE',  ( -4.598786737361987953, 3.118391931134617323, -0.4203182062997219970 ) ) ;
#6908 = CARTESIAN_POINT ( 'NONE',  ( -80.00000337463094979, -17.32050807568882078, -9.999999999999998224 ) ) ;
#6909 = DIRECTION ( 'NONE',  ( 0.000000000000000000, 0.000000000000000000, 1.000000000000000000 ) ) ;
#6910 = ORIENTED_EDGE ( 'NONE', *, *, #30612, .F. ) ;
#6911 = VERTEX_POINT ( 'NONE', #5626 ) ;
#6912 = EDGE_CURVE ( 'NONE', #33445, #18148, #26956, .T. ) ;
#6913 = ORIENTED_EDGE ( 'NONE', *, *, #18323, .F. ) ;
#6914 = EDGE_CURVE ( 'NONE', #9484, #32397, #16213, .T. ) ;
#6915 = ORIENTED_EDGE ( 'NONE', *, *, #28174, .T. ) ;
#6916 = ORIENTED_EDGE ( 'NONE', *, *, #28616, .T. ) ;
#6917 = EDGE_CURVE ( 'NONE', #12472, #14042, #6619, .T. ) ;
#6918 = DIRECTION ( 'NONE',  ( 0.000000000000000000, 0.000000000000000000, -1.000000000000000000 ) ) ;
#6919 = ADVANCED_FACE ( 'NONE', ( #9004 ), #29985, .F. ) ;
#6920 = DIRECTION ( 'NONE',  ( 0.000000000000000000, 0.000000000000000000, 1.000000000000000000 ) ) ;
#6921 = ORIENTED_EDGE ( 'NONE', *, *, #9396, .F. ) ;
#6922 = CIRCLE ( 'NONE', #6300, 2.000000000000001776 ) ;
#6923 = DIRECTION ( 'NONE',  ( -0.000000000000000000, -0.000000000000000000, 1.000000000000000000 ) ) ;
#6924 = CARTESIAN_POINT ( 'NONE',  ( 106.8646861230860878, 42.81779240327628600, 32.50000000000000000 ) ) ;
#6925 = AXIS2_PLACEMENT_3D ( 'NONE', #1082, #21519, #32566 ) ;
#6926 = DIRECTION ( 'NONE',  ( 0.000000000000000000, 0.000000000000000000, 1.000000000000000000 ) ) ;
#6927 = AXIS2_PLACEMENT_3D ( 'NONE', #1360, #3635, #35139 ) ;
#6928 = ORIENTED_EDGE ( 'NONE', *, *, #4058, .F. ) ;
#6929 = VECTOR ( 'NONE', #18494, 1000.000000000000000 ) ;
#6930 = DIRECTION ( 'NONE',  ( 1.000000000000000000, 0.000000000000000000, 0.000000000000000000 ) ) ;
#6931 = CIRCLE ( 'NONE', #36858, 33.00000000000001421 ) ;
#6932 = FACE_OUTER_BOUND ( 'NONE', #34477, .T. ) ;
#6933 = CARTESIAN_POINT ( 'NONE',  ( 5.750000000000000000, 89.94802294027094547, -24.99999999999999645 ) ) ;
#6934 = ORIENTED_EDGE ( 'NONE', *, *, #683, .T. ) ;
#6935 = DIRECTION ( 'NONE',  ( -1.000000000000000000, 0.000000000000000000, 0.000000000000000000 ) ) ;
#6936 = DIRECTION ( 'NONE',  ( 0.000000000000000000, 0.000000000000000000, 1.000000000000000000 ) ) ;
#6937 = ORIENTED_EDGE ( 'NONE', *, *, #5724, .T. ) ;
#6938 = EDGE_LOOP ( 'NONE', ( #4475, #19535, #15637, #7352 ) ) ;
#6939 = DIRECTION ( 'NONE',  ( -1.000000000000000000, 0.000000000000000000, 0.000000000000000000 ) ) ;
#6940 = LINE ( 'NONE', #18387, #7954 ) ;
#6941 = CARTESIAN_POINT ( 'NONE',  ( 51.13139720814400846, -27.50000000000022737, -5.000000000000000888 ) ) ;
#6942 = DIRECTION ( 'NONE',  ( 0.000000000000000000, 0.000000000000000000, 1.000000000000000000 ) ) ;
#6943 = ORIENTED_EDGE ( 'NONE', *, *, #33031, .T. ) ;
#6944 = AXIS2_PLACEMENT_3D ( 'NONE', #23706, #14527, #26152 ) ;
#6945 = CARTESIAN_POINT ( 'NONE',  ( -56.67878100130369035, 27.78182860042797131, -4.999999999999997335 ) ) ;
#6946 = FACE_OUTER_BOUND ( 'NONE', #26056, .T. ) ;
#6947 = AXIS2_PLACEMENT_3D ( 'NONE', #29893, #27453, #30248 ) ;
#6948 = VERTEX_POINT ( 'NONE', #23810 ) ;
#6949 = AXIS2_PLACEMENT_3D ( 'NONE', #18784, #36045, #13330 ) ;
#6950 = PRESENTATION_LAYER_ASSIGNMENT (  '', '', ( #30992 ) ) ;
#6951 = VERTEX_POINT ( 'NONE', #35817 ) ;
#6952 = CIRCLE ( 'NONE', #5783, 2.000000000000001776 ) ;
#6953 = AXIS2_PLACEMENT_3D ( 'NONE', #11947, #26395, #26209 ) ;
#6954 = DIRECTION ( 'NONE',  ( 0.000000000000000000, 0.000000000000000000, 1.000000000000000000 ) ) ;
#6955 = VECTOR ( 'NONE', #8506, 1000.000000000000000 ) ;
#6956 = DIRECTION ( 'NONE',  ( 1.000000000000000000, 0.000000000000000000, 0.000000000000000000 ) ) ;
#6957 = AXIS2_PLACEMENT_3D ( 'NONE', #28641, #5971, #2972 ) ;
#6958 = DIRECTION ( 'NONE',  ( 0.000000000000000000, 0.000000000000000000, 1.000000000000000000 ) ) ;
#6959 = ORIENTED_EDGE ( 'NONE', *, *, #34953, .F. ) ;
#6960 = ORIENTED_EDGE ( 'NONE', *, *, #15972, .T. ) ;
#6961 = VECTOR ( 'NONE', #3089, 1000.000000000000000 ) ;
#6962 = EDGE_LOOP ( 'NONE', ( #15021, #18285 ) ) ;
#6963 = DIRECTION ( 'NONE',  ( 0.000000000000000000, 0.000000000000000000, 1.000000000000000000 ) ) ;
#6964 = EDGE_CURVE ( 'NONE', #36953, #8381, #1296, .T. ) ;
#6965 = FACE_BOUND ( 'NONE', #4545, .T. ) ;
#6966 = DIRECTION ( 'NONE',  ( 0.000000000000000000, 0.000000000000000000, 1.000000000000000000 ) ) ;
#6967 = FACE_BOUND ( 'NONE', #12128, .T. ) ;
#6968 = DIRECTION ( 'NONE',  ( 0.000000000000000000, 0.000000000000000000, 1.000000000000000000 ) ) ;
#6969 = ORIENTED_EDGE ( 'NONE', *, *, #24907, .F. ) ;
#6970 = DIRECTION ( 'NONE',  ( 0.000000000000000000, 0.000000000000000000, 1.000000000000000000 ) ) ;
#6971 = VECTOR ( 'NONE', #3226, 1000.000000000000000 ) ;
#6972 = DIRECTION ( 'NONE',  ( 0.000000000000000000, 0.000000000000000000, 1.000000000000000000 ) ) ;
#6973 = VECTOR ( 'NONE', #176, 1000.000000000000000 ) ;
#6974 = DIRECTION ( 'NONE',  ( 0.000000000000000000, 0.000000000000000000, 1.000000000000000000 ) ) ;
#6975 = EDGE_LOOP ( 'NONE', ( #7279, #35921, #29209, #11623 ) ) ;
#6976 = CARTESIAN_POINT ( 'NONE',  ( 84.99999662536831124, -25.98076211353319565, -5.000000000000000000 ) ) ;
#6977 = PRODUCT_DEFINITION_FORMATION_WITH_SPECIFIED_SOURCE ( 'ANY', '', #8866, .NOT_KNOWN. ) ;
#6978 = DIRECTION ( 'NONE',  ( 0.000000000000000000, 0.000000000000000000, 1.000000000000000000 ) ) ;
#6979 = CYLINDRICAL_SURFACE ( 'NONE', #1821, 2.000000000000001776 ) ;
#6980 = AXIS2_PLACEMENT_3D ( 'NONE', #36073, #36628, #13919 ) ;
#6981 = CIRCLE ( 'NONE', #10602, 2.000000000000001776 ) ;
#6982 = ORIENTED_EDGE ( 'NONE', *, *, #554, .F. ) ;
#6983 = VECTOR ( 'NONE', #423, 999.9999999999998863 ) ;
#6984 = ORIENTED_EDGE ( 'NONE', *, *, #6856, .T. ) ;
#6985 = CIRCLE ( 'NONE', #32730, 2.000000000000001776 ) ;
#6986 = DIRECTION ( 'NONE',  ( 1.000000000000000000, 0.000000000000000000, 0.000000000000000000 ) ) ;
#6987 = DIRECTION ( 'NONE',  ( 0.000000000000000000, 0.000000000000000000, 1.000000000000000000 ) ) ;
#6988 = CARTESIAN_POINT ( 'NONE',  ( 0.000000000000000000, 0.000000000000000000, -5.000000000000000000 ) ) ;
#6989 = VERTEX_POINT ( 'NONE', #29790 ) ;
#6990 = ORIENTED_EDGE ( 'NONE', *, *, #15723, .T. ) ;
#6991 = ORIENTED_EDGE ( 'NONE', *, *, #14088, .T. ) ;
#6992 = ADVANCED_FACE ( 'NONE', ( #12544 ), #21167, .F. ) ;
#6993 = EDGE_CURVE ( 'NONE', #9603, #8407, #1119, .T. ) ;
#6994 = CIRCLE ( 'NONE', #18373, 33.00000000000001421 ) ;
#6995 = CARTESIAN_POINT ( 'NONE',  ( -5.999999999999985789, -149.8799519615616305, 32.50000000000000000 ) ) ;
#6996 = ORIENTED_EDGE ( 'NONE', *, *, #14817, .T. ) ;
#6997 = PRODUCT_DEFINITION ( 'UNKNOWN', '', #12966, #2443 ) ;
#6998 = ORIENTED_EDGE ( 'NONE', *, *, #29801, .F. ) ;
#6999 = CARTESIAN_POINT ( 'NONE',  ( 9.999996625368655856, -86.60254037844400443, -9.999999999999998224 ) ) ;
#7000 = ORIENTED_EDGE ( 'NONE', *, *, #14837, .F. ) ;
#7001 = AXIS2_PLACEMENT_3D ( 'NONE', #20642, #32073, #36039 ) ;
#7002 = ORIENTED_EDGE ( 'NONE', *, *, #4082, .T. ) ;
#7003 = EDGE_CURVE ( 'NONE', #1358, #15010, #15735, .T. ) ;
#7004 = FACE_OUTER_BOUND ( 'NONE', #27680, .T. ) ;
#7005 = AXIS2_PLACEMENT_3D ( 'NONE', #25879, #23256, #9007 ) ;
#7006 = CIRCLE ( 'NONE', #23177, 2.000000000000001776 ) ;
#7007 = DIRECTION ( 'NONE',  ( 1.000000000000000000, 0.000000000000000000, 0.000000000000000000 ) ) ;
#7008 = ORIENTED_EDGE ( 'NONE', *, *, #19898, .T. ) ;
#7009 = EDGE_LOOP ( 'NONE', ( #30750, #33999, #22185, #6072 ) ) ;
#7010 = DIRECTION ( 'NONE',  ( -0.000000000000000000, -0.000000000000000000, 1.000000000000000000 ) ) ;
#7011 = FACE_OUTER_BOUND ( 'NONE', #8488, .T. ) ;
#7012 = LINE ( 'NONE', #18459, #35741 ) ;
#7013 = VECTOR ( 'NONE', #6936, 1000.000000000000000 ) ;
#7014 = DIRECTION ( 'NONE',  ( -1.000000000000000000, 0.000000000000000000, 0.000000000000000000 ) ) ;
#7015 = CARTESIAN_POINT ( 'NONE',  ( 0.000000000000000000, 2.935248768560057453, -3.903127820947815962E-15 ) ) ;
#7016 = CIRCLE ( 'NONE', #31542, 30.00000000000001421 ) ;
#7017 = AXIS2_PLACEMENT_3D ( 'NONE', #4224, #24259, #35371 ) ;
#7018 = ORIENTED_EDGE ( 'NONE', *, *, #6613, .T. ) ;
#7019 = DIRECTION ( 'NONE',  ( 1.000000000000000000, 0.000000000000000000, 0.000000000000000000 ) ) ;
#7020 = ORIENTED_EDGE ( 'NONE', *, *, #3387, .T. ) ;
#7021 = ADVANCED_FACE ( 'NONE', ( #7300 ), #4125, .F. ) ;
#7022 = DIRECTION ( 'NONE',  ( 0.000000000000000000, 0.000000000000000000, 1.000000000000000000 ) ) ;
#7023 = CARTESIAN_POINT ( 'NONE',  ( -20.00000337463123756, -69.28203230275522628, 17.49999999999999645 ) ) ;
#7024 = CARTESIAN_POINT ( 'NONE',  ( -77.00000337463100664, -43.30127018922202353, -5.000000000000000000 ) ) ;
#7025 = VECTOR ( 'NONE', #20386, 1000.000000000000000 ) ;
#7026 = CARTESIAN_POINT ( 'NONE',  ( 74.99999662536835388, -43.30127018922199511, -9.999999999999998224 ) ) ;
#7027 = DIRECTION ( 'NONE',  ( 0.000000000000000000, 0.000000000000000000, 1.000000000000000000 ) ) ;
#7028 = CYLINDRICAL_SURFACE ( 'NONE', #26531, 2.000000000000000000 ) ;
#7029 = VERTEX_POINT ( 'NONE', #35265 ) ;
#7030 = CARTESIAN_POINT ( 'NONE',  ( -37.00000337463116296, 77.94228634059957983, -5.000000000000000000 ) ) ;
#7031 = CIRCLE ( 'NONE', #27981, 1.999999999999998224 ) ;
#7032 = DIRECTION ( 'NONE',  ( -1.000000000000000000, 0.000000000000000000, 0.000000000000000000 ) ) ;
#7033 = DIRECTION ( 'NONE',  ( 0.000000000000000000, 0.000000000000000000, 1.000000000000000000 ) ) ;
#7034 = CIRCLE ( 'NONE', #15439, 2.000000000000001776 ) ;
#7035 = ORIENTED_EDGE ( 'NONE', *, *, #33845, .T. ) ;
#7036 = VERTEX_POINT ( 'NONE', #12146 ) ;
#7037 = VERTEX_POINT ( 'NONE', #32597 ) ;
#7038 = AXIS2_PLACEMENT_3D ( 'NONE', #9829, #24092, #4231 ) ;
#7039 = EDGE_CURVE ( 'NONE', #29631, #3733, #3011, .T. ) ;
#7040 = DIRECTION ( 'NONE',  ( 1.000000000000000000, 0.000000000000000000, 0.000000000000000000 ) ) ;
#7041 = PLANE ( 'NONE',  #15816 ) ;
#7042 = CARTESIAN_POINT ( 'NONE',  ( 98.28784258493033121, 106.7731239591685437, 32.50000000000000000 ) ) ;
#7043 = ORIENTED_EDGE ( 'NONE', *, *, #23640, .F. ) ;
#7044 = COLOUR_RGB ( '', 0.66274510, 0.83137255, 0.94901961) ;
#7045 = AXIS2_PLACEMENT_3D ( 'NONE', #8425, #19853, #8590 ) ;
#7046 = CIRCLE ( 'NONE', #19628, 2.000000000000001776 ) ;
#7047 = DIRECTION ( 'NONE',  ( -0.000000000000000000, -0.000000000000000000, 1.000000000000000000 ) ) ;
#7048 = DIRECTION ( 'NONE',  ( 1.000000000000000000, 0.000000000000000000, 0.000000000000000000 ) ) ;
#7049 = ORIENTED_EDGE ( 'NONE', *, *, #21889, .F. ) ;
#7050 = LINE ( 'NONE', #18496, #22765 ) ;
#7051 = ADVANCED_FACE ( 'NONE', ( #18738 ), #12342, .T. ) ;
#7052 = ORIENTED_EDGE ( 'NONE', *, *, #1553, .F. ) ;
#7053 = FACE_BOUND ( 'NONE', #19723, .T. ) ;
#7054 = CIRCLE ( 'NONE', #29818, 3.499999999999996003 ) ;
#7055 = EDGE_CURVE ( 'NONE', #6532, #24891, #5426, .T. ) ;
#7056 = CARTESIAN_POINT ( 'NONE',  ( 79.99999662536833966, 34.64101615137759183, -9.999999999999998224 ) ) ;
#7057 = DIRECTION ( 'NONE',  ( 1.000000000000000000, 0.000000000000000000, 0.000000000000000000 ) ) ;
#7058 = AXIS2_PLACEMENT_3D ( 'NONE', #1537, #18437, #26485 ) ;
#7059 = CARTESIAN_POINT ( 'NONE',  ( 101.7384897088143560, -110.2237710830540180, 32.50000000000000000 ) ) ;
#7060 = ORIENTED_EDGE ( 'NONE', *, *, #34814, .T. ) ;
#7061 = DIRECTION ( 'NONE',  ( 1.000000000000000000, 0.000000000000000000, 0.000000000000000000 ) ) ;
#7062 = AXIS2_PLACEMENT_3D ( 'NONE', #23969, #4274, #35417 ) ;
#7063 = CIRCLE ( 'NONE', #28015, 2.000000000000001776 ) ;
#7064 = AXIS2_PLACEMENT_3D ( 'NONE', #20387, #9123, #17751 ) ;
#7065 = DIRECTION ( 'NONE',  ( 1.000000000000000000, 0.000000000000000000, 0.000000000000000000 ) ) ;
#7066 = CIRCLE ( 'NONE', #8247, 2.000000000000001776 ) ;
#7067 = CARTESIAN_POINT ( 'NONE',  ( -98.28784258493107018, -106.7731239591678474, 32.50000000000000000 ) ) ;
#7068 = DIRECTION ( 'NONE',  ( 0.8660254037844413721, 0.4999999999999950595, 0.000000000000000000 ) ) ;
#7069 = VERTEX_POINT ( 'NONE', #32800 ) ;
#7070 = DIRECTION ( 'NONE',  ( 0.000000000000000000, 0.000000000000000000, 1.000000000000000000 ) ) ;
#7071 = CYLINDRICAL_SURFACE ( 'NONE', #28018, 3.500000000000003109 ) ;
#7072 = DIRECTION ( 'NONE',  ( -1.000000000000000000, 0.000000000000000000, 0.000000000000000000 ) ) ;
#7073 = AXIS2_PLACEMENT_3D ( 'NONE', #7929, #16557, #8111 ) ;
#7074 = EDGE_CURVE ( 'NONE', #14854, #18637, #16188, .T. ) ;
#7075 = EDGE_LOOP ( 'NONE', ( #11140, #9843, #14511, #36433 ) ) ;
#7076 = ORIENTED_EDGE ( 'NONE', *, *, #11586, .T. ) ;
#7077 = DIRECTION ( 'NONE',  ( 1.000000000000000000, 0.000000000000000000, 0.000000000000000000 ) ) ;
#7078 = DIRECTION ( 'NONE',  ( -0.8660254037844449249, -0.4999999999999888423, 0.000000000000000000 ) ) ;
#7079 = ADVANCED_FACE ( 'NONE', ( #20797 ), #32233, .F. ) ;
#7080 = CARTESIAN_POINT ( 'NONE',  ( -75.00000337463097821, 43.30127018922197379, -5.000000000000000000 ) ) ;
#7081 = EDGE_LOOP ( 'NONE', ( #36238, #3760 ) ) ;
#7082 = AXIS2_PLACEMENT_3D ( 'NONE', #13915, #45, #22357 ) ;
#7083 = EDGE_CURVE ( 'NONE', #12432, #21828, #31166, .T. ) ;
#7084 = DIRECTION ( 'NONE',  ( 0.5000000000000039968, 0.8660254037844363761, 0.000000000000000000 ) ) ;
#7085 = CARTESIAN_POINT ( 'NONE',  ( 44.99999662536849598, 60.62177826491077326, -9.999999999999998224 ) ) ;
#7086 = AXIS2_PLACEMENT_3D ( 'NONE', #29709, #21479, #35730 ) ;
#7087 = DIRECTION ( 'NONE',  ( 0.000000000000000000, 0.000000000000000000, 1.000000000000000000 ) ) ;
#7088 = EDGE_LOOP ( 'NONE', ( #2847, #15188 ) ) ;
#7089 = VECTOR ( 'NONE', #13971, 1000.000000000000114 ) ;
#7090 = ORIENTED_EDGE ( 'NONE', *, *, #26571, .F. ) ;
#7091 = DIRECTION ( 'NONE',  ( 1.000000000000000000, 0.000000000000000000, 0.000000000000000000 ) ) ;
#7092 = CIRCLE ( 'NONE', #25652, 2.000000000000001776 ) ;
#7093 = CARTESIAN_POINT ( 'NONE',  ( 35.19434990244975126, -52.39915983220758022, 12.49999999999999822 ) ) ;
#7094 = ORIENTED_EDGE ( 'NONE', *, *, #36493, .F. ) ;
#7095 = CARTESIAN_POINT ( 'NONE',  ( -47.63139720814380951, 27.50000000000055422, -15.00000000000000000 ) ) ;
#7096 = ORIENTED_EDGE ( 'NONE', *, *, #4607, .F. ) ;
#7097 = CARTESIAN_POINT ( 'NONE',  ( 66.99999662536841072, -25.98076211353320275, -9.999999999999998224 ) ) ;
#7098 = AXIS2_PLACEMENT_3D ( 'NONE', #8303, #25895, #34340 ) ;
#7099 = VECTOR ( 'NONE', #5498, 1000.000000000000000 ) ;
#7100 = EDGE_CURVE ( 'NONE', #17212, #20372, #4223, .T. ) ;
#7101 = FACE_BOUND ( 'NONE', #31418, .T. ) ;
#7102 = EDGE_LOOP ( 'NONE', ( #4126, #19256, #33852, #25643 ) ) ;
#7103 = ORIENTED_EDGE ( 'NONE', *, *, #5186, .F. ) ;
#7104 = CARTESIAN_POINT ( 'NONE',  ( 12.99999662536863632, -77.94228634059960825, -9.999999999999998224 ) ) ;
#7105 = ORIENTED_EDGE ( 'NONE', *, *, #20342, .F. ) ;
#7106 = AXIS2_PLACEMENT_3D ( 'NONE', #2217, #22279, #13657 ) ;
#7107 = PLANE ( 'NONE',  #25433 ) ;
#7108 = CIRCLE ( 'NONE', #2326, 2.000000000000000000 ) ;
#7109 = DIRECTION ( 'NONE',  ( 0.000000000000000000, 0.000000000000000000, -1.000000000000000000 ) ) ;
#7110 = DIRECTION ( 'NONE',  ( 1.000000000000000000, 0.000000000000000000, 0.000000000000000000 ) ) ;
#7111 = VERTEX_POINT ( 'NONE', #26604 ) ;
#7112 = CARTESIAN_POINT ( 'NONE',  ( 66.00000000000000000, 0.000000000000000000, 2.445500000000000007 ) ) ;
#7113 = AXIS2_PLACEMENT_3D ( 'NONE', #10205, #26889, #9644 ) ;
#7114 = ORIENTED_EDGE ( 'NONE', *, *, #22154, .T. ) ;
#7115 = ORIENTED_EDGE ( 'NONE', *, *, #3985, .F. ) ;
#7116 = ADVANCED_FACE ( 'NONE', ( #29595 ), #6563, .F. ) ;
#7117 = VECTOR ( 'NONE', #10301, 1000.000000000000000 ) ;
#7118 = ORIENTED_EDGE ( 'NONE', *, *, #29345, .T. ) ;
#7119 = CARTESIAN_POINT ( 'NONE',  ( -77.00000337463097821, -8.660254037844422825, -5.000000000000000000 ) ) ;
#7120 = AXIS2_PLACEMENT_3D ( 'NONE', #13389, #22582, #25227 ) ;
#7121 = DIRECTION ( 'NONE',  ( 0.000000000000000000, 0.000000000000000000, 1.000000000000000000 ) ) ;
#7122 = EDGE_CURVE ( 'NONE', #26515, #25741, #29419, .T. ) ;
#7123 = EDGE_LOOP ( 'NONE', ( #7096, #27423, #10961, #2693, #24769 ) ) ;
#7124 = CARTESIAN_POINT ( 'NONE',  ( -37.00000337463116296, 60.62177826491077326, -9.999999999999998224 ) ) ;
#7125 = DIRECTION ( 'NONE',  ( 0.000000000000000000, 0.000000000000000000, -1.000000000000000000 ) ) ;
#7126 = AXIS2_PLACEMENT_3D ( 'NONE', #5604, #2804, #22862 ) ;
#7127 = ORIENTED_EDGE ( 'NONE', *, *, #17358, .F. ) ;
#7128 = CARTESIAN_POINT ( 'NONE',  ( 4.999999999999999112, 2.886751345948125991, -5.700000000000000178 ) ) ;
#7129 = EDGE_CURVE ( 'NONE', #6217, #27465, #28750, .T. ) ;
#7130 = AXIS2_PLACEMENT_3D ( 'NONE', #3770, #7472, #34914 ) ;
#7131 = FACE_OUTER_BOUND ( 'NONE', #34149, .T. ) ;
#7132 = FACE_OUTER_BOUND ( 'NONE', #22221, .T. ) ;
#7133 = CARTESIAN_POINT ( 'NONE',  ( 104.0323809747665109, -35.06837973811266096, 32.50000000000000000 ) ) ;
#7134 = ADVANCED_FACE ( 'NONE', ( #5031 ), #33560, .T. ) ;
#7135 = DIRECTION ( 'NONE',  ( 1.000000000000000000, 0.000000000000000000, 0.000000000000000000 ) ) ;
#7136 = ADVANCED_FACE ( 'NONE', ( #27357 ), #13285, .F. ) ;
#7137 = CARTESIAN_POINT ( 'NONE',  ( -0.8179331680533066251, -5.301268757141566645, -5.826062401966622062 ) ) ;
#7138 = ORIENTED_EDGE ( 'NONE', *, *, #28796, .F. ) ;
#7139 = ORIENTED_EDGE ( 'NONE', *, *, #14019, .T. ) ;
#7140 = CARTESIAN_POINT ( 'NONE',  ( -58.00000337463107059, -34.64101615137762025, -9.999999999999998224 ) ) ;
#7141 = CARTESIAN_POINT ( 'NONE',  ( -53.00000337463109190, -60.62177826491083010, -5.000000000000000000 ) ) ;
#7142 = DIRECTION ( 'NONE',  ( -1.000000000000000000, 0.000000000000000000, 0.000000000000000000 ) ) ;
#7143 = CARTESIAN_POINT ( 'NONE',  ( 37.50000000000000000, -103.4105893997321743, 27.50000000000000000 ) ) ;
#7144 = EDGE_LOOP ( 'NONE', ( #8181, #6696 ) ) ;
#7145 = EDGE_CURVE ( 'NONE', #4037, #25006, #33563, .T. ) ;
#7146 = DIRECTION ( 'NONE',  ( 1.000000000000000000, 0.000000000000000000, 0.000000000000000000 ) ) ;
#7147 = EDGE_CURVE ( 'NONE', #34111, #35831, #2426, .T. ) ;
#7148 = DIRECTION ( 'NONE',  ( 1.000000000000000000, 0.000000000000000000, 0.000000000000000000 ) ) ;
#7149 = EDGE_CURVE ( 'NONE', #9158, #10452, #28168, .T. ) ;
#7150 = ORIENTED_EDGE ( 'NONE', *, *, #31656, .F. ) ;
#7151 = ADVANCED_FACE ( 'NONE', ( #19469 ), #27901, .F. ) ;
#7152 = CIRCLE ( 'NONE', #16151, 95.00000000000000000 ) ;
#7153 = ADVANCED_FACE ( 'NONE', ( #13665 ), #30896, .F. ) ;
#7154 = FACE_OUTER_BOUND ( 'NONE', #906, .T. ) ;
#7155 = ORIENTED_EDGE ( 'NONE', *, *, #28916, .T. ) ;
#7156 = CIRCLE ( 'NONE', #10154, 2.000000000000001776 ) ;
#7157 = DIRECTION ( 'NONE',  ( 1.000000000000000000, 0.000000000000000000, 0.000000000000000000 ) ) ;
#7158 = DIRECTION ( 'NONE',  ( 0.000000000000000000, 0.000000000000000000, 1.000000000000000000 ) ) ;
#7159 = AXIS2_PLACEMENT_3D ( 'NONE', #5210, #1656, #27882 ) ;
#7160 = CARTESIAN_POINT ( 'NONE',  ( 2.618768541235299896, 4.261555969668734178, -0.5078976954042870862 ) ) ;
#7161 = VERTEX_POINT ( 'NONE', #2423 ) ;
#7162 = CIRCLE ( 'NONE', #8944, 27.00000000000001421 ) ;
#7163 = ORIENTED_EDGE ( 'NONE', *, *, #33023, .T. ) ;
#7164 = B_SPLINE_CURVE_WITH_KNOTS ( 'NONE', 3,
 ( #21757, #33192, #27585, #7513, #13318, #10161, #18963, #15769, #7334, #7160, #21398, #9765, #18199, #3961, #21199, #32841, #18599, #4160, #15404, #24405 ),
 .UNSPECIFIED., .F., .F.,
 ( 4, 2, 2, 2, 2, 2, 2, 2, 2, 4 ),
 ( 2.781148923614798380E-07, 0.0008372784139766645825, 0.001674278713060967658, 0.002511279012145270842, 0.003348279311229572942, 0.003766779460771723775, 0.004185279610313873307, 0.005022279909398174105, 0.005859280208482472302, 0.006696280507566771366 ),
 .UNSPECIFIED. ) ;
#7165 = ORIENTED_EDGE ( 'NONE', *, *, #31999, .F. ) ;
#7166 = LINE ( 'NONE', #18415, #27956 ) ;
#7167 = VECTOR ( 'NONE', #305, 1000.000000000000000 ) ;
#7168 = DIRECTION ( 'NONE',  ( 1.000000000000000000, 0.000000000000000000, 0.000000000000000000 ) ) ;
#7169 = VECTOR ( 'NONE', #6308, 1000.000000000000000 ) ;
#7170 = CARTESIAN_POINT ( 'NONE',  ( -55.00000337463110611, -43.30127018922202353, -9.999999999999998224 ) ) ;
#7171 = CARTESIAN_POINT ( 'NONE',  ( -83.00000337463092137, -8.660254037844422825, -5.000000000000000000 ) ) ;
#7172 = CARTESIAN_POINT ( 'NONE',  ( 7.041719095097282852E-16, 87.07302294027100231, -20.02035392823936633 ) ) ;
#7173 = ORIENTED_EDGE ( 'NONE', *, *, #18340, .T. ) ;
#7174 = DIRECTION ( 'NONE',  ( -0.000000000000000000, 0.000000000000000000, -1.000000000000000000 ) ) ;
#7175 = FACE_OUTER_BOUND ( 'NONE', #25270, .T. ) ;
#7176 = CARTESIAN_POINT ( 'NONE',  ( -20.00000337463124112, 69.28203230275516944, 17.49999999999999645 ) ) ;
#7177 = ORIENTED_EDGE ( 'NONE', *, *, #31039, .F. ) ;
#7178 = DIRECTION ( 'NONE',  ( 0.000000000000000000, 0.000000000000000000, 1.000000000000000000 ) ) ;
#7179 = FACE_OUTER_BOUND ( 'NONE', #2484, .T. ) ;
#7180 = AXIS2_PLACEMENT_3D ( 'NONE', #244, #9064, #6077 ) ;
#7181 = ORIENTED_EDGE ( 'NONE', *, *, #16279, .T. ) ;
#7182 = VERTEX_POINT ( 'NONE', #22286 ) ;
#7183 = CIRCLE ( 'NONE', #28131, 45.00000000000000000 ) ;
#7184 = DIRECTION ( 'NONE',  ( 0.000000000000000000, 0.000000000000000000, 1.000000000000000000 ) ) ;
#7185 = VECTOR ( 'NONE', #21607, 1000.000000000000000 ) ;
#7186 = DIRECTION ( 'NONE',  ( 1.000000000000000000, 0.000000000000000000, 0.000000000000000000 ) ) ;
#7187 = DIRECTION ( 'NONE',  ( 0.000000000000000000, 0.000000000000000000, -1.000000000000000000 ) ) ;
#7188 = EDGE_LOOP ( 'NONE', ( #25721, #32984, #36736, #7326, #1228 ) ) ;
#7189 = ORIENTED_EDGE ( 'NONE', *, *, #34064, .T. ) ;
#7190 = AXIS2_PLACEMENT_3D ( 'NONE', #30625, #2675, #25024 ) ;
#7191 = ORIENTED_EDGE ( 'NONE', *, *, #22663, .T. ) ;
#7192 = EDGE_CURVE ( 'NONE', #2273, #15837, #34702, .T. ) ;
#7193 = CARTESIAN_POINT ( 'NONE',  ( 39.99999662536853151, -69.28203230275519786, -9.999999999999998224 ) ) ;
#7194 = CIRCLE ( 'NONE', #4201, 2.000000000000001776 ) ;
#7195 = ORIENTED_EDGE ( 'NONE', *, *, #31020, .F. ) ;
#7196 = EDGE_CURVE ( 'NONE', #6819, #9156, #26992, .T. ) ;
#7197 = ORIENTED_EDGE ( 'NONE', *, *, #23872, .F. ) ;
#7198 = VECTOR ( 'NONE', #33107, 1000.000000000000000 ) ;
#7199 = CARTESIAN_POINT ( 'NONE',  ( 39.99999662536853151, -69.28203230275519786, 12.50000000000000000 ) ) ;
#7200 = ORIENTED_EDGE ( 'NONE', *, *, #14594, .F. ) ;
#7201 = VERTEX_POINT ( 'NONE', #36719 ) ;
#7202 = CARTESIAN_POINT ( 'NONE',  ( -40.00000337463113453, -69.28203230275519786, -9.999999999999998224 ) ) ;
#7203 = DIRECTION ( 'NONE',  ( 0.000000000000000000, 0.000000000000000000, 1.000000000000000000 ) ) ;
#7204 = ORIENTED_EDGE ( 'NONE', *, *, #26011, .T. ) ;
#7205 = ORIENTED_EDGE ( 'NONE', *, *, #14865, .F. ) ;
#7206 = CARTESIAN_POINT ( 'NONE',  ( -6.000000000000000000, 149.8799519615616305, 27.50000000000000000 ) ) ;
#7207 = CYLINDRICAL_SURFACE ( 'NONE', #3396, 24.99999999999999289 ) ;
#7208 = CIRCLE ( 'NONE', #2419, 2.000000000000000000 ) ;
#7209 = CARTESIAN_POINT ( 'NONE',  ( -80.00000337463094979, -17.32050807568882078, 12.50000000000000000 ) ) ;
#7210 = DIRECTION ( 'NONE',  ( 1.000000000000000000, 0.000000000000000000, 0.000000000000000000 ) ) ;
#7211 = ORIENTED_EDGE ( 'NONE', *, *, #18731, .F. ) ;
#7212 = DIRECTION ( 'NONE',  ( 0.000000000000000000, 0.000000000000000000, 1.000000000000000000 ) ) ;
#7213 = EDGE_LOOP ( 'NONE', ( #31507, #20051, #23766, #26085 ) ) ;
#7214 = CIRCLE ( 'NONE', #34174, 2.000000000000001776 ) ;
#7215 = CARTESIAN_POINT ( 'NONE',  ( -83.00000337463092137, 25.98076211353317433, 17.49999999999999645 ) ) ;
#7216 = DIRECTION ( 'NONE',  ( -0.000000000000000000, -0.000000000000000000, -1.000000000000000000 ) ) ;
#7217 = AXIS2_PLACEMENT_3D ( 'NONE', #27713, #10853, #19128 ) ;
#7218 = CARTESIAN_POINT ( 'NONE',  ( 70.80619744048946984, -84.18124734178287838, 27.50000000000000000 ) ) ;
#7219 = DIRECTION ( 'NONE',  ( 1.000000000000000000, 0.000000000000000000, 0.000000000000000000 ) ) ;
#7220 = EDGE_CURVE ( 'NONE', #1919, #30886, #12517, .T. ) ;
#7221 = CARTESIAN_POINT ( 'NONE',  ( -59.13646009116099833, 70.47608876694653190, -4.999999999999997335 ) ) ;
#7222 = CARTESIAN_POINT ( 'NONE',  ( -33.99999999999945288, 58.88972745734214698, 12.49999999999999822 ) ) ;
#7223 = DIRECTION ( 'NONE',  ( -0.6439740589782688707, 0.7650473262243671080, 0.000000000000000000 ) ) ;
#7224 = EDGE_LOOP ( 'NONE', ( #21446, #20791 ) ) ;
#7225 = CARTESIAN_POINT ( 'NONE',  ( 14.99999662536863632, -77.94228634059960825, 17.49999999999999645 ) ) ;
#7226 = FACE_OUTER_BOUND ( 'NONE', #2706, .T. ) ;
#7227 = CARTESIAN_POINT ( 'NONE',  ( 74.99999662536836809, 25.98076211353319565, 17.49999999999999645 ) ) ;
#7228 = ORIENTED_EDGE ( 'NONE', *, *, #7798, .T. ) ;
#7229 = EDGE_LOOP ( 'NONE', ( #14601, #27687 ) ) ;
#7230 = VERTEX_POINT ( 'NONE', #16299 ) ;
#7231 = DIRECTION ( 'NONE',  ( 1.000000000000000000, 0.000000000000000000, 0.000000000000000000 ) ) ;
#7232 = LINE ( 'NONE', #35547, #12194 ) ;
#7233 = CARTESIAN_POINT ( 'NONE',  ( 71.99999662536839651, 34.64101615137758472, 17.49999999999999645 ) ) ;
#7234 = VERTEX_POINT ( 'NONE', #2229 ) ;
#7235 = CYLINDRICAL_SURFACE ( 'NONE', #22730, 2.000000000000001776 ) ;
#7236 = DIRECTION ( 'NONE',  ( 0.000000000000000000, 0.000000000000000000, 1.000000000000000000 ) ) ;
#7237 = EDGE_LOOP ( 'NONE', ( #22423, #7862, #12608, #30672 ) ) ;
#7238 = AXIS2_PLACEMENT_3D ( 'NONE', #34284, #31809, #17227 ) ;
#7239 = EDGE_CURVE ( 'NONE', #18905, #11624, #7674, .T. ) ;
#7240 = CARTESIAN_POINT ( 'NONE',  ( -63.00000337463106348, -60.62177826491083010, -9.999999999999998224 ) ) ;
#7241 = ORIENTED_EDGE ( 'NONE', *, *, #27783, .T. ) ;
#7242 = FACE_BOUND ( 'NONE', #19263, .T. ) ;
#7243 = LINE ( 'NONE', #18859, #12366 ) ;
#7244 = CYLINDRICAL_SURFACE ( 'NONE', #9556, 2.000000000000001776 ) ;
#7245 = CARTESIAN_POINT ( 'NONE',  ( -62.33939050065184517, 13.89091430021398565, 12.49999999999999822 ) ) ;
#7246 = ORIENTED_EDGE ( 'NONE', *, *, #34520, .T. ) ;
#7247 = CARTESIAN_POINT ( 'NONE',  ( 61.99999662536843914, -34.64101615137759893, -5.000000000000000000 ) ) ;
#7248 = APPLICATION_PROTOCOL_DEFINITION ( 'draft international standard', 'automotive_design', 1998, #8705 ) ;
#7249 = CARTESIAN_POINT ( 'NONE',  ( -2.500000000000000000, 3.061616997868383141E-16, -5.624496230895140947 ) ) ;
#7250 = DIRECTION ( 'NONE',  ( -0.4999999999999980016, 0.8660254037844398178, 0.000000000000000000 ) ) ;
#7251 = CYLINDRICAL_SURFACE ( 'NONE', #9601, 2.000000000000001776 ) ;
#7252 = CARTESIAN_POINT ( 'NONE',  ( -23.00000337463120559, 77.94228634059957983, -9.999999999999998224 ) ) ;
#7253 = ADVANCED_FACE ( 'NONE', ( #24922 ), #22459, .F. ) ;
#7254 = ORIENTED_EDGE ( 'NONE', *, *, #14136, .F. ) ;
#7255 = CARTESIAN_POINT ( 'NONE',  ( 3.000000000000000000, 3.673940397442059868E-16, -5.974599999999999689 ) ) ;
#7256 = CARTESIAN_POINT ( 'NONE',  ( -70.00000337463099243, 51.96152422706637708, 12.50000000000000000 ) ) ;
#7257 = LINE ( 'NONE', #32381, #14768 ) ;
#7258 = ADVANCED_FACE ( 'NONE', ( #30158 ), #4485, .T. ) ;
#7259 = EDGE_LOOP ( 'NONE', ( #9279, #4278 ) ) ;
#7260 = CIRCLE ( 'NONE', #28210, 2.000000000000001776 ) ;
#7261 = EDGE_LOOP ( 'NONE', ( #6517, #18722, #33634, #17983, #12343 ) ) ;
#7262 = EDGE_CURVE ( 'NONE', #1362, #4953, #15533, .T. ) ;
#7263 = CARTESIAN_POINT ( 'NONE',  ( 83.10590767357030018, -8.018049208621972568, -5.000000000000000000 ) ) ;
#7264 = DIRECTION ( 'NONE',  ( 0.000000000000000000, 0.000000000000000000, -1.000000000000000000 ) ) ;
#7265 = DIRECTION ( 'NONE',  ( 0.000000000000000000, 0.000000000000000000, -1.000000000000000000 ) ) ;
#7266 = EDGE_CURVE ( 'NONE', #35823, #5530, #19215, .T. ) ;
#7267 = ORIENTED_EDGE ( 'NONE', *, *, #8986, .F. ) ;
#7268 = DIRECTION ( 'NONE',  ( -0.000000000000000000, -0.000000000000000000, -1.000000000000000000 ) ) ;
#7269 = CARTESIAN_POINT ( 'NONE',  ( -37.50000000000000000, 103.4105893997321886, -19.99999999999999645 ) ) ;
#7270 = CARTESIAN_POINT ( 'NONE',  ( 64.99999662536839651, -43.30127018922199511, 17.49999999999999645 ) ) ;
#7271 = CARTESIAN_POINT ( 'NONE',  ( -78.38321060269107932, 72.20005542350995142, 32.50000000000000000 ) ) ;
#7272 = ORIENTED_EDGE ( 'NONE', *, *, #4576, .T. ) ;
#7273 = VERTEX_POINT ( 'NONE', #34618 ) ;
#7274 = DIRECTION ( 'NONE',  ( 0.000000000000000000, 0.000000000000000000, 1.000000000000000000 ) ) ;
#7275 = DIRECTION ( 'NONE',  ( 0.000000000000000000, 0.000000000000000000, 1.000000000000000000 ) ) ;
#7276 = VERTEX_POINT ( 'NONE', #3829 ) ;
#7277 = EDGE_CURVE ( 'NONE', #3917, #4661, #9089, .T. ) ;
#7278 = CARTESIAN_POINT ( 'NONE',  ( 34.00000000000000000, -103.4105893997321743, 27.50000000000000000 ) ) ;
#7279 = ORIENTED_EDGE ( 'NONE', *, *, #18335, .F. ) ;
#7280 = CARTESIAN_POINT ( 'NONE',  ( 0.000000000000000000, 0.000000000000000000, -5.700000000000000178 ) ) ;
#7281 = CARTESIAN_POINT ( 'NONE',  ( -2.500000000000003997, 4.330127018922192761, -6.000000000000000000 ) ) ;
#7282 = ORIENTED_EDGE ( 'NONE', *, *, #30075, .F. ) ;
#7283 = ORIENTED_EDGE ( 'NONE', *, *, #35507, .T. ) ;
#7284 = DIRECTION ( 'NONE',  ( 0.000000000000000000, 0.000000000000000000, 1.000000000000000000 ) ) ;
#7285 = ORIENTED_EDGE ( 'NONE', *, *, #2323, .F. ) ;
#7286 = ADVANCED_FACE ( 'NONE', ( #9479 ), #5933, .F. ) ;
#7287 = CARTESIAN_POINT ( 'NONE',  ( 34.00000000000068923, 58.88972745734143643, -4.999999999999997335 ) ) ;
#7288 = DIRECTION ( 'NONE',  ( 1.000000000000000000, 0.000000000000000000, 0.000000000000000000 ) ) ;
#7289 = CYLINDRICAL_SURFACE ( 'NONE', #17310, 2.000000000000001776 ) ;
#7290 = EDGE_CURVE ( 'NONE', #6890, #2002, #28692, .T. ) ;
#7291 = ORIENTED_EDGE ( 'NONE', *, *, #27781, .T. ) ;
#7292 =( REPRESENTATION_RELATIONSHIP ('NONE','NONE', #15268, #35440 ) REPRESENTATION_RELATIONSHIP_WITH_TRANSFORMATION ( #4255 )SHAPE_REPRESENTATION_RELATIONSHIP( ) );
#7293 = DIRECTION ( 'NONE',  ( 0.000000000000000000, -0.000000000000000000, -1.000000000000000000 ) ) ;
#7294 = CYLINDRICAL_SURFACE ( 'NONE', #34617, 3.000000000000002665 ) ;
#7295 = ORIENTED_EDGE ( 'NONE', *, *, #25930, .T. ) ;
#7296 = VERTEX_POINT ( 'NONE', #32339 ) ;
#7297 = EDGE_LOOP ( 'NONE', ( #27641, #25542, #7422, #28201 ) ) ;
#7298 = DIRECTION ( 'NONE',  ( -1.000000000000000000, 0.000000000000000000, 0.000000000000000000 ) ) ;
#7299 = AXIS2_PLACEMENT_3D ( 'NONE', #30790, #10563, #24819 ) ;
#7300 = FACE_OUTER_BOUND ( 'NONE', #26228, .T. ) ;
#7301 = EDGE_LOOP ( 'NONE', ( #31263, #3836 ) ) ;
#7302 = EDGE_CURVE ( 'NONE', #203, #16962, #30578, .T. ) ;
#7303 = CIRCLE ( 'NONE', #17466, 27.00000000000001421 ) ;
#7304 = DIRECTION ( 'NONE',  ( -1.000000000000000000, 0.000000000000000000, 0.000000000000000000 ) ) ;
#7305 = DIRECTION ( 'NONE',  ( 0.000000000000000000, 0.000000000000000000, -1.000000000000000000 ) ) ;
#7306 = VERTEX_POINT ( 'NONE', #17528 ) ;
#7307 = DIRECTION ( 'NONE',  ( 0.000000000000000000, 0.000000000000000000, 1.000000000000000000 ) ) ;
#7308 = LINE ( 'NONE', #9568, #24018 ) ;
#7309 = ADVANCED_FACE ( 'NONE', ( #20913 ), #23721, .F. ) ;
#7310 = DIRECTION ( 'NONE',  ( 0.000000000000000000, 0.000000000000000000, 1.000000000000000000 ) ) ;
#7311 = CARTESIAN_POINT ( 'NONE',  ( 0.000000000000000000, 0.000000000000000000, 0.000000000000000000 ) ) ;
#7312 = DIRECTION ( 'NONE',  ( -0.000000000000000000, -0.000000000000000000, 1.000000000000000000 ) ) ;
#7313 = DIRECTION ( 'NONE',  ( 0.000000000000000000, 0.000000000000000000, 1.000000000000000000 ) ) ;
#7314 = VERTEX_POINT ( 'NONE', #11902 ) ;
#7315 = ORIENTED_EDGE ( 'NONE', *, *, #34978, .F. ) ;
#7316 = DIRECTION ( 'NONE',  ( 0.000000000000000000, -0.000000000000000000, -1.000000000000000000 ) ) ;
#7317 = CARTESIAN_POINT ( 'NONE',  ( 61.99999662536842493, 51.96152422706639129, -9.999999999999998224 ) ) ;
#7318 = DIRECTION ( 'NONE',  ( 1.000000000000000000, 0.000000000000000000, 0.000000000000000000 ) ) ;
#7319 = CARTESIAN_POINT ( 'NONE',  ( 40.98360655737705116, 111.1639425680974398, 18.49999999999999645 ) ) ;
#7320 = ORIENTED_EDGE ( 'NONE', *, *, #5046, .F. ) ;
#7321 = UNCERTAINTY_MEASURE_WITH_UNIT (LENGTH_MEASURE( 1.000000000000000082E-05 ), #5910, 'distance_accuracy_value', 'NONE');
#7322 = FACE_OUTER_BOUND ( 'NONE', #27235, .T. ) ;
#7323 = DIRECTION ( 'NONE',  ( 1.000000000000000000, 0.000000000000000000, 0.000000000000000000 ) ) ;
#7324 = EDGE_CURVE ( 'NONE', #4760, #12700, #11711, .T. ) ;
#7325 = CARTESIAN_POINT ( 'NONE',  ( 5.000000000000000888, -2.886751345948134873, -2.080000000000000071 ) ) ;
#7326 = ORIENTED_EDGE ( 'NONE', *, *, #29029, .F. ) ;
#7327 = AXIS2_PLACEMENT_3D ( 'NONE', #4173, #29843, #12190 ) ;
#7328 = CARTESIAN_POINT ( 'NONE',  ( 70.47608876694671665, 59.13646009116074964, -49.22241343995293761 ) ) ;
#7329 = ORIENTED_EDGE ( 'NONE', *, *, #34064, .F. ) ;
#7330 =( NAMED_UNIT ( * ) PLANE_ANGLE_UNIT ( ) SI_UNIT ( $, .RADIAN. ) );
#7331 = DIRECTION ( 'NONE',  ( 0.000000000000000000, 0.000000000000000000, 1.000000000000000000 ) ) ;
#7332 = ADVANCED_FACE ( 'NONE', ( #15091 ), #35373, .F. ) ;
#7333 = DIRECTION ( 'NONE',  ( 0.000000000000000000, 0.000000000000000000, 1.000000000000000000 ) ) ;
#7334 = CARTESIAN_POINT ( 'NONE',  ( 2.255011273957053586, 4.471571325851512846, -0.5083873451168745561 ) ) ;
#7335 = EDGE_CURVE ( 'NONE', #24169, #1857, #21529, .T. ) ;
#7336 = ORIENTED_EDGE ( 'NONE', *, *, #16458, .F. ) ;
#7337 = EDGE_LOOP ( 'NONE', ( #33032, #18630, #10854, #7200 ) ) ;
#7338 = EDGE_CURVE ( 'NONE', #32985, #12040, #35303, .T. ) ;
#7339 = AXIS2_PLACEMENT_3D ( 'NONE', #4156, #15957, #4897 ) ;
#7340 = ORIENTED_EDGE ( 'NONE', *, *, #2987, .F. ) ;
#7341 = DIRECTION ( 'NONE',  ( -1.000000000000000000, 0.000000000000000000, 0.000000000000000000 ) ) ;
#7342 = CARTESIAN_POINT ( 'NONE',  ( 31.09745072740910388, 83.47442710120324705, 12.49999999999999645 ) ) ;
#7343 = CARTESIAN_POINT ( 'NONE',  ( 71.99999662536839651, 17.32050807568879236, -5.000000000000000000 ) ) ;
#7344 = CARTESIAN_POINT ( 'NONE',  ( -5.000000000000000888, -1.924500897298784041, -3.818275046351167212 ) ) ;
#7345 = DIRECTION ( 'NONE',  ( -1.000000000000000000, 0.000000000000000000, 0.000000000000000000 ) ) ;
#7346 = ORIENTED_EDGE ( 'NONE', *, *, #2019, .T. ) ;
#7347 = DIRECTION ( 'NONE',  ( 1.000000000000000000, 0.000000000000000000, 0.000000000000000000 ) ) ;
#7348 = DIRECTION ( 'NONE',  ( -1.000000000000000000, 0.000000000000000000, 0.000000000000000000 ) ) ;
#7349 = EDGE_CURVE ( 'NONE', #19893, #14036, #3111, .T. ) ;
#7350 = AXIS2_PLACEMENT_3D ( 'NONE', #28499, #2833, #23057 ) ;
#7351 = CARTESIAN_POINT ( 'NONE',  ( 64.99999662536839651, 60.62177826491078747, -5.000000000000000000 ) ) ;
#7352 = ORIENTED_EDGE ( 'NONE', *, *, #32835, .T. ) ;
#7353 = DIRECTION ( 'NONE',  ( -1.000000000000000000, 0.000000000000000000, 0.000000000000000000 ) ) ;
#7354 = DIRECTION ( 'NONE',  ( 0.000000000000000000, 0.000000000000000000, 1.000000000000000000 ) ) ;
#7355 = ORIENTED_EDGE ( 'NONE', *, *, #11843, .F. ) ;
#7356 = VERTEX_POINT ( 'NONE', #26161 ) ;
#7357 = CARTESIAN_POINT ( 'NONE',  ( -108.3061974404896262, 19.22934205795090534, 27.50000000000000000 ) ) ;
#7358 = CARTESIAN_POINT ( 'NONE',  ( 64.99999662536841072, -25.98076211353320275, 12.50000000000000000 ) ) ;
#7359 = CARTESIAN_POINT ( 'NONE',  ( 55.27226924886075921, -77.26562141134597539, 27.50000000000000000 ) ) ;
#7360 = VERTEX_POINT ( 'NONE', #23166 ) ;
#7361 = ORIENTED_EDGE ( 'NONE', *, *, #30865, .T. ) ;
#7362 = ORIENTED_EDGE ( 'NONE', *, *, #28372, .T. ) ;
#7363 = FACE_OUTER_BOUND ( 'NONE', #17797, .T. ) ;
#7364 = CIRCLE ( 'NONE', #35532, 2.000000000000001776 ) ;
#7365 = EDGE_CURVE ( 'NONE', #23506, #12265, #470, .T. ) ;
#7366 = VERTEX_POINT ( 'NONE', #28953 ) ;
#7367 = EDGE_CURVE ( 'NONE', #1054, #32590, #29899, .T. ) ;
#7368 = VERTEX_POINT ( 'NONE', #8917 ) ;
#7369 = FACE_OUTER_BOUND ( 'NONE', #35217, .T. ) ;
#7370 = ORIENTED_EDGE ( 'NONE', *, *, #6220, .F. ) ;
#7371 = ORIENTED_EDGE ( 'NONE', *, *, #12245, .T. ) ;
#7372 = LINE ( 'NONE', #18814, #5258 ) ;
#7373 = AXIS2_PLACEMENT_3D ( 'NONE', #21917, #33364, #4487 ) ;
#7374 = DIRECTION ( 'NONE',  ( 0.000000000000000000, 0.000000000000000000, 1.000000000000000000 ) ) ;
#7375 = ORIENTED_EDGE ( 'NONE', *, *, #33593, .F. ) ;
#7376 = ORIENTED_EDGE ( 'NONE', *, *, #18611, .T. ) ;
#7377 = EDGE_CURVE ( 'NONE', #12408, #12313, #7162, .T. ) ;
#7378 = DIRECTION ( 'NONE',  ( 1.000000000000000000, 0.000000000000000000, 0.000000000000000000 ) ) ;
#7379 = LINE ( 'NONE', #12228, #18359 ) ;
#7380 = DIRECTION ( 'NONE',  ( 0.000000000000000000, 0.000000000000000000, 1.000000000000000000 ) ) ;
#7381 = CARTESIAN_POINT ( 'NONE',  ( -15.00000337463126066, 77.94228634059957983, -9.999999999999998224 ) ) ;
#7382 = ORIENTED_EDGE ( 'NONE', *, *, #8737, .T. ) ;
#7383 = DIRECTION ( 'NONE',  ( 1.000000000000000000, 0.000000000000000000, 0.000000000000000000 ) ) ;
#7384 = ORIENTED_EDGE ( 'NONE', *, *, #31079, .T. ) ;
#7385 = LINE ( 'NONE', #33253, #22773 ) ;
#7386 = DIRECTION ( 'NONE',  ( 0.000000000000000000, 0.000000000000000000, 1.000000000000000000 ) ) ;
#7387 = CIRCLE ( 'NONE', #2000, 2.000000000000001776 ) ;
#7388 = CARTESIAN_POINT ( 'NONE',  ( 35.83991598322139538, 56.52018970185221747, -49.22241343995293761 ) ) ;
#7389 = CARTESIAN_POINT ( 'NONE',  ( 69.99999662536841072, 51.96152422706640550, -5.000000000000000000 ) ) ;
#7390 = EDGE_CURVE ( 'NONE', #2540, #28847, #4162, .T. ) ;
#7391 = CARTESIAN_POINT ( 'NONE',  ( -55.00000337463107059, 60.62177826491078747, 17.49999999999999645 ) ) ;
#7392 = EDGE_CURVE ( 'NONE', #32947, #21445, #14915, .T. ) ;
#7393 = AXIS2_PLACEMENT_3D ( 'NONE', #14779, #34682, #34480 ) ;
#7394 = DIRECTION ( 'NONE',  ( 0.000000000000000000, 0.000000000000000000, 1.000000000000000000 ) ) ;
#7395 = EDGE_CURVE ( 'NONE', #13632, #33336, #16136, .T. ) ;
#7396 = ADVANCED_FACE ( 'NONE', ( #13373 ), #24831, .F. ) ;
#7397 = DIRECTION ( 'NONE',  ( 0.000000000000000000, 0.000000000000000000, -1.000000000000000000 ) ) ;
#7398 = ORIENTED_EDGE ( 'NONE', *, *, #26805, .T. ) ;
#7399 = CARTESIAN_POINT ( 'NONE',  ( 73.47608876694671665, 59.13646009116074964, -49.22241343995293761 ) ) ;
#7400 = DIRECTION ( 'NONE',  ( 0.000000000000000000, 0.000000000000000000, -1.000000000000000000 ) ) ;
#7401 = DIRECTION ( 'NONE',  ( 0.000000000000000000, 0.000000000000000000, 1.000000000000000000 ) ) ;
#7402 = CIRCLE ( 'NONE', #35019, 3.000000000000007105 ) ;
#7403 = VERTEX_POINT ( 'NONE', #4027 ) ;
#7404 = ORIENTED_EDGE ( 'NONE', *, *, #18758, .F. ) ;
#7405 = EDGE_LOOP ( 'NONE', ( #22340, #26272, #16422, #30979, #30208, #12182, #13169, #4363 ) ) ;
#7406 = CIRCLE ( 'NONE', #28341, 2.000000000000001776 ) ;
#7407 = DIRECTION ( 'NONE',  ( 0.000000000000000000, 0.000000000000000000, -1.000000000000000000 ) ) ;
#7408 = DIRECTION ( 'NONE',  ( 1.000000000000000000, 0.000000000000000000, 0.000000000000000000 ) ) ;
#7409 = ORIENTED_EDGE ( 'NONE', *, *, #4856, .T. ) ;
#7410 = AXIS2_PLACEMENT_3D ( 'NONE', #35380, #23927, #30080 ) ;
#7411 = DIRECTION ( 'NONE',  ( 1.000000000000000000, 0.000000000000000000, 0.000000000000000000 ) ) ;
#7412 = LINE ( 'NONE', #13786, #35089 ) ;
#7413 = EDGE_LOOP ( 'NONE', ( #2008, #4074, #20125, #24446 ) ) ;
#7414 = FACE_BOUND ( 'NONE', #17685, .T. ) ;
#7415 = VERTEX_POINT ( 'NONE', #30456 ) ;
#7416 = FACE_BOUND ( 'NONE', #19550, .T. ) ;
#7417 = AXIS2_PLACEMENT_3D ( 'NONE', #35677, #35329, #18627 ) ;
#7418 = EDGE_CURVE ( 'NONE', #31822, #2372, #16028, .T. ) ;
#7419 = DIRECTION ( 'NONE',  ( 1.000000000000000000, 0.000000000000000000, 0.000000000000000000 ) ) ;
#7420 = CARTESIAN_POINT ( 'NONE',  ( 54.99999662536846046, -43.30127018922200222, -9.999999999999998224 ) ) ;
#7421 =( LENGTH_UNIT ( ) NAMED_UNIT ( * ) SI_UNIT ( .MILLI., .METRE. ) );
#7422 = ORIENTED_EDGE ( 'NONE', *, *, #3706, .T. ) ;
#7423 = CARTESIAN_POINT ( 'NONE',  ( 6.249999999999998224, 3.673940397442060854E-16, -3.000000000000000888 ) ) ;
#7424 = AXIS2_PLACEMENT_3D ( 'NONE', #858, #15499, #18107 ) ;
#7425 = CYLINDRICAL_SURFACE ( 'NONE', #35070, 3.000000000000002665 ) ;
#7426 = CYLINDRICAL_SURFACE ( 'NONE', #10473, 2.000000000000001776 ) ;
#7427 = AXIS2_PLACEMENT_3D ( 'NONE', #12028, #23665, #6974 ) ;
#7428 = CARTESIAN_POINT ( 'NONE',  ( -78.00000337463096400, -34.64101615137762025, -9.999999999999998224 ) ) ;
#7429 = DIRECTION ( 'NONE',  ( 1.000000000000000000, 0.000000000000000000, 0.000000000000000000 ) ) ;
#7430 = ORIENTED_EDGE ( 'NONE', *, *, #10226, .T. ) ;
#7431 = DIRECTION ( 'NONE',  ( -0.000000000000000000, -0.000000000000000000, 1.000000000000000000 ) ) ;
#7432 = CARTESIAN_POINT ( 'NONE',  ( -37.50000000000000000, 103.4105893997321743, -11.00000000000000355 ) ) ;
#7433 = FACE_OUTER_BOUND ( 'NONE', #18307, .T. ) ;
#7434 = EDGE_LOOP ( 'NONE', ( #15665, #3103 ) ) ;
#7435 = EDGE_CURVE ( 'NONE', #13911, #22954, #17331, .T. ) ;
#7436 = VERTEX_POINT ( 'NONE', #36086 ) ;
#7437 = CARTESIAN_POINT ( 'NONE',  ( -68.00000337463099243, 34.64101615137758472, -9.999999999999998224 ) ) ;
#7438 = CARTESIAN_POINT ( 'NONE',  ( 46.99999662536849598, 60.62177826491077326, -9.999999999999998224 ) ) ;
#7439 = VECTOR ( 'NONE', #33524, 1000.000000000000000 ) ;
#7440 = DIRECTION ( 'NONE',  ( -0.000000000000000000, -0.000000000000000000, 1.000000000000000000 ) ) ;
#7441 = EDGE_LOOP ( 'NONE', ( #33974, #17537, #6154, #2943, #31652 ) ) ;
#7442 = DIRECTION ( 'NONE',  ( 1.000000000000000000, 0.000000000000000000, 0.000000000000000000 ) ) ;
#7443 = CYLINDRICAL_SURFACE ( 'NONE', #6925, 3.500000000000003109 ) ;
#7444 = CARTESIAN_POINT ( 'NONE',  ( 33.99999999999999289, 103.4105893997321743, 27.49999999999999645 ) ) ;
#7445 = FACE_OUTER_BOUND ( 'NONE', #17533, .T. ) ;
#7446 = ORIENTED_EDGE ( 'NONE', *, *, #19753, .F. ) ;
#7447 = CIRCLE ( 'NONE', #23000, 2.000000000000001776 ) ;
#7448 = VERTEX_POINT ( 'NONE', #32701 ) ;
#7449 = DIRECTION ( 'NONE',  ( 1.000000000000000000, 0.000000000000000000, 0.000000000000000000 ) ) ;
#7450 = AXIS2_PLACEMENT_3D ( 'NONE', #34165, #3190, #368 ) ;
#7451 = CARTESIAN_POINT ( 'NONE',  ( -70.00000337463102085, -51.96152422706641971, 17.49999999999999645 ) ) ;
#7452 = ORIENTED_EDGE ( 'NONE', *, *, #2319, .T. ) ;
#7453 = CARTESIAN_POINT ( 'NONE',  ( -1.582370436567960503, -4.859920694386081763, -3.719399823475761480 ) ) ;
#7454 = ORIENTED_EDGE ( 'NONE', *, *, #15395, .T. ) ;
#7455 = CARTESIAN_POINT ( 'NONE',  ( -70.00000337463099243, 51.96152422706637708, -9.999999999999998224 ) ) ;
#7456 = EDGE_CURVE ( 'NONE', #7637, #9530, #25130, .T. ) ;
#7457 = EDGE_CURVE ( 'NONE', #8932, #30738, #5377, .T. ) ;
#7458 = DIRECTION ( 'NONE',  ( 1.000000000000000000, 0.000000000000000000, 0.000000000000000000 ) ) ;
#7459 = EDGE_LOOP ( 'NONE', ( #29243, #15773 ) ) ;
#7460 = CIRCLE ( 'NONE', #8659, 2.000000000000001776 ) ;
#7461 = CARTESIAN_POINT ( 'NONE',  ( 0.7030283904599238243, 5.367609061416947824, -4.096693167835341320 ) ) ;
#7462 = VERTEX_POINT ( 'NONE', #1775 ) ;
#7463 = DIRECTION ( 'NONE',  ( 0.000000000000000000, 0.000000000000000000, 1.000000000000000000 ) ) ;
#7464 = CIRCLE ( 'NONE', #20036, 2.000000000000000000 ) ;
#7465 = DIRECTION ( 'NONE',  ( 0.000000000000000000, 0.000000000000000000, -1.000000000000000000 ) ) ;
#7466 = EDGE_CURVE ( 'NONE', #21403, #27674, #5958, .T. ) ;
#7467 = DIRECTION ( 'NONE',  ( 0.000000000000000000, 0.000000000000000000, 1.000000000000000000 ) ) ;
#7468 = DIRECTION ( 'NONE',  ( 1.000000000000000000, 0.000000000000000000, 0.000000000000000000 ) ) ;
#7469 = ORIENTED_EDGE ( 'NONE', *, *, #8184, .T. ) ;
#7470 = DIRECTION ( 'NONE',  ( 0.000000000000000000, 0.000000000000000000, 1.000000000000000000 ) ) ;
#7471 = DIRECTION ( 'NONE',  ( 0.5000000000000039968, 0.8660254037844363761, 0.000000000000000000 ) ) ;
#7472 = DIRECTION ( 'NONE',  ( -0.000000000000000000, -0.000000000000000000, 1.000000000000000000 ) ) ;
#7473 = ORIENTED_EDGE ( 'NONE', *, *, #32564, .T. ) ;
#7474 = VECTOR ( 'NONE', #1105, 1000.000000000000000 ) ;
#7475 = CIRCLE ( 'NONE', #31416, 2.000000000000001776 ) ;
#7476 = ORIENTED_EDGE ( 'NONE', *, *, #23774, .T. ) ;
#7477 = CIRCLE ( 'NONE', #33216, 33.00000000000001421 ) ;
#7478 = VERTEX_POINT ( 'NONE', #24653 ) ;
#7479 = AXIS2_PLACEMENT_3D ( 'NONE', #19800, #31387, #8168 ) ;
#7480 = EDGE_CURVE ( 'NONE', #11344, #16972, #20915, .T. ) ;
#7481 = DIRECTION ( 'NONE',  ( 1.000000000000000000, 0.000000000000000000, 0.000000000000000000 ) ) ;
#7482 = VERTEX_POINT ( 'NONE', #27456 ) ;
#7483 = DIRECTION ( 'NONE',  ( 0.000000000000000000, 0.000000000000000000, -1.000000000000000000 ) ) ;
#7484 = DIRECTION ( 'NONE',  ( 0.000000000000000000, 0.000000000000000000, 1.000000000000000000 ) ) ;
#7485 = CARTESIAN_POINT ( 'NONE',  ( 59.99999662536842493, -51.96152422706639840, -9.999999999999998224 ) ) ;
#7486 = AXIS2_PLACEMENT_3D ( 'NONE', #26812, #18743, #24174 ) ;
#7487 = DIRECTION ( 'NONE',  ( -0.000000000000000000, -0.000000000000000000, 1.000000000000000000 ) ) ;
#7488 = DIRECTION ( 'NONE',  ( 1.000000000000000000, 0.000000000000000000, 0.000000000000000000 ) ) ;
#7489 = FACE_OUTER_BOUND ( 'NONE', #32444, .T. ) ;
#7490 = CARTESIAN_POINT ( 'NONE',  ( 62.99999662536841072, -25.98076211353320275, 17.49999999999999645 ) ) ;
#7491 = ORIENTED_EDGE ( 'NONE', *, *, #3146, .T. ) ;
#7492 = CIRCLE ( 'NONE', #22446, 2.000000000000001776 ) ;
#7493 = EDGE_LOOP ( 'NONE', ( #25181, #18986, #12274, #17819 ) ) ;
#7494 = CARTESIAN_POINT ( 'NONE',  ( -85.00000337463092137, 8.660254037844389075, 17.49999999999999645 ) ) ;
#7495 = ADVANCED_FACE ( 'NONE', ( #27252 ), #4782, .F. ) ;
#7496 = FACE_OUTER_BOUND ( 'NONE', #25199, .T. ) ;
#7497 = DIRECTION ( 'NONE',  ( 0.000000000000000000, 0.000000000000000000, 1.000000000000000000 ) ) ;
#7498 = CARTESIAN_POINT ( 'NONE',  ( 49.99999662536846756, 69.28203230275516944, -9.999999999999998224 ) ) ;
#7499 = ORIENTED_EDGE ( 'NONE', *, *, #17102, .F. ) ;
#7500 = VECTOR ( 'NONE', #20543, 1000.000000000000000 ) ;
#7501 = CARTESIAN_POINT ( 'NONE',  ( 41.99999662536853151, -69.28203230275519786, -5.000000000000000000 ) ) ;
#7502 = VECTOR ( 'NONE', #16008, 1000.000000000000000 ) ;
#7503 = DIRECTION ( 'NONE',  ( 1.000000000000000000, 0.000000000000000000, 0.000000000000000000 ) ) ;
#7504 = CYLINDRICAL_SURFACE ( 'NONE', #31155, 2.000000000000001776 ) ;
#7505 = VERTEX_POINT ( 'NONE', #29897 ) ;
#7506 = EDGE_CURVE ( 'NONE', #31238, #26391, #30498, .T. ) ;
#7507 = LINE ( 'NONE', #35644, #22600 ) ;
#7508 = ORIENTED_EDGE ( 'NONE', *, *, #27435, .F. ) ;
#7509 = DIRECTION ( 'NONE',  ( 0.000000000000000000, 0.000000000000000000, -1.000000000000000000 ) ) ;
#7510 = DIRECTION ( 'NONE',  ( 0.000000000000000000, 0.000000000000000000, -1.000000000000000000 ) ) ;
#7511 = EDGE_CURVE ( 'NONE', #550, #29302, #14332, .T. ) ;
#7512 = AXIS2_PLACEMENT_3D ( 'NONE', #33293, #1247, #13401 ) ;
#7513 = CARTESIAN_POINT ( 'NONE',  ( 0.7178748134486927501, 5.359037475107204962, -1.327869168827484403 ) ) ;
#7514 = ORIENTED_EDGE ( 'NONE', *, *, #20903, .T. ) ;
#7515 = VECTOR ( 'NONE', #36085, 1000.000000000000000 ) ;
#7516 = ORIENTED_EDGE ( 'NONE', *, *, #11134, .T. ) ;
#7517 = AXIS2_PLACEMENT_3D ( 'NONE', #24232, #12981, #15627 ) ;
#7518 = PLANE ( 'NONE',  #36538 ) ;
#7519 = CIRCLE ( 'NONE', #18900, 27.00000000000001066 ) ;
#7520 = AXIS2_PLACEMENT_3D ( 'NONE', #21020, #34737, #11830 ) ;
#7521 = VERTEX_POINT ( 'NONE', #10219 ) ;
#7522 = FACE_OUTER_BOUND ( 'NONE', #30640, .T. ) ;
#7523 = DIRECTION ( 'NONE',  ( 1.000000000000000000, 0.000000000000000000, 0.000000000000000000 ) ) ;
#7524 = DIRECTION ( 'NONE',  ( 0.000000000000000000, 0.000000000000000000, 1.000000000000000000 ) ) ;
#7525 = CARTESIAN_POINT ( 'NONE',  ( -60.00000337463107059, -34.64101615137762025, -9.999999999999998224 ) ) ;
#7526 = LINE ( 'NONE', #7172, #36324 ) ;
#7527 = VERTEX_POINT ( 'NONE', #27077 ) ;
#7528 = DIRECTION ( 'NONE',  ( -0.000000000000000000, 0.000000000000000000, 1.000000000000000000 ) ) ;
#7529 = AXIS2_PLACEMENT_3D ( 'NONE', #32562, #21314, #18699 ) ;
#7530 = ADVANCED_FACE ( 'NONE', ( #29697 ), #21647, .F. ) ;
#7531 = DIRECTION ( 'NONE',  ( 1.000000000000000000, 0.000000000000000000, 0.000000000000000000 ) ) ;
#7532 = VERTEX_POINT ( 'NONE', #32902 ) ;
#7533 = CARTESIAN_POINT ( 'NONE',  ( 79.83584911142594365, 32.64776363509508883, -5.000000000000000000 ) ) ;
#7534 = DIRECTION ( 'NONE',  ( 0.000000000000000000, 0.000000000000000000, 1.000000000000000000 ) ) ;
#7535 = ORIENTED_EDGE ( 'NONE', *, *, #36084, .F. ) ;
#7536 = ADVANCED_FACE ( 'NONE', ( #21819 ), #12810, .F. ) ;
#7537 = ORIENTED_EDGE ( 'NONE', *, *, #33856, .F. ) ;
#7538 = AXIS2_PLACEMENT_3D ( 'NONE', #1385, #18653, #25028 ) ;
#7539 = EDGE_CURVE ( 'NONE', #25339, #33109, #8371, .T. ) ;
#7540 = CARTESIAN_POINT ( 'NONE',  ( 72.99999662536836809, 43.30127018922198801, -5.000000000000000000 ) ) ;
#7541 = DIRECTION ( 'NONE',  ( 0.000000000000000000, -0.000000000000000000, -1.000000000000000000 ) ) ;
#7542 = AXIS2_PLACEMENT_3D ( 'NONE', #1342, #21412, #7724 ) ;
#7543 = DIRECTION ( 'NONE',  ( 1.000000000000000000, 0.000000000000000000, 0.000000000000000000 ) ) ;
#7544 = ORIENTED_EDGE ( 'NONE', *, *, #18131, .T. ) ;
#7545 = ORIENTED_EDGE ( 'NONE', *, *, #22194, .T. ) ;
#7546 = CIRCLE ( 'NONE', #17707, 27.00000000000001421 ) ;
#7547 = EDGE_LOOP ( 'NONE', ( #14302, #10711 ) ) ;
#7548 = CIRCLE ( 'NONE', #955, 2.000000000000001776 ) ;
#7549 = AXIS2_PLACEMENT_3D ( 'NONE', #19936, #2339, #25219 ) ;
#7550 = CARTESIAN_POINT ( 'NONE',  ( -58.00000337463104216, 34.64101615137757051, -5.000000000000000000 ) ) ;
#7551 = AXIS2_PLACEMENT_3D ( 'NONE', #11560, #34460, #14208 ) ;
#7552 = ORIENTED_EDGE ( 'NONE', *, *, #1319, .T. ) ;
#7553 = CARTESIAN_POINT ( 'NONE',  ( -95.00000000000001421, 1.163414459189985801E-14, -10.00000000000000000 ) ) ;
#7554 = AXIS2_PLACEMENT_3D ( 'NONE', #22249, #33688, #16821 ) ;
#7555 = VERTEX_POINT ( 'NONE', #15827 ) ;
#7556 = ORIENTED_EDGE ( 'NONE', *, *, #20296, .F. ) ;
#7557 = AXIS2_PLACEMENT_3D ( 'NONE', #22588, #34044, #22791 ) ;
#7558 = CARTESIAN_POINT ( 'NONE',  ( -77.00000337463099243, -25.98076211353322051, 17.49999999999999645 ) ) ;
#7559 = EDGE_CURVE ( 'NONE', #34954, #34992, #34120, .T. ) ;
#7560 = DIRECTION ( 'NONE',  ( -1.000000000000000000, 0.000000000000000000, 0.000000000000000000 ) ) ;
#7561 = VERTEX_POINT ( 'NONE', #22565 ) ;
#7562 = ORIENTED_EDGE ( 'NONE', *, *, #25041, .F. ) ;
#7563 = CARTESIAN_POINT ( 'NONE',  ( -40.00000337463113453, 69.28203230275516944, -9.999999999999998224 ) ) ;
#7564 = CARTESIAN_POINT ( 'NONE',  ( 101.4249800177813086, -31.43204461043964315, 32.50002500000000083 ) ) ;
#7565 = AXIS2_PLACEMENT_3D ( 'NONE', #34058, #28228, #5374 ) ;
#7566 = CARTESIAN_POINT ( 'NONE',  ( 62.99999662536839651, -60.62177826491080168, -9.999999999999998224 ) ) ;
#7567 = LINE ( 'NONE', #16374, #4102 ) ;
#7568 = ORIENTED_EDGE ( 'NONE', *, *, #13202, .T. ) ;
#7569 = CARTESIAN_POINT ( 'NONE',  ( 4.999996625368645198, 77.94228634059957983, -9.999999999999998224 ) ) ;
#7570 = DIRECTION ( 'NONE',  ( 1.000000000000000000, 0.000000000000000000, 0.000000000000000000 ) ) ;
#7571 = DIRECTION ( 'NONE',  ( 0.000000000000000000, 0.000000000000000000, -1.000000000000000000 ) ) ;
#7572 = CARTESIAN_POINT ( 'NONE',  ( 84.99999662536831124, -8.660254037844397956, -9.999999999999998224 ) ) ;
#7573 = DIRECTION ( 'NONE',  ( 1.000000000000000000, 0.000000000000000000, 0.000000000000000000 ) ) ;
#7574 = DIRECTION ( 'NONE',  ( 0.000000000000000000, 0.000000000000000000, 1.000000000000000000 ) ) ;
#7575 = AXIS2_PLACEMENT_3D ( 'NONE', #24426, #6978, #1179 ) ;
#7576 = AXIS2_PLACEMENT_3D ( 'NONE', #21122, #12675, #12496 ) ;
#7577 = EDGE_CURVE ( 'NONE', #6948, #10265, #26319, .T. ) ;
#7578 = DIRECTION ( 'NONE',  ( 0.000000000000000000, 0.000000000000000000, -1.000000000000000000 ) ) ;
#7579 = CARTESIAN_POINT ( 'NONE',  ( 3.000000000000000000, 0.000000000000000000, 2.541999999999999815 ) ) ;
#7580 = ORIENTED_EDGE ( 'NONE', *, *, #19939, .F. ) ;
#7581 = EDGE_CURVE ( 'NONE', #36464, #36567, #14946, .T. ) ;
#7582 = DIRECTION ( 'NONE',  ( 0.000000000000000000, 0.000000000000000000, 1.000000000000000000 ) ) ;
#7583 = CARTESIAN_POINT ( 'NONE',  ( -2.500000000000003997, 4.330127018922192761, -6.000000000000000000 ) ) ;
#7584 = CARTESIAN_POINT ( 'NONE',  ( -5.999999999999985789, -149.8799519615616305, 32.55002500000000509 ) ) ;
#7585 = ORIENTED_EDGE ( 'NONE', *, *, #945, .F. ) ;
#7586 = CIRCLE ( 'NONE', #24968, 2.000000000000001776 ) ;
#7587 = EDGE_CURVE ( 'NONE', #31164, #24047, #27547, .T. ) ;
#7588 = ORIENTED_EDGE ( 'NONE', *, *, #10732, .F. ) ;
#7589 = EDGE_LOOP ( 'NONE', ( #6847, #17308, #19190, #29526 ) ) ;
#7590 = CARTESIAN_POINT ( 'NONE',  ( 24.99999662536859546, -77.94228634059960825, -9.999999999999998224 ) ) ;
#7591 = DIRECTION ( 'NONE',  ( 0.000000000000000000, 0.000000000000000000, 1.000000000000000000 ) ) ;
#7592 = EDGE_CURVE ( 'NONE', #4869, #34330, #24539, .T. ) ;
#7593 = ORIENTED_EDGE ( 'NONE', *, *, #910, .T. ) ;
#7594 = EDGE_CURVE ( 'NONE', #8273, #10919, #3566, .T. ) ;
#7595 = AXIS2_PLACEMENT_3D ( 'NONE', #35901, #10211, #7383 ) ;
#7596 = DIRECTION ( 'NONE',  ( 0.000000000000000000, 0.000000000000000000, 1.000000000000000000 ) ) ;
#7597 = FACE_OUTER_BOUND ( 'NONE', #22745, .T. ) ;
#7598 = ORIENTED_EDGE ( 'NONE', *, *, #24319, .T. ) ;
#7599 = CARTESIAN_POINT ( 'NONE',  ( -72.00000337463100664, -2.404119930384582903E-14, -9.999999999999998224 ) ) ;
#7600 = ORIENTED_EDGE ( 'NONE', *, *, #12389, .T. ) ;
#7601 = FACE_BOUND ( 'NONE', #21800, .T. ) ;
#7602 = EDGE_CURVE ( 'NONE', #7637, #12047, #28553, .T. ) ;
#7603 = AXIS2_PLACEMENT_3D ( 'NONE', #36516, #14369, #5551 ) ;
#7604 = AXIS2_PLACEMENT_3D ( 'NONE', #15573, #13126, #933 ) ;
#7605 = ADVANCED_FACE ( 'NONE', ( #16385 ), #2887, .F. ) ;
#7606 = AXIS2_PLACEMENT_3D ( 'NONE', #15467, #18652, #24085 ) ;
#7607 = DIRECTION ( 'NONE',  ( 1.000000000000000000, 0.000000000000000000, 0.000000000000000000 ) ) ;
#7608 = DIRECTION ( 'NONE',  ( 1.000000000000000000, 0.000000000000000000, 0.000000000000000000 ) ) ;
#7609 = EDGE_CURVE ( 'NONE', #942, #14720, #4811, .T. ) ;
#7610 = EDGE_CURVE ( 'NONE', #25010, #4390, #25157, .T. ) ;
#7611 = FACE_OUTER_BOUND ( 'NONE', #25967, .T. ) ;
#7612 = ADVANCED_FACE ( 'NONE', ( #2509 ), #36267, .F. ) ;
#7613 = VERTEX_POINT ( 'NONE', #28191 ) ;
#7614 = CARTESIAN_POINT ( 'NONE',  ( 111.8061974404898962, 19.22934205794938478, 27.50000000000000000 ) ) ;
#7615 = CONTEXT_DEPENDENT_SHAPE_REPRESENTATION ( #29057, #19113 ) ;
#7616 = AXIS2_PLACEMENT_3D ( 'NONE', #27051, #1364, #35689 ) ;
#7617 = CARTESIAN_POINT ( 'NONE',  ( 19.99999662536858835, 69.28203230275516944, -9.999999999999998224 ) ) ;
#7618 = CARTESIAN_POINT ( 'NONE',  ( -60.00000337463104216, 51.96152422706639129, -9.999999999999998224 ) ) ;
#7619 = ORIENTED_EDGE ( 'NONE', *, *, #26377, .F. ) ;
#7620 = DIRECTION ( 'NONE',  ( 0.000000000000000000, 1.000000000000000000, -1.224646799147353207E-16 ) ) ;
#7621 = CYLINDRICAL_SURFACE ( 'NONE', #34711, 2.000000000000001776 ) ;
#7622 = ORIENTED_EDGE ( 'NONE', *, *, #20422, .T. ) ;
#7623 = DIRECTION ( 'NONE',  ( 0.000000000000000000, 0.000000000000000000, 1.000000000000000000 ) ) ;
#7624 = CIRCLE ( 'NONE', #11288, 8.500000000000007105 ) ;
#7625 = CARTESIAN_POINT ( 'NONE',  ( -5.000000000000000000, 2.886751345948126879, -6.000000000000000000 ) ) ;
#7626 = FACE_OUTER_BOUND ( 'NONE', #11340, .T. ) ;
#7627 = CIRCLE ( 'NONE', #23787, 2.000000000000001776 ) ;
#7628 = AXIS2_PLACEMENT_3D ( 'NONE', #5460, #172, #34319 ) ;
#7629 = ORIENTED_EDGE ( 'NONE', *, *, #32567, .F. ) ;
#7630 = AXIS2_PLACEMENT_3D ( 'NONE', #18477, #12248, #15273 ) ;
#7631 = EDGE_LOOP ( 'NONE', ( #22935, #11297 ) ) ;
#7632 = FACE_OUTER_BOUND ( 'NONE', #15542, .T. ) ;
#7633 = CARTESIAN_POINT ( 'NONE',  ( -5.184911785340869272, 2.993510214990760865, -4.330720594357042152 ) ) ;
#7634 = CIRCLE ( 'NONE', #28578, 2.000000000000001776 ) ;
#7635 = CARTESIAN_POINT ( 'NONE',  ( -37.00000337463116296, -60.62177826491080168, 17.49999999999999645 ) ) ;
#7636 = CIRCLE ( 'NONE', #28580, 33.00000000000002132 ) ;
#7637 = VERTEX_POINT ( 'NONE', #13571 ) ;
#7638 = VERTEX_POINT ( 'NONE', #7775 ) ;
#7639 = PLANE ( 'NONE',  #12772 ) ;
#7640 = CARTESIAN_POINT ( 'NONE',  ( -2.260257450329326456, 4.468542444510766209, -0.5197061503823194872 ) ) ;
#7641 = CARTESIAN_POINT ( 'NONE',  ( -70.80619744048887299, 84.18124734178336155, 27.50000000000000000 ) ) ;
#7642 = CIRCLE ( 'NONE', #4648, 95.00000000000001421 ) ;
#7643 = DIRECTION ( 'NONE',  ( 1.000000000000000000, 0.000000000000000000, 0.000000000000000000 ) ) ;
#7644 = ORIENTED_EDGE ( 'NONE', *, *, #4871, .F. ) ;
#7645 = VERTEX_POINT ( 'NONE', #25214 ) ;
#7646 = CARTESIAN_POINT ( 'NONE',  ( 4.999999999999999112, 0.2466074518009281902, -1.346217697502835001E-15 ) ) ;
#7647 = CYLINDRICAL_SURFACE ( 'NONE', #2104, 45.00000000000000000 ) ;
#7648 = ORIENTED_EDGE ( 'NONE', *, *, #9673, .F. ) ;
#7649 = CARTESIAN_POINT ( 'NONE',  ( 71.99999662536838230, -34.64101615137759183, 17.49999999999999645 ) ) ;
#7650 = ORIENTED_EDGE ( 'NONE', *, *, #5642, .T. ) ;
#7651 = VECTOR ( 'NONE', #34983, 1000.000000000000000 ) ;
#7652 = CIRCLE ( 'NONE', #28599, 2.000000000000001776 ) ;
#7653 = LINE ( 'NONE', #16103, #21931 ) ;
#7654 = VECTOR ( 'NONE', #11306, 1000.000000000000000 ) ;
#7655 = VECTOR ( 'NONE', #27032, 1000.000000000000000 ) ;
#7656 = CARTESIAN_POINT ( 'NONE',  ( -52.00000337463112032, -51.96152422706641971, 17.49999999999999645 ) ) ;
#7657 = EDGE_CURVE ( 'NONE', #32118, #24986, #36461, .T. ) ;
#7658 = DIRECTION ( 'NONE',  ( 0.000000000000000000, 0.000000000000000000, -1.000000000000000000 ) ) ;
#7659 = ORIENTED_EDGE ( 'NONE', *, *, #15113, .T. ) ;
#7660 = FILL_AREA_STYLE ('',( #30335 ) ) ;
#7661 = CARTESIAN_POINT ( 'NONE',  ( 3.000000000000000000, 2.935248768560057453, -3.903127820947815962E-15 ) ) ;
#7662 = CIRCLE ( 'NONE', #28609, 95.00000000000001421 ) ;
#7663 = CARTESIAN_POINT ( 'NONE',  ( 56.67878100130369035, -27.78182860042797131, 12.49999999999999822 ) ) ;
#7664 = CARTESIAN_POINT ( 'NONE',  ( 0.000000000000000000, 0.000000000000000000, -5.000000000000000000 ) ) ;
#7665 = ORIENTED_EDGE ( 'NONE', *, *, #639, .T. ) ;
#7666 = CARTESIAN_POINT ( 'NONE',  ( -66.98486643701050980, 43.54686869003479899, -5.000000000000000000 ) ) ;
#7667 = DIRECTION ( 'NONE',  ( 1.000000000000000000, 0.000000000000000000, 0.000000000000000000 ) ) ;
#7668 = CIRCLE ( 'NONE', #33419, 3.000000000000002220 ) ;
#7669 = CARTESIAN_POINT ( 'NONE',  ( 49.99999662536846756, 51.96152422706637708, 17.49999999999999645 ) ) ;
#7670 = EDGE_LOOP ( 'NONE', ( #35271, #3200 ) ) ;
#7671 = ORIENTED_EDGE ( 'NONE', *, *, #5789, .T. ) ;
#7672 = ORIENTED_EDGE ( 'NONE', *, *, #8278, .T. ) ;
#7673 = AXIS2_PLACEMENT_3D ( 'NONE', #19914, #34356, #16558 ) ;
#7674 = LINE ( 'NONE', #13461, #18541 ) ;
#7675 = VERTEX_POINT ( 'NONE', #13765 ) ;
#7676 = CIRCLE ( 'NONE', #22056, 3.250000000000001332 ) ;
#7677 = AXIS2_PLACEMENT_3D ( 'NONE', #29639, #9412, #21207 ) ;
#7678 = CARTESIAN_POINT ( 'NONE',  ( 59.99999662536845335, 34.64101615137759893, 12.50000000000000000 ) ) ;
#7679 = DIRECTION ( 'NONE',  ( 1.000000000000000000, 0.000000000000000000, 0.000000000000000000 ) ) ;
#7680 = EDGE_CURVE ( 'NONE', #2655, #33332, #34731, .T. ) ;
#7681 = AXIS2_PLACEMENT_3D ( 'NONE', #15510, #4439, #21305 ) ;
#7682 = FACE_OUTER_BOUND ( 'NONE', #26598, .T. ) ;
#7683 = AXIS2_PLACEMENT_3D ( 'NONE', #31852, #1132, #6743 ) ;
#7684 = CARTESIAN_POINT ( 'NONE',  ( 34.99999662536855283, -60.62177826491080168, -9.999999999999998224 ) ) ;
#7685 = CARTESIAN_POINT ( 'NONE',  ( 83.67710222720860713, -27.48074558388129773, -5.000000000000000000 ) ) ;
#7686 = CARTESIAN_POINT ( 'NONE',  ( -72.00000337463100664, 17.32050807568877460, -9.999999999999998224 ) ) ;
#7687 = CYLINDRICAL_SURFACE ( 'NONE', #17218, 2.000000000000001776 ) ;
#7688 = CARTESIAN_POINT ( 'NONE',  ( 3.000000000000000000, -2.201436576420042979, 1.271000000000003682 ) ) ;
#7689 = ORIENTED_EDGE ( 'NONE', *, *, #23385, .F. ) ;
#7690 = EDGE_LOOP ( 'NONE', ( #31467, #28838, #4670, #14373 ) ) ;
#7691 = CIRCLE ( 'NONE', #28633, 33.00000000000001421 ) ;
#7692 = DIRECTION ( 'NONE',  ( 0.000000000000000000, 0.000000000000000000, 1.000000000000000000 ) ) ;
#7693 = CARTESIAN_POINT ( 'NONE',  ( 35.19434990244975126, -52.39915983220758022, -4.999999999999997335 ) ) ;
#7694 = DIRECTION ( 'NONE',  ( 0.000000000000000000, 0.000000000000000000, 1.000000000000000000 ) ) ;
#7695 = CARTESIAN_POINT ( 'NONE',  ( -20.00000337463124112, 69.28203230275516944, -5.000000000000000000 ) ) ;
#7696 = ORIENTED_EDGE ( 'NONE', *, *, #11404, .F. ) ;
#7697 = UNCERTAINTY_MEASURE_WITH_UNIT (LENGTH_MEASURE( 1.000000000000000082E-05 ), #35038, 'distance_accuracy_value', 'NONE');
#7698 = AXIS2_PLACEMENT_3D ( 'NONE', #1464, #2023, #15728 ) ;
#7699 = CARTESIAN_POINT ( 'NONE',  ( 74.99999662536836809, 8.660254037844394404, 12.50000000000000000 ) ) ;
#7700 = CARTESIAN_POINT ( 'NONE',  ( 2.500000000000021760, -4.330127018922177662, 0.000000000000000000 ) ) ;
#7701 = VECTOR ( 'NONE', #24032, 1000.000000000000000 ) ;
#7702 = ORIENTED_EDGE ( 'NONE', *, *, #8383, .F. ) ;
#7703 = ADVANCED_FACE ( 'NONE', ( #5341 ), #36812, .F. ) ;
#7704 = DIRECTION ( 'NONE',  ( -1.000000000000000000, -0.000000000000000000, -0.000000000000000000 ) ) ;
#7705 = ORIENTED_EDGE ( 'NONE', *, *, #9539, .F. ) ;
#7706 = CIRCLE ( 'NONE', #28647, 2.000000000000001776 ) ;
#7707 = DIRECTION ( 'NONE',  ( 0.000000000000000000, 0.000000000000000000, 1.000000000000000000 ) ) ;
#7708 = CARTESIAN_POINT ( 'NONE',  ( 57.99999662536843914, -34.64101615137759893, 12.50000000000000000 ) ) ;
#7709 = CYLINDRICAL_SURFACE ( 'NONE', #21484, 25.00000000000000000 ) ;
#7710 = VERTEX_POINT ( 'NONE', #418 ) ;
#7711 = ORIENTED_EDGE ( 'NONE', *, *, #28011, .T. ) ;
#7712 = CIRCLE ( 'NONE', #24479, 2.000000000000001776 ) ;
#7713 = AXIS2_PLACEMENT_3D ( 'NONE', #7381, #10009, #7210 ) ;
#7714 = VERTEX_POINT ( 'NONE', #26304 ) ;
#7715 = CARTESIAN_POINT ( 'NONE',  ( 84.99999662536832545, 25.98076211353319565, -9.999999999999998224 ) ) ;
#7716 = ADVANCED_FACE ( 'NONE', ( #29092 ), #11850, .F. ) ;
#7717 = DIRECTION ( 'NONE',  ( 0.000000000000000000, 0.000000000000000000, 1.000000000000000000 ) ) ;
#7718 = B_SPLINE_CURVE_WITH_KNOTS ( 'NONE', 3,
 ( #1285, #6907, #10460, #24722, #29777, #18351, #4292, #32789 ),
 .UNSPECIFIED., .F., .F.,
 ( 4, 2, 2, 4 ),
 ( 2.451332856832783740E-07, 0.001475502392055661870, 0.002213131021440650163, 0.002950759650825637587 ),
 .UNSPECIFIED. ) ;
#7719 = DIRECTION ( 'NONE',  ( 0.000000000000000000, 0.000000000000000000, -1.000000000000000000 ) ) ;
#7720 = CARTESIAN_POINT ( 'NONE',  ( 9.999996625368625658, 86.60254037844397601, -5.000000000000000000 ) ) ;
#7721 = DIRECTION ( 'NONE',  ( -0.000000000000000000, -0.000000000000000000, -1.000000000000000000 ) ) ;
#7722 = ADVANCED_FACE ( 'NONE', ( #17660 ), #26472, .F. ) ;
#7723 = EDGE_LOOP ( 'NONE', ( #7155, #8906 ) ) ;
#7724 = DIRECTION ( 'NONE',  ( -1.000000000000000000, 0.000000000000000000, 0.000000000000000000 ) ) ;
#7725 = PRODUCT_DEFINITION_SHAPE ( 'NONE', 'NONE',  #37119 ) ;
#7726 = FACE_OUTER_BOUND ( 'NONE', #5599, .T. ) ;
#7727 = CIRCLE ( 'NONE', #5942, 2.000000000000001776 ) ;
#7728 =( NAMED_UNIT ( * ) SI_UNIT ( $, .STERADIAN. ) SOLID_ANGLE_UNIT ( ) );
#7729 = VERTEX_POINT ( 'NONE', #20652 ) ;
#7730 = FACE_OUTER_BOUND ( 'NONE', #3162, .T. ) ;
#7731 = EDGE_CURVE ( 'NONE', #3751, #5803, #35366, .T. ) ;
#7732 = AXIS2_PLACEMENT_3D ( 'NONE', #34785, #20499, #6642 ) ;
#7733 = CARTESIAN_POINT ( 'NONE',  ( 21.99999662536859191, 69.28203230275516944, -5.000000000000000000 ) ) ;
#7734 = EDGE_LOOP ( 'NONE', ( #7189, #32021 ) ) ;
#7735 = ORIENTED_EDGE ( 'NONE', *, *, #28390, .F. ) ;
#7736 = EDGE_CURVE ( 'NONE', #6161, #12760, #10796, .T. ) ;
#7737 = CIRCLE ( 'NONE', #23283, 3.000000000000003553 ) ;
#7738 = PLANE ( 'NONE',  #36680 ) ;
#7739 = DIRECTION ( 'NONE',  ( 1.000000000000000000, 0.000000000000000000, 0.000000000000000000 ) ) ;
#7740 = CARTESIAN_POINT ( 'NONE',  ( 0.000000000000000000, 55.00000000000000000, -5.000000000000000888 ) ) ;
#7741 = ORIENTED_EDGE ( 'NONE', *, *, #34102, .T. ) ;
#7742 = VERTEX_POINT ( 'NONE', #9422 ) ;
#7743 = MANIFOLD_SOLID_BREP ( 'EndChamfer', #18386 ) ;
#7744 = AXIS2_PLACEMENT_3D ( 'NONE', #31996, #12518, #6714 ) ;
#7745 = CYLINDRICAL_SURFACE ( 'NONE', #3308, 1.999999999999998224 ) ;
#7746 = AXIS2_PLACEMENT_3D ( 'NONE', #37084, #11385, #34268 ) ;
#7747 = EDGE_LOOP ( 'NONE', ( #28344, #23095 ) ) ;
#7748 = AXIS2_PLACEMENT_3D ( 'NONE', #9825, #21260, #1388 ) ;
#7749 = DIRECTION ( 'NONE',  ( 0.000000000000000000, 0.000000000000000000, 1.000000000000000000 ) ) ;
#7750 = VERTEX_POINT ( 'NONE', #6421 ) ;
#7751 = B_SPLINE_CURVE_WITH_KNOTS ( 'NONE', 3,
 ( #1375, #35354, #26693, #3816, #35154, #12794 ),
 .UNSPECIFIED., .F., .F.,
 ( 4, 2, 4 ),
 ( 0.000000000000000000, 0.0002514304509865740098, 0.0005028609019731480195 ),
 .UNSPECIFIED. ) ;
#7752 = EDGE_LOOP ( 'NONE', ( #20234, #36014 ) ) ;
#7753 = ADVANCED_FACE ( 'NONE', ( #15046 ), #20854, .F. ) ;
#7754 = AXIS2_PLACEMENT_3D ( 'NONE', #21395, #4518, #29832 ) ;
#7755 = CARTESIAN_POINT ( 'NONE',  ( -13.00000337463125710, -77.94228634059960825, -5.000000000000000000 ) ) ;
#7756 = AXIS2_PLACEMENT_3D ( 'NONE', #8172, #1981, #28229 ) ;
#7757 = CARTESIAN_POINT ( 'NONE',  ( 72.99999662536836809, 8.660254037844394404, 17.49999999999999645 ) ) ;
#7758 = ORIENTED_EDGE ( 'NONE', *, *, #2980, .F. ) ;
#7759 = ORIENTED_EDGE ( 'NONE', *, *, #17447, .T. ) ;
#7760 = DIRECTION ( 'NONE',  ( -0.000000000000000000, -0.000000000000000000, 1.000000000000000000 ) ) ;
#7761 = CIRCLE ( 'NONE', #29882, 2.000000000000000000 ) ;
#7762 = CARTESIAN_POINT ( 'NONE',  ( -82.00000337463094979, -2.404119930384582903E-14, -9.999999999999998224 ) ) ;
#7763 = EDGE_CURVE ( 'NONE', #13023, #24009, #10185, .T. ) ;
#7764 = CARTESIAN_POINT ( 'NONE',  ( 5.000000000000000000, 24.49489742783178414, 15.00000000000000000 ) ) ;
#7765 = CARTESIAN_POINT ( 'NONE',  ( -5.253368672218637236, 3.033033817057754877, -4.359491423763649287 ) ) ;
#7766 = ORIENTED_EDGE ( 'NONE', *, *, #14817, .F. ) ;
#7767 = DIRECTION ( 'NONE',  ( -0.000000000000000000, -0.000000000000000000, 1.000000000000000000 ) ) ;
#7768 = EDGE_CURVE ( 'NONE', #7356, #9425, #23111, .T. ) ;
#7769 = FACE_BOUND ( 'NONE', #5752, .T. ) ;
#7770 = CYLINDRICAL_SURFACE ( 'NONE', #30980, 2.000000000000001776 ) ;
#7771 = DIRECTION ( 'NONE',  ( -1.000000000000000000, 0.000000000000000000, 0.000000000000000000 ) ) ;
#7772 = CARTESIAN_POINT ( 'NONE',  ( -82.00000337463094979, 34.64101615137757051, -5.000000000000000000 ) ) ;
#7773 = AXIS2_PLACEMENT_3D ( 'NONE', #7095, #12882, #18542 ) ;
#7774 = CARTESIAN_POINT ( 'NONE',  ( -62.00000337463104927, 51.96152422706639129, 17.49999999999999645 ) ) ;
#7775 = CARTESIAN_POINT ( 'NONE',  ( 77.99999662536833966, -3.224517592124143893E-15, 17.49999999999999645 ) ) ;
#7776 = CYLINDRICAL_SURFACE ( 'NONE', #3189, 2.000000000000001776 ) ;
#7777 = ORIENTED_EDGE ( 'NONE', *, *, #32205, .F. ) ;
#7778 = CARTESIAN_POINT ( 'NONE',  ( 49.99999662536846756, 69.28203230275516944, -9.999999999999998224 ) ) ;
#7779 = DIRECTION ( 'NONE',  ( 0.000000000000000000, 0.000000000000000000, 1.000000000000000000 ) ) ;
#7780 = AXIS2_PLACEMENT_3D ( 'NONE', #15968, #9962, #7168 ) ;
#7781 = DIRECTION ( 'NONE',  ( 1.000000000000000000, 0.000000000000000000, 0.000000000000000000 ) ) ;
#7782 = ORIENTED_EDGE ( 'NONE', *, *, #14774, .T. ) ;
#7783 = ORIENTED_EDGE ( 'NONE', *, *, #17926, .F. ) ;
#7784 = ORIENTED_EDGE ( 'NONE', *, *, #36651, .F. ) ;
#7785 = EDGE_CURVE ( 'NONE', #28919, #4855, #3617, .T. ) ;
#7786 = AXIS2_PLACEMENT_3D ( 'NONE', #23707, #12442, #6649 ) ;
#7787 = DIRECTION ( 'NONE',  ( 0.000000000000000000, 1.000000000000000000, -1.224646799147353207E-16 ) ) ;
#7788 = LINE ( 'NONE', #24844, #8873 ) ;
#7789 = AXIS2_PLACEMENT_3D ( 'NONE', #36352, #16459, #15908 ) ;
#7790 = ORIENTED_EDGE ( 'NONE', *, *, #32607, .T. ) ;
#7791 = DIRECTION ( 'NONE',  ( -1.000000000000000000, 0.000000000000000000, 0.000000000000000000 ) ) ;
#7792 = DIRECTION ( 'NONE',  ( -0.000000000000000000, -0.000000000000000000, 1.000000000000000000 ) ) ;
#7793 = ORIENTED_EDGE ( 'NONE', *, *, #32083, .F. ) ;
#7794 = FACE_BOUND ( 'NONE', #9244, .T. ) ;
#7795 = EDGE_LOOP ( 'NONE', ( #28378, #32682 ) ) ;
#7796 = FACE_OUTER_BOUND ( 'NONE', #31359, .T. ) ;
#7797 = CIRCLE ( 'NONE', #28742, 2.000000000000001776 ) ;
#7798 = EDGE_CURVE ( 'NONE', #3339, #406, #31729, .T. ) ;
#7799 = CARTESIAN_POINT ( 'NONE',  ( -1.653121499799246497, 4.819072548984005167, -5.948595712916174172 ) ) ;
#7800 = CYLINDRICAL_SURFACE ( 'NONE', #28719, 2.000000000000001776 ) ;
#7801 = CARTESIAN_POINT ( 'NONE',  ( -45.00000337463111322, -77.94228634059960825, 17.49999999999999645 ) ) ;
#7802 = VECTOR ( 'NONE', #11487, 1000.000000000000000 ) ;
#7803 = ADVANCED_FACE ( 'NONE', ( #3235 ), #26108, .F. ) ;
#7804 = VERTEX_POINT ( 'NONE', #6226 ) ;
#7805 = DIRECTION ( 'NONE',  ( 1.000000000000000000, 0.000000000000000000, 0.000000000000000000 ) ) ;
#7806 = VECTOR ( 'NONE', #15172, 1000.000000000000000 ) ;
#7807 = SHAPE_DEFINITION_REPRESENTATION ( #28906, #26771 ) ;
#7808 = EDGE_CURVE ( 'NONE', #33601, #10938, #15557, .T. ) ;
#7809 = DIRECTION ( 'NONE',  ( 1.000000000000000000, 0.000000000000000000, 0.000000000000000000 ) ) ;
#7810 = LINE ( 'NONE', #13804, #20624 ) ;
#7811 = AXIS2_PLACEMENT_3D ( 'NONE', #3714, #21135, #20565 ) ;
#7812 = VERTEX_POINT ( 'NONE', #4178 ) ;
#7813 = FACE_BOUND ( 'NONE', #15099, .T. ) ;
#7814 = DIRECTION ( 'NONE',  ( -0.000000000000000000, -0.000000000000000000, 1.000000000000000000 ) ) ;
#7816 = ORIENTED_EDGE ( 'NONE', *, *, #35245, .F. ) ;
#7815 = EDGE_CURVE ( 'NONE', #35811, #32676, #3008, .T. ) ;
#7817 = CYLINDRICAL_SURFACE ( 'NONE', #21394, 2.000000000000001776 ) ;
#7818 = EDGE_CURVE ( 'NONE', #28919, #24399, #1523, .T. ) ;
#7819 = AXIS2_PLACEMENT_3D ( 'NONE', #16068, #7620, #36118 ) ;
#7820 = FACE_OUTER_BOUND ( 'NONE', #13607, .T. ) ;
#7821 = DIRECTION ( 'NONE',  ( -1.000000000000000000, 0.000000000000000000, 0.000000000000000000 ) ) ;
#7822 = EDGE_CURVE ( 'NONE', #14745, #28198, #27205, .T. ) ;
#7823 = ORIENTED_EDGE ( 'NONE', *, *, #8229, .F. ) ;
#7824 = ORIENTED_EDGE ( 'NONE', *, *, #35676, .F. ) ;
#7825 = VECTOR ( 'NONE', #6784, 1000.000000000000000 ) ;
#7826 = DIRECTION ( 'NONE',  ( 0.000000000000000000, 0.000000000000000000, 1.000000000000000000 ) ) ;
#7827 = DIRECTION ( 'NONE',  ( 1.000000000000000000, 0.000000000000000000, 0.000000000000000000 ) ) ;
#7828 = EDGE_CURVE ( 'NONE', #18936, #11967, #6590, .T. ) ;
#7829 = EDGE_CURVE ( 'NONE', #32102, #12218, #31131, .T. ) ;
#7830 = DIRECTION ( 'NONE',  ( 0.000000000000000000, 0.000000000000000000, 1.000000000000000000 ) ) ;
#7831 = VERTEX_POINT ( 'NONE', #18212 ) ;
#7832 = ORIENTED_EDGE ( 'NONE', *, *, #14523, .T. ) ;
#7833 = EDGE_CURVE ( 'NONE', #25354, #20763, #34147, .T. ) ;
#7834 = CIRCLE ( 'NONE', #34756, 2.000000000000001776 ) ;
#7835 = DIRECTION ( 'NONE',  ( 0.000000000000000000, 0.000000000000000000, 1.000000000000000000 ) ) ;
#7836 = CARTESIAN_POINT ( 'NONE',  ( 32.99999662536853862, 77.94228634059959404, 12.50000000000000000 ) ) ;
#7837 = DIRECTION ( 'NONE',  ( 1.000000000000000000, 0.000000000000000000, 0.000000000000000000 ) ) ;
#7838 = CARTESIAN_POINT ( 'NONE',  ( -107.2750611683612192, 48.40478642138986487, 32.50000000000000711 ) ) ;
#7839 = ORIENTED_EDGE ( 'NONE', *, *, #25113, .T. ) ;
#7840 = ORIENTED_EDGE ( 'NONE', *, *, #2780, .T. ) ;
#7841 = FACE_OUTER_BOUND ( 'NONE', #10741, .T. ) ;
#7842 = FACE_OUTER_BOUND ( 'NONE', #30536, .T. ) ;
#7843 = ORIENTED_EDGE ( 'NONE', *, *, #33232, .F. ) ;
#7844 = CARTESIAN_POINT ( 'NONE',  ( 0.2117491801717968081, -5.895756138069173424, -4.027903350935069682 ) ) ;
#7845 = ORIENTED_EDGE ( 'NONE', *, *, #35526, .T. ) ;
#7846 = DIRECTION ( 'NONE',  ( 1.000000000000000000, 0.000000000000000000, 0.000000000000000000 ) ) ;
#7847 = EDGE_CURVE ( 'NONE', #23924, #36749, #18614, .T. ) ;
#7848 = DIRECTION ( 'NONE',  ( 1.000000000000000000, 0.000000000000000000, 0.000000000000000000 ) ) ;
#7849 = EDGE_CURVE ( 'NONE', #5113, #30348, #28134, .T. ) ;
#7850 = CARTESIAN_POINT ( 'NONE',  ( 41.99999662536853151, -69.28203230275519786, 17.49999999999999645 ) ) ;
#7851 = ORIENTED_EDGE ( 'NONE', *, *, #5041, .T. ) ;
#7852 = CARTESIAN_POINT ( 'NONE',  ( 0.000000000000000000, 0.000000000000000000, 0.000000000000000000 ) ) ;
#7853 = CARTESIAN_POINT ( 'NONE',  ( 6.249999999999998224, 0.000000000000000000, 0.000000000000000000 ) ) ;
#7854 = CARTESIAN_POINT ( 'NONE',  ( -83.00000337463092137, 8.660254037844389075, -9.999999999999998224 ) ) ;
#7855 = CARTESIAN_POINT ( 'NONE',  ( 0.000000000000000000, 0.000000000000000000, -5.000000000000000000 ) ) ;
#7856 = CONICAL_SURFACE ( 'NONE', #29977, 20.00000000000001066, 0.1396263401595466691 ) ;
#7857 = ORIENTED_EDGE ( 'NONE', *, *, #26589, .F. ) ;
#7858 = DIRECTION ( 'NONE',  ( 1.000000000000000000, 0.000000000000000000, 0.000000000000000000 ) ) ;
#7859 = EDGE_CURVE ( 'NONE', #11646, #11785, #16773, .T. ) ;
#7860 = DIRECTION ( 'NONE',  ( 1.000000000000000000, 0.000000000000000000, 0.000000000000000000 ) ) ;
#7861 = CARTESIAN_POINT ( 'NONE',  ( -65.00000000000000000, 0.000000000000000000, -49.86348611802629449 ) ) ;
#7862 = ORIENTED_EDGE ( 'NONE', *, *, #5340, .T. ) ;
#7863 = ORIENTED_EDGE ( 'NONE', *, *, #23640, .T. ) ;
#7864 = CARTESIAN_POINT ( 'NONE',  ( -85.00000337463092137, 25.98076211353317433, -9.999999999999998224 ) ) ;
#7865 = ORIENTED_EDGE ( 'NONE', *, *, #27254, .F. ) ;
#7866 = CARTESIAN_POINT ( 'NONE',  ( -5.000000000000000888, -2.488288133785819589, -1.689848211693934621 ) ) ;
#7867 = DIRECTION ( 'NONE',  ( 0.000000000000000000, 0.000000000000000000, 1.000000000000000000 ) ) ;
#7868 = EDGE_CURVE ( 'NONE', #21906, #26245, #30407, .T. ) ;
#7869 = EDGE_CURVE ( 'NONE', #32183, #23730, #3975, .T. ) ;
#7870 = CARTESIAN_POINT ( 'NONE',  ( -47.04203867989546950, 43.19957991610416315, 12.49999999999999822 ) ) ;
#7871 = ADVANCED_FACE ( 'NONE', ( #15421 ), #19770, .T. ) ;
#7872 = EDGE_CURVE ( 'NONE', #36949, #2973, #35942, .T. ) ;
#7873 = DIRECTION ( 'NONE',  ( 0.000000000000000000, 0.000000000000000000, 1.000000000000000000 ) ) ;
#7874 = CARTESIAN_POINT ( 'NONE',  ( 105.1746053637160117, -37.32370766915258287, 32.49999999999999289 ) ) ;
#7875 = FACE_OUTER_BOUND ( 'NONE', #32435, .T. ) ;
#7876 = AXIS2_PLACEMENT_3D ( 'NONE', #21010, #6751, #18388 ) ;
#7877 = DIRECTION ( 'NONE',  ( -0.000000000000000000, 0.8660254037844420383, -0.4999999999999945599 ) ) ;
#7878 = DIRECTION ( 'NONE',  ( 0.000000000000000000, 0.000000000000000000, 1.000000000000000000 ) ) ;
#7879 = ORIENTED_EDGE ( 'NONE', *, *, #1173, .T. ) ;
#7880 = VERTEX_POINT ( 'NONE', #15219 ) ;
#7881 = SURFACE_SIDE_STYLE ('',( #33173 ) ) ;
#7882 = DIRECTION ( 'NONE',  ( -0.000000000000000000, 0.000000000000000000, -1.000000000000000000 ) ) ;
#7883 = FACE_OUTER_BOUND ( 'NONE', #8028, .T. ) ;
#7884 = DIRECTION ( 'NONE',  ( 0.000000000000000000, 0.000000000000000000, -1.000000000000000000 ) ) ;
#7885 = ORIENTED_EDGE ( 'NONE', *, *, #22160, .T. ) ;
#7886 = CARTESIAN_POINT ( 'NONE',  ( 5.000000000000000888, -2.488288133785820033, -1.689848211693934621 ) ) ;
#7887 = ORIENTED_EDGE ( 'NONE', *, *, #10930, .T. ) ;
#7888 = DIRECTION ( 'NONE',  ( 0.000000000000000000, -0.4999999999999990563, 0.8660254037844391517 ) ) ;
#7889 = VERTEX_POINT ( 'NONE', #4539 ) ;
#7890 = EDGE_CURVE ( 'NONE', #2354, #19731, #2844, .T. ) ;
#7891 = DIRECTION ( 'NONE',  ( -1.000000000000000000, 0.000000000000000000, 0.000000000000000000 ) ) ;
#7892 = DIRECTION ( 'NONE',  ( -1.000000000000000000, 0.000000000000000000, -0.000000000000000000 ) ) ;
#7893 = CIRCLE ( 'NONE', #36641, 2.000000000000001776 ) ;
#7894 = LINE ( 'NONE', #11053, #5912 ) ;
#7895 = ORIENTED_EDGE ( 'NONE', *, *, #11684, .F. ) ;
#7896 = ORIENTED_EDGE ( 'NONE', *, *, #15056, .T. ) ;
#7897 = AXIS2_PLACEMENT_3D ( 'NONE', #18015, #12362, #3392 ) ;
#7898 = ORIENTED_EDGE ( 'NONE', *, *, #7480, .T. ) ;
#7899 = DIRECTION ( 'NONE',  ( 0.000000000000000000, 0.5000000000000013323, 0.8660254037844378194 ) ) ;
#7900 = LINE ( 'NONE', #2070, #18571 ) ;
#7901 = CARTESIAN_POINT ( 'NONE',  ( 79.99999662536833966, 17.32050807568879236, -5.000000000000000000 ) ) ;
#7902 = LINE ( 'NONE', #4732, #11489 ) ;
#7903 = CARTESIAN_POINT ( 'NONE',  ( 5.244936596612841839, -2.071425061673250578, -4.180295101352479392 ) ) ;
#7904 = ORIENTED_EDGE ( 'NONE', *, *, #21702, .F. ) ;
#7905 = CARTESIAN_POINT ( 'NONE',  ( 0.000000000000000000, -95.00000000000001421, 27.50000000000000000 ) ) ;
#7906 = CARTESIAN_POINT ( 'NONE',  ( 0.000000000000000000, 0.000000000000000000, 2.266666666666666607 ) ) ;
#7907 = EDGE_CURVE ( 'NONE', #7234, #13265, #26977, .T. ) ;
#7908 = DIRECTION ( 'NONE',  ( 0.000000000000000000, 0.000000000000000000, 1.000000000000000000 ) ) ;
#7909 = VERTEX_POINT ( 'NONE', #35666 ) ;
#7910 = CARTESIAN_POINT ( 'NONE',  ( 47.04203867989577503, -43.19957991610382919, 12.49999999999999822 ) ) ;
#7911 = DIRECTION ( 'NONE',  ( 0.4999999999999924505, -0.8660254037844429265, 0.000000000000000000 ) ) ;
#7912 = ORIENTED_EDGE ( 'NONE', *, *, #7239, .F. ) ;
#7913 = ORIENTED_EDGE ( 'NONE', *, *, #20003, .T. ) ;
#7914 = FACE_OUTER_BOUND ( 'NONE', #66, .T. ) ;
#7915 = CIRCLE ( 'NONE', #23485, 2.000000000000001776 ) ;
#7916 = DIRECTION ( 'NONE',  ( 1.000000000000000000, 0.000000000000000000, 0.000000000000000000 ) ) ;
#7917 = DIRECTION ( 'NONE',  ( 1.000000000000000000, 0.000000000000000000, 0.000000000000000000 ) ) ;
#7918 = CARTESIAN_POINT ( 'NONE',  ( -35.00000337463116296, 77.94228634059957983, -5.000000000000000000 ) ) ;
#7919 = ORIENTED_EDGE ( 'NONE', *, *, #29826, .F. ) ;
#7920 = ORIENTED_EDGE ( 'NONE', *, *, #14566, .F. ) ;
#7921 = FACE_BOUND ( 'NONE', #29967, .T. ) ;
#7922 = ORIENTED_EDGE ( 'NONE', *, *, #24091, .F. ) ;
#7923 = DIRECTION ( 'NONE',  ( 1.000000000000000000, 0.000000000000000000, 0.000000000000000000 ) ) ;
#7924 = ORIENTED_EDGE ( 'NONE', *, *, #16308, .F. ) ;
#7925 = EDGE_CURVE ( 'NONE', #18009, #24444, #22200, .T. ) ;
#7926 = EDGE_LOOP ( 'NONE', ( #20969, #33170, #11499, #24166 ) ) ;
#7927 = CIRCLE ( 'NONE', #9117, 33.00000000000001421 ) ;
#7928 = CIRCLE ( 'NONE', #742, 2.000000000000001776 ) ;
#7929 = CARTESIAN_POINT ( 'NONE',  ( 29.99999662536857770, -69.28203230275519786, 12.50000000000000000 ) ) ;
#7930 = CARTESIAN_POINT ( 'NONE',  ( 21.99999662536862033, -86.60254037844400443, 17.49999999999999645 ) ) ;
#7931 = ORIENTED_EDGE ( 'NONE', *, *, #21492, .T. ) ;
#7932 = VERTEX_POINT ( 'NONE', #9969 ) ;
#7933 = DIRECTION ( 'NONE',  ( 1.000000000000000000, 0.000000000000000000, 0.000000000000000000 ) ) ;
#7934 = CYLINDRICAL_SURFACE ( 'NONE', #33326, 2.000000000000001776 ) ;
#7935 = DIRECTION ( 'NONE',  ( 0.000000000000000000, 0.000000000000000000, 1.000000000000000000 ) ) ;
#7936 = DIRECTION ( 'NONE',  ( 0.000000000000000000, 0.000000000000000000, 1.000000000000000000 ) ) ;
#7937 = EDGE_CURVE ( 'NONE', #23931, #21264, #10823, .T. ) ;
#7938 = ORIENTED_EDGE ( 'NONE', *, *, #6430, .T. ) ;
#7939 = CARTESIAN_POINT ( 'NONE',  ( -85.00000337463092137, 8.660254037844389075, -9.999999999999998224 ) ) ;
#7940 = AXIS2_PLACEMENT_3D ( 'NONE', #31488, #17066, #5827 ) ;
#7941 = FACE_BOUND ( 'NONE', #11764, .T. ) ;
#7942 = DIRECTION ( 'NONE',  ( -1.000000000000000000, 0.000000000000000000, 0.000000000000000000 ) ) ;
#7943 = PLANE ( 'NONE',  #27968 ) ;
#7944 = DIRECTION ( 'NONE',  ( -1.000000000000000000, 0.000000000000000000, 0.000000000000000000 ) ) ;
#7945 = DIRECTION ( 'NONE',  ( 0.000000000000000000, 0.000000000000000000, 1.000000000000000000 ) ) ;
#7946 = CARTESIAN_POINT ( 'NONE',  ( 49.99999662536846756, 51.96152422706637708, -9.999999999999998224 ) ) ;
#7947 = ADVANCED_FACE ( 'NONE', ( #7175 ), #976, .F. ) ;
#7948 = CARTESIAN_POINT ( 'NONE',  ( -50.00000337463110611, -69.28203230275519786, 12.50000000000000000 ) ) ;
#7949 = ORIENTED_EDGE ( 'NONE', *, *, #19097, .F. ) ;
#7950 = DIRECTION ( 'NONE',  ( 0.000000000000000000, 0.000000000000000000, 1.000000000000000000 ) ) ;
#7951 = DIRECTION ( 'NONE',  ( 0.000000000000000000, 0.000000000000000000, -1.000000000000000000 ) ) ;
#7952 = CYLINDRICAL_SURFACE ( 'NONE', #22928, 2.000000000000001776 ) ;
#7953 = ORIENTED_EDGE ( 'NONE', *, *, #9539, .T. ) ;
#7954 = VECTOR ( 'NONE', #29814, 1000.000000000000000 ) ;
#7955 = ORIENTED_EDGE ( 'NONE', *, *, #10489, .F. ) ;
#7956 = ORIENTED_EDGE ( 'NONE', *, *, #17502, .F. ) ;
#7957 = DIRECTION ( 'NONE',  ( 1.000000000000000000, 0.000000000000000000, 0.000000000000000000 ) ) ;
#7958 = DIRECTION ( 'NONE',  ( 0.000000000000000000, 0.000000000000000000, 1.000000000000000000 ) ) ;
#7959 = ORIENTED_EDGE ( 'NONE', *, *, #11473, .F. ) ;
#7960 = EDGE_CURVE ( 'NONE', #32676, #35811, #7834, .T. ) ;
#7961 = CARTESIAN_POINT ( 'NONE',  ( -90.60231327712325822, -15.97563234535699017, 12.49999999999999822 ) ) ;
#7962 = CIRCLE ( 'NONE', #22951, 95.00000000000001421 ) ;
#7963 = LINE ( 'NONE', #34345, #10543 ) ;
#7964 = ORIENTED_EDGE ( 'NONE', *, *, #18555, .T. ) ;
#7965 = EDGE_CURVE ( 'NONE', #1092, #2403, #34163, .T. ) ;
#7966 = DIRECTION ( 'NONE',  ( 0.000000000000000000, 0.000000000000000000, -1.000000000000000000 ) ) ;
#7967 = VERTEX_POINT ( 'NONE', #33413 ) ;
#7968 = DIRECTION ( 'NONE',  ( 1.000000000000000000, 0.000000000000000000, 0.000000000000000000 ) ) ;
#7969 = ADVANCED_FACE ( 'NONE', ( #2080 ), #10723, .F. ) ;
#7970 = CYLINDRICAL_SURFACE ( 'NONE', #4044, 2.000000000000001776 ) ;
#7971 = DIRECTION ( 'NONE',  ( 1.000000000000000000, 0.000000000000000000, 0.000000000000000000 ) ) ;
#7972 = EDGE_CURVE ( 'NONE', #31059, #4753, #3040, .T. ) ;
#7973 = ORIENTED_EDGE ( 'NONE', *, *, #29463, .T. ) ;
#7974 = CARTESIAN_POINT ( 'NONE',  ( 90.60231327712337190, 15.97563234535636134, -4.999999999999997335 ) ) ;
#7975 = AXIS2_PLACEMENT_3D ( 'NONE', #15622, #20667, #9791 ) ;
#7976 = ITEM_DEFINED_TRANSFORMATION ( 'NONE', 'NONE', #18953,  #21385 ) ;
#7977 = DIRECTION ( 'NONE',  ( 0.000000000000000000, 0.000000000000000000, -1.000000000000000000 ) ) ;
#7978 = LINE ( 'NONE', #19247, #26016 ) ;
#7979 = VECTOR ( 'NONE', #22682, 1000.000000000000000 ) ;
#7980 = EDGE_CURVE ( 'NONE', #25343, #11611, #29951, .T. ) ;
#7981 = ORIENTED_EDGE ( 'NONE', *, *, #367, .F. ) ;
#7982 = DIRECTION ( 'NONE',  ( 1.000000000000000000, 0.000000000000000000, 0.000000000000000000 ) ) ;
#7983 = CARTESIAN_POINT ( 'NONE',  ( -108.3061974404896262, 19.22934205795090534, 32.50000000000000000 ) ) ;
#7984 = ORIENTED_EDGE ( 'NONE', *, *, #16808, .T. ) ;
#7985 = CARTESIAN_POINT ( 'NONE',  ( 34.99999662536855283, -77.94228634059960825, -9.999999999999998224 ) ) ;
#7986 = CYLINDRICAL_SURFACE ( 'NONE', #37046, 2.000000000000001776 ) ;
#7987 = CARTESIAN_POINT ( 'NONE',  ( 34.99999662536855283, 60.62177826491078747, -9.999999999999998224 ) ) ;
#7988 = DIRECTION ( 'NONE',  ( 1.000000000000000000, 0.000000000000000000, 0.000000000000000000 ) ) ;
#7989 = ORIENTED_EDGE ( 'NONE', *, *, #28221, .F. ) ;
#7990 = CIRCLE ( 'NONE', #25948, 2.000000000000001776 ) ;
#7991 = EDGE_LOOP ( 'NONE', ( #27337, #23884, #15327, #25123 ) ) ;
#7992 = CARTESIAN_POINT ( 'NONE',  ( 61.99999662536845335, 34.64101615137759893, 12.50000000000000000 ) ) ;
#7993 = DIRECTION ( 'NONE',  ( 0.000000000000000000, 0.000000000000000000, 1.000000000000000000 ) ) ;
#7994 = DIRECTION ( 'NONE',  ( 1.000000000000000000, 0.000000000000000000, 0.000000000000000000 ) ) ;
#7995 = ADVANCED_FACE ( 'NONE', ( #24978 ), #13516, .F. ) ;
#7996 = ORIENTED_EDGE ( 'NONE', *, *, #27050, .F. ) ;
#7997 = ORIENTED_EDGE ( 'NONE', *, *, #16983, .F. ) ;
#7998 = LINE ( 'NONE', #22425, #2619 ) ;
#7999 = CARTESIAN_POINT ( 'NONE',  ( -4.652319770550016109, 3.087484620012986625, -1.687189089856314217 ) ) ;
#8000 = VECTOR ( 'NONE', #9020, 1000.000000000000000 ) ;
#8001 = ORIENTED_EDGE ( 'NONE', *, *, #20759, .F. ) ;
#8002 = EDGE_CURVE ( 'NONE', #24448, #20171, #36965, .T. ) ;
#8003 = ORIENTED_EDGE ( 'NONE', *, *, #11581, .F. ) ;
#8004 = AXIS2_PLACEMENT_3D ( 'NONE', #28242, #27683, #16266 ) ;
#8005 =( NAMED_UNIT ( * ) PLANE_ANGLE_UNIT ( ) SI_UNIT ( $, .RADIAN. ) );
#8006 = DIRECTION ( 'NONE',  ( 1.000000000000000000, 0.000000000000000000, 0.000000000000000000 ) ) ;
#8007 = ORIENTED_EDGE ( 'NONE', *, *, #13573, .T. ) ;
#8008 = ADVANCED_FACE ( 'NONE', ( #16173 ), #13331, .F. ) ;
#8009 = LINE ( 'NONE', #34264, #13734 ) ;
#8010 = ORIENTED_EDGE ( 'NONE', *, *, #21098, .F. ) ;
#8011 = FACE_BOUND ( 'NONE', #29377, .T. ) ;
#8012 = CONICAL_SURFACE ( 'NONE', #28368, 4.749999999999999112, 0.4572823821333981131 ) ;
#8013 = CARTESIAN_POINT ( 'NONE',  ( 47.99999662536846756, 51.96152422706637708, -9.999999999999998224 ) ) ;
#8014 = CARTESIAN_POINT ( 'NONE',  ( 32.99999662536853862, 77.94228634059959404, 17.49999999999999645 ) ) ;
#8015 = VERTEX_POINT ( 'NONE', #22163 ) ;
#8016 = DIRECTION ( 'NONE',  ( 0.000000000000000000, 0.000000000000000000, 1.000000000000000000 ) ) ;
#8017 = VECTOR ( 'NONE', #31943, 1000.000000000000000 ) ;
#8018 = DIRECTION ( 'NONE',  ( 1.000000000000000000, 0.000000000000000000, 0.000000000000000000 ) ) ;
#8019 = EDGE_CURVE ( 'NONE', #22077, #538, #7214, .T. ) ;
#8020 = DIRECTION ( 'NONE',  ( -0.000000000000000000, -0.000000000000000000, 1.000000000000000000 ) ) ;
#8021 = DIRECTION ( 'NONE',  ( 0.000000000000000000, 0.000000000000000000, 1.000000000000000000 ) ) ;
#8022 = ORIENTED_EDGE ( 'NONE', *, *, #8299, .F. ) ;
#8023 = CARTESIAN_POINT ( 'NONE',  ( 81.99999662536832545, -17.32050807568879591, -5.000000000000000000 ) ) ;
#8024 = CARTESIAN_POINT ( 'NONE',  ( 55.27226924886128501, 77.26562141134559170, 32.50000000000000000 ) ) ;
#8025 = CARTESIAN_POINT ( 'NONE',  ( 57.99999662536844625, 34.64101615137759893, 12.50000000000000000 ) ) ;
#8026 = ORIENTED_EDGE ( 'NONE', *, *, #11674, .F. ) ;
#8027 = AXIS2_PLACEMENT_3D ( 'NONE', #29000, #34838, #6143 ) ;
#8028 = EDGE_LOOP ( 'NONE', ( #35266, #1350, #20276, #7267, #35018 ) ) ;
#8029 = CARTESIAN_POINT ( 'NONE',  ( 33.99999999999986500, -58.88972745734191250, -49.86561046011506448 ) ) ;
#8030 = ORIENTED_EDGE ( 'NONE', *, *, #18531, .F. ) ;
#8031 = CYLINDRICAL_SURFACE ( 'NONE', #30113, 3.000000000000006217 ) ;
#8032 = FACE_OUTER_BOUND ( 'NONE', #13422, .T. ) ;
#8033 = AXIS2_PLACEMENT_3D ( 'NONE', #20629, #3599, #6044 ) ;
#8034 = DIRECTION ( 'NONE',  ( 0.000000000000000000, 0.000000000000000000, 1.000000000000000000 ) ) ;
#8035 = EDGE_CURVE ( 'NONE', #31719, #26481, #19211, .T. ) ;
#8036 = AXIS2_PLACEMENT_3D ( 'NONE', #14818, #12554, #20605 ) ;
#8037 = CARTESIAN_POINT ( 'NONE',  ( 66.99999662536839651, 60.62177826491078747, 17.49999999999999645 ) ) ;
#8038 = DIRECTION ( 'NONE',  ( 0.000000000000000000, 0.000000000000000000, 1.000000000000000000 ) ) ;
#8039 = DIRECTION ( 'NONE',  ( 1.000000000000000000, 0.000000000000000000, 0.000000000000000000 ) ) ;
#8040 = EDGE_CURVE ( 'NONE', #18995, #10128, #16800, .T. ) ;
#8041 = DIRECTION ( 'NONE',  ( 0.000000000000000000, 0.000000000000000000, 1.000000000000000000 ) ) ;
#8042 = DIRECTION ( 'NONE',  ( 0.000000000000000000, -0.000000000000000000, -1.000000000000000000 ) ) ;
#8043 = ORIENTED_EDGE ( 'NONE', *, *, #14919, .T. ) ;
#8044 = EDGE_CURVE ( 'NONE', #21315, #26861, #31149, .T. ) ;
#8045 = ORIENTED_EDGE ( 'NONE', *, *, #11989, .F. ) ;
#8046 = FACE_OUTER_BOUND ( 'NONE', #23768, .T. ) ;
#8047 = DIRECTION ( 'NONE',  ( -0.000000000000000000, -0.000000000000000000, -1.000000000000000000 ) ) ;
#8048 = DIRECTION ( 'NONE',  ( -0.000000000000000000, -0.000000000000000000, -1.000000000000000000 ) ) ;
#8049 = AXIS2_PLACEMENT_3D ( 'NONE', #26425, #31679, #23252 ) ;
#8050 = DIRECTION ( 'NONE',  ( 0.000000000000000000, 0.000000000000000000, 1.000000000000000000 ) ) ;
#8051 = ADVANCED_FACE ( 'NONE', ( #7726 ), #10525, .F. ) ;
#8052 = ORIENTED_EDGE ( 'NONE', *, *, #34402, .T. ) ;
#8053 = UNCERTAINTY_MEASURE_WITH_UNIT (LENGTH_MEASURE( 1.000000000000000082E-05 ), #16328, 'distance_accuracy_value', 'NONE');
#8054 = EDGE_CURVE ( 'NONE', #34770, #10069, #6614, .T. ) ;
#8055 = AXIS2_PLACEMENT_3D ( 'NONE', #35184, #20362, #11719 ) ;
#8056 = CARTESIAN_POINT ( 'NONE',  ( 5.000000000000000000, -0.9645339558193165574, -0.6919071587033235327 ) ) ;
#8057 = VERTEX_POINT ( 'NONE', #16894 ) ;
#8058 = ORIENTED_EDGE ( 'NONE', *, *, #22695, .F. ) ;
#8059 = DIRECTION ( 'NONE',  ( -0.9396926207859139790, 0.000000000000000000, -0.3420201433256533918 ) ) ;
#8060 = ORIENTED_EDGE ( 'NONE', *, *, #25601, .T. ) ;
#8061 = ADVANCED_FACE ( 'NONE', ( #10893 ), #2637, .F. ) ;
#8062 =( LENGTH_UNIT ( ) NAMED_UNIT ( * ) SI_UNIT ( .MILLI., .METRE. ) );
#8063 = DIRECTION ( 'NONE',  ( 0.000000000000000000, 0.000000000000000000, 1.000000000000000000 ) ) ;
#8064 = AXIS2_PLACEMENT_3D ( 'NONE', #12895, #1460, #15547 ) ;
#8065 = AXIS2_PLACEMENT_3D ( 'NONE', #4716, #2054, #13490 ) ;
#8066 = ADVANCED_FACE ( 'NONE', ( #21968 ), #36579, .F. ) ;
#8067 = CARTESIAN_POINT ( 'NONE',  ( -50.00000337463112032, -51.96152422706641971, -5.000000000000000000 ) ) ;
#8068 = EDGE_CURVE ( 'NONE', #18257, #19938, #4430, .T. ) ;
#8069 = VECTOR ( 'NONE', #10614, 1000.000000000000000 ) ;
#8070 = DIRECTION ( 'NONE',  ( -1.000000000000000000, -0.000000000000000000, -0.000000000000000000 ) ) ;
#8071 = EDGE_CURVE ( 'NONE', #21230, #13656, #20391, .T. ) ;
#8072 = ORIENTED_EDGE ( 'NONE', *, *, #8192, .F. ) ;
#8073 = ORIENTED_EDGE ( 'NONE', *, *, #27203, .F. ) ;
#8074 = ORIENTED_EDGE ( 'NONE', *, *, #16870, .T. ) ;
#8075 = ORIENTED_EDGE ( 'NONE', *, *, #21339, .F. ) ;
#8076 = ORIENTED_EDGE ( 'NONE', *, *, #709, .F. ) ;
#8078 = DIRECTION ( 'NONE',  ( 0.000000000000000000, 0.000000000000000000, 1.000000000000000000 ) ) ;
#8077 = AXIS2_PLACEMENT_3D ( 'NONE', #20063, #3025, #11800 ) ;
#8079 = CYLINDRICAL_SURFACE ( 'NONE', #11384, 2.000000000000000000 ) ;
#8080 = CIRCLE ( 'NONE', #9892, 2.000000000000001776 ) ;
#8081 = CARTESIAN_POINT ( 'NONE',  ( 4.166666666666666963, -3.367876570272838155, -3.818275046351167212 ) ) ;
#8082 = DIRECTION ( 'NONE',  ( 0.000000000000000000, 0.000000000000000000, 1.000000000000000000 ) ) ;
#8083 = CARTESIAN_POINT ( 'NONE',  ( 32.99999662536855283, 60.62177826491078747, -5.000000000000000000 ) ) ;
#8084 = ORIENTED_EDGE ( 'NONE', *, *, #19887, .F. ) ;
#8085 = CARTESIAN_POINT ( 'NONE',  ( -65.00000337463102085, 60.62177826491077326, -9.999999999999998224 ) ) ;
#8086 = CIRCLE ( 'NONE', #36218, 2.000000000000001776 ) ;
#8087 = DIRECTION ( 'NONE',  ( -0.000000000000000000, -0.000000000000000000, 1.000000000000000000 ) ) ;
#8088 = CARTESIAN_POINT ( 'NONE',  ( 37.99999662536853151, 69.28203230275518365, -9.999999999999998224 ) ) ;
#8089 = EDGE_LOOP ( 'NONE', ( #3191, #17433, #35199, #9958 ) ) ;
#8090 = DIRECTION ( 'NONE',  ( 0.4999999999999919509, -0.8660254037844432595, 0.000000000000000000 ) ) ;
#8091 = CARTESIAN_POINT ( 'NONE',  ( -37.50000000000000000, 103.4105893997321743, -11.00000000000000355 ) ) ;
#8092 = VECTOR ( 'NONE', #22649, 1000.000000000000000 ) ;
#8093 = EDGE_LOOP ( 'NONE', ( #31856, #10527, #34513, #31870 ) ) ;
#8094 = VECTOR ( 'NONE', #26334, 1000.000000000000000 ) ;
#8095 = VERTEX_POINT ( 'NONE', #26257 ) ;
#8096 = DIRECTION ( 'NONE',  ( -0.6439740589782688707, 0.7650473262243671080, 0.000000000000000000 ) ) ;
#8097 = FACE_OUTER_BOUND ( 'NONE', #31714, .T. ) ;
#8098 = DIRECTION ( 'NONE',  ( -0.000000000000000000, 0.000000000000000000, 1.000000000000000000 ) ) ;
#8099 = ORIENTED_EDGE ( 'NONE', *, *, #32739, .T. ) ;
#8100 = ORIENTED_EDGE ( 'NONE', *, *, #32186, .F. ) ;
#8101 = LINE ( 'NONE', #5105, #11706 ) ;
#8102 = CIRCLE ( 'NONE', #35051, 2.000000000000001776 ) ;
#8103 = VERTEX_POINT ( 'NONE', #17071 ) ;
#8104 = AXIS2_PLACEMENT_3D ( 'NONE', #35168, #20703, #9655 ) ;
#8105 = CARTESIAN_POINT ( 'NONE',  ( -50.00000337463110611, -69.28203230275519786, -5.000000000000000000 ) ) ;
#8106 = ORIENTED_EDGE ( 'NONE', *, *, #24579, .F. ) ;
#8107 = CIRCLE ( 'NONE', #30260, 2.000000000000001776 ) ;
#8108 = AXIS2_PLACEMENT_3D ( 'NONE', #30527, #10833, #19102 ) ;
#8109 = EDGE_LOOP ( 'NONE', ( #154, #18243, #8834, #24639 ) ) ;
#8110 = AXIS2_PLACEMENT_3D ( 'NONE', #21881, #32962, #7449 ) ;
#8111 = DIRECTION ( 'NONE',  ( 1.000000000000000000, 0.000000000000000000, 0.000000000000000000 ) ) ;
#8112 = DIRECTION ( 'NONE',  ( 0.000000000000000000, 0.000000000000000000, 1.000000000000000000 ) ) ;
#8113 = ADVANCED_FACE ( 'NONE', ( #20604 ), #17443, .T. ) ;
#8114 = EDGE_LOOP ( 'NONE', ( #36553, #21356, #12693, #23015 ) ) ;
#8115 = VERTEX_POINT ( 'NONE', #14273 ) ;
#8116 = CARTESIAN_POINT ( 'NONE',  ( -68.00000337463099243, 34.64101615137758472, -5.000000000000000000 ) ) ;
#8117 = AXIS2_PLACEMENT_3D ( 'NONE', #8929, #34810, #12466 ) ;
#8118 = FACE_OUTER_BOUND ( 'NONE', #23135, .T. ) ;
#8119 = CARTESIAN_POINT ( 'NONE',  ( -70.00000337463099243, 17.32050807568877460, -9.999999999999998224 ) ) ;
#8120 = CIRCLE ( 'NONE', #25489, 2.000000000000001776 ) ;
#8121 = DIRECTION ( 'NONE',  ( 1.000000000000000000, 0.000000000000000000, 0.000000000000000000 ) ) ;
#8122 = ORIENTED_EDGE ( 'NONE', *, *, #25808, .F. ) ;
#8123 = CYLINDRICAL_SURFACE ( 'NONE', #24948, 3.000000000000005773 ) ;
#8124 = FACE_BOUND ( 'NONE', #29413, .T. ) ;
#8125 = LINE ( 'NONE', #19569, #12381 ) ;
#8126 = DIRECTION ( 'NONE',  ( -0.000000000000000000, -0.000000000000000000, -1.000000000000000000 ) ) ;
#8127 = CARTESIAN_POINT ( 'NONE',  ( -48.00000337463110611, -69.28203230275519786, -9.999999999999998224 ) ) ;
#8128 = CARTESIAN_POINT ( 'NONE',  ( 37.50000000000000000, 103.4105893997321743, -19.99999999999999645 ) ) ;
#8129 = DIRECTION ( 'NONE',  ( 0.000000000000000000, 0.000000000000000000, 1.000000000000000000 ) ) ;
#8130 = VECTOR ( 'NONE', #6415, 1000.000000000000000 ) ;
#8131 = DIRECTION ( 'NONE',  ( -1.000000000000000000, 0.000000000000000000, 0.000000000000000000 ) ) ;
#8132 = VERTEX_POINT ( 'NONE', #29246 ) ;
#8133 = DIRECTION ( 'NONE',  ( -0.000000000000000000, -0.000000000000000000, 1.000000000000000000 ) ) ;
#8134 = DIRECTION ( 'NONE',  ( 0.000000000000000000, 0.000000000000000000, -1.000000000000000000 ) ) ;
#8135 = CARTESIAN_POINT ( 'NONE',  ( 54.99999662536844625, 43.30127018922198801, -9.999999999999998224 ) ) ;
#8136 = VECTOR ( 'NONE', #14770, 1000.000000000000000 ) ;
#8137 = EDGE_CURVE ( 'NONE', #575, #14128, #14992, .T. ) ;
#8138 = AXIS2_PLACEMENT_3D ( 'NONE', #32829, #26631, #7148 ) ;
#8139 = CIRCLE ( 'NONE', #26705, 3.500000000000003109 ) ;
#8140 = EDGE_CURVE ( 'NONE', #35823, #27946, #5633, .T. ) ;
#8141 = ORIENTED_EDGE ( 'NONE', *, *, #34442, .F. ) ;
#8142 = CIRCLE ( 'NONE', #926, 27.00000000000001421 ) ;
#8143 = ORIENTED_EDGE ( 'NONE', *, *, #21711, .F. ) ;
#8144 = VERTEX_POINT ( 'NONE', #6182 ) ;
#8145 = CARTESIAN_POINT ( 'NONE',  ( -78.00000337463096400, -34.64101615137762025, -5.000000000000000000 ) ) ;
#8146 = LINE ( 'NONE', #30470, #23842 ) ;
#8147 = ORIENTED_EDGE ( 'NONE', *, *, #19080, .F. ) ;
#8148 = CIRCLE ( 'NONE', #17721, 1.999999999999998224 ) ;
#8149 = FACE_OUTER_BOUND ( 'NONE', #20050, .T. ) ;
#8150 = EDGE_CURVE ( 'NONE', #26529, #30363, #29362, .T. ) ;
#8151 = EDGE_LOOP ( 'NONE', ( #16181, #24279, #16352, #31710, #35573, #33440, #7562, #31023 ) ) ;
#8152 = CARTESIAN_POINT ( 'NONE',  ( -35.00000337463117717, -77.94228634059963667, 17.49999999999999645 ) ) ;
#8153 = ORIENTED_EDGE ( 'NONE', *, *, #19407, .T. ) ;
#8154 = CARTESIAN_POINT ( 'NONE',  ( 47.63139720814418610, 27.49999999999988987, -5.000000000000000000 ) ) ;
#8155 = VERTEX_POINT ( 'NONE', #32030 ) ;
#8156 = FACE_OUTER_BOUND ( 'NONE', #26241, .T. ) ;
#8157 = CARTESIAN_POINT ( 'NONE',  ( 51.99999662536848888, -51.96152422706640550, 17.49999999999999645 ) ) ;
#8158 = AXIS2_PLACEMENT_3D ( 'NONE', #34323, #11266, #33965 ) ;
#8159 = EDGE_CURVE ( 'NONE', #10243, #6282, #19795, .T. ) ;
#8160 = VERTEX_POINT ( 'NONE', #16 ) ;
#8161 = DIRECTION ( 'NONE',  ( 0.000000000000000000, 0.000000000000000000, 1.000000000000000000 ) ) ;
#8162 = AXIS2_PLACEMENT_3D ( 'NONE', #32712, #2521, #31203 ) ;
#8163 = CIRCLE ( 'NONE', #24298, 2.000000000000001776 ) ;
#8164 = CONTEXT_DEPENDENT_SHAPE_REPRESENTATION ( #16874, #24785 ) ;
#8165 = CIRCLE ( 'NONE', #31479, 2.000000000000001776 ) ;
#8166 = AXIS2_PLACEMENT_3D ( 'NONE', #21652, #27081, #27260 ) ;
#8167 = DIRECTION ( 'NONE',  ( 0.000000000000000000, -0.5000000000000013323, -0.8660254037844379305 ) ) ;
#8168 = DIRECTION ( 'NONE',  ( -1.000000000000000000, 0.000000000000000000, 0.000000000000000000 ) ) ;
#8169 = CIRCLE ( 'NONE', #32097, 2.000000000000001776 ) ;
#8170 = VERTEX_POINT ( 'NONE', #179 ) ;
#8171 = FACE_OUTER_BOUND ( 'NONE', #706, .T. ) ;
#8172 = CARTESIAN_POINT ( 'NONE',  ( 34.99999662536853862, 77.94228634059959404, 17.49999999999999645 ) ) ;
#8173 = ORIENTED_EDGE ( 'NONE', *, *, #14783, .T. ) ;
#8174 = DIRECTION ( 'NONE',  ( -1.000000000000000000, 0.000000000000000000, 0.000000000000000000 ) ) ;
#8175 = CARTESIAN_POINT ( 'NONE',  ( -51.13139720814380240, 27.50000000000055422, -5.000000000000000000 ) ) ;
#8176 = CARTESIAN_POINT ( 'NONE',  ( 4.999999999999999112, -2.886751345948144198, -3.984345921091770659 ) ) ;
#8177 = DIRECTION ( 'NONE',  ( 1.000000000000000000, 0.000000000000000000, 0.000000000000000000 ) ) ;
#8178 = CIRCLE ( 'NONE', #13580, 2.000000000000001776 ) ;
#8179 = ORIENTED_EDGE ( 'NONE', *, *, #14347, .T. ) ;
#8180 = EDGE_CURVE ( 'NONE', #10442, #31670, #20982, .T. ) ;
#8181 = ORIENTED_EDGE ( 'NONE', *, *, #15653, .F. ) ;
#8182 = CARTESIAN_POINT ( 'NONE',  ( -3.866666666667000651, 5.429267476220137302E-16, 3.400000000000000355 ) ) ;
#8183 = DIRECTION ( 'NONE',  ( 1.000000000000000000, 0.000000000000000000, 0.000000000000000000 ) ) ;
#8184 = EDGE_CURVE ( 'NONE', #36367, #11611, #23446, .T. ) ;
#8185 = CIRCLE ( 'NONE', #12959, 2.000000000000001776 ) ;
#8186 = ORIENTED_EDGE ( 'NONE', *, *, #6122, .F. ) ;
#8187 = ORIENTED_EDGE ( 'NONE', *, *, #17535, .F. ) ;
#8188 = AXIS2_PLACEMENT_3D ( 'NONE', #28102, #474, #36723 ) ;
#8189 = PRODUCT_RELATED_PRODUCT_CATEGORY ( 'part', '', ( #20242 ) ) ;
#8190 = DIRECTION ( 'NONE',  ( 0.000000000000000000, 0.000000000000000000, 1.000000000000000000 ) ) ;
#8191 = CARTESIAN_POINT ( 'NONE',  ( 1.999996625368696490, -86.60254037844400443, -9.999999999999998224 ) ) ;
#8192 = EDGE_CURVE ( 'NONE', #17871, #23793, #15008, .T. ) ;
#8193 = PRODUCT_DEFINITION_FORMATION_WITH_SPECIFIED_SOURCE ( 'ANY', '', #34021, .NOT_KNOWN. ) ;
#8194 = CARTESIAN_POINT ( 'NONE',  ( -85.00000337463092137, -25.98076211353322051, -9.999999999999998224 ) ) ;
#8195 = AXIS2_PLACEMENT_3D ( 'NONE', #4213, #18247, #10206 ) ;
#8196 = AXIS2_PLACEMENT_3D ( 'NONE', #11365, #16984, #10817 ) ;
#8197 = ORIENTED_EDGE ( 'NONE', *, *, #27873, .T. ) ;
#8198 = CIRCLE ( 'NONE', #2789, 2.000000000000001776 ) ;
#8199 = EDGE_LOOP ( 'NONE', ( #27898, #36787, #12123, #35997 ) ) ;
#8200 = DIRECTION ( 'NONE',  ( -0.000000000000000000, -0.000000000000000000, 1.000000000000000000 ) ) ;
#8201 = CIRCLE ( 'NONE', #5202, 2.000000000000001776 ) ;
#8202 = EDGE_CURVE ( 'NONE', #7356, #203, #23380, .T. ) ;
#8203 = CARTESIAN_POINT ( 'NONE',  ( 64.99999662536841072, 25.98076211353318854, -9.999999999999998224 ) ) ;
#8204 = ORIENTED_EDGE ( 'NONE', *, *, #21128, .T. ) ;
#8205 = CARTESIAN_POINT ( 'NONE',  ( 71.99999662536839651, 34.64101615137758472, -5.000000000000000000 ) ) ;
#8206 = ORIENTED_EDGE ( 'NONE', *, *, #18021, .F. ) ;
#8207 = CARTESIAN_POINT ( 'NONE',  ( 69.99999662536841072, 51.96152422706640550, -9.999999999999998224 ) ) ;
#8208 = AXIS2_PLACEMENT_3D ( 'NONE', #16913, #22743, #13909 ) ;
#8209 = DIRECTION ( 'NONE',  ( 1.000000000000000000, 0.000000000000000000, 0.000000000000000000 ) ) ;
#8210 = ORIENTED_EDGE ( 'NONE', *, *, #14171, .F. ) ;
#8211 = CIRCLE ( 'NONE', #24379, 5.000000000000000000 ) ;
#8212 = CARTESIAN_POINT ( 'NONE',  ( -47.63139720814419320, 27.49999999999989697, 10.70000000000000107 ) ) ;
#8213 = AXIS2_PLACEMENT_3D ( 'NONE', #1721, #21600, #18970 ) ;
#8214 = FACE_OUTER_BOUND ( 'NONE', #6745, .T. ) ;
#8215 = EDGE_CURVE ( 'NONE', #35442, #12315, #12154, .T. ) ;
#8216 = CIRCLE ( 'NONE', #17209, 2.000000000000001776 ) ;
#8217 = DIRECTION ( 'NONE',  ( -0.000000000000000000, -0.000000000000000000, 1.000000000000000000 ) ) ;
#8218 = DIRECTION ( 'NONE',  ( -0.000000000000000000, -0.000000000000000000, 1.000000000000000000 ) ) ;
#8219 = CLOSED_SHELL ( 'NONE', ( #14021, #22878, #20690, #14478, #10904, #2569, #18517, #22051, #1329, #28849, #22091, #35522, #14922, #15263, #17435, #11394, #34187, #8591, #30019, #13997, #3356, #8113, #17566, #19990, #13254, #27020, #30785, #29252 ) ) ;
#8220 = ORIENTED_EDGE ( 'NONE', *, *, #32957, .F. ) ;
#8221 = DIRECTION ( 'NONE',  ( 1.000000000000000000, 0.000000000000000000, 0.000000000000000000 ) ) ;
#8222 = CARTESIAN_POINT ( 'NONE',  ( -45.00000337463111322, 77.94228634059959404, -9.999999999999998224 ) ) ;
#8223 = CARTESIAN_POINT ( 'NONE',  ( -80.00000337463094979, 34.64101615137757051, 17.49999999999999645 ) ) ;
#8224 = CIRCLE ( 'NONE', #11207, 33.00000000000001421 ) ;
#8225 = EDGE_CURVE ( 'NONE', #37038, #33197, #31493, .T. ) ;
#8226 = CIRCLE ( 'NONE', #6419, 2.000000000000000000 ) ;
#8227 = ORIENTED_EDGE ( 'NONE', *, *, #7609, .F. ) ;
#8228 = ORIENTED_EDGE ( 'NONE', *, *, #3713, .F. ) ;
#8229 = EDGE_CURVE ( 'NONE', #16622, #27555, #25882, .T. ) ;
#8230 = DIRECTION ( 'NONE',  ( -0.8660254037844380415, 0.5000000000000009992, 0.000000000000000000 ) ) ;
#8231 = VERTEX_POINT ( 'NONE', #26061 ) ;
#8232 = CARTESIAN_POINT ( 'NONE',  ( -17.00000337463125533, -77.94228634059960825, -9.999999999999998224 ) ) ;
#8233 = CIRCLE ( 'NONE', #22013, 2.000000000000001776 ) ;
#8234 = DIRECTION ( 'NONE',  ( 0.000000000000000000, 0.000000000000000000, 1.000000000000000000 ) ) ;
#8235 = CIRCLE ( 'NONE', #29175, 2.541999999999999815 ) ;
#8236 = DIRECTION ( 'NONE',  ( 0.000000000000000000, 0.000000000000000000, -1.000000000000000000 ) ) ;
#8237 = CARTESIAN_POINT ( 'NONE',  ( 56.52018970185258695, -35.83991598322081273, -49.22241343995298024 ) ) ;
#8238 = DIRECTION ( 'NONE',  ( -0.000000000000000000, -0.000000000000000000, 1.000000000000000000 ) ) ;
#8239 = CARTESIAN_POINT ( 'NONE',  ( -96.90588911714331743, -67.77518747868774085, 32.49999999999998579 ) ) ;
#8240 = DIRECTION ( 'NONE',  ( 1.000000000000000000, 0.000000000000000000, 0.000000000000000000 ) ) ;
#8241 = CIRCLE ( 'NONE', #10028, 2.000000000000000000 ) ;
#8242 = LINE ( 'NONE', #17028, #6487 ) ;
#8243 = EDGE_LOOP ( 'NONE', ( #16364, #9105, #17016 ) ) ;
#8244 = ORIENTED_EDGE ( 'NONE', *, *, #31663, .F. ) ;
#8245 = CARTESIAN_POINT ( 'NONE',  ( 69.99999662536839651, 34.64101615137758472, -5.000000000000000000 ) ) ;
#8246 = EDGE_CURVE ( 'NONE', #2447, #21044, #4835, .T. ) ;
#8247 = AXIS2_PLACEMENT_3D ( 'NONE', #14665, #11118, #31732 ) ;
#8248 = DIRECTION ( 'NONE',  ( 1.000000000000000000, 0.000000000000000000, 0.000000000000000000 ) ) ;
#8249 = CARTESIAN_POINT ( 'NONE',  ( 4.999996625368645198, 77.94228634059957983, -9.999999999999998224 ) ) ;
#8250 = CARTESIAN_POINT ( 'NONE',  ( 3.500000000000000888, 55.00000000000000000, 5.000000000000000888 ) ) ;
#8251 = EDGE_LOOP ( 'NONE', ( #30137, #23167, #993, #1088 ) ) ;
#8252 = AXIS2_PLACEMENT_3D ( 'NONE', #14579, #22674, #28827 ) ;
#8253 = AXIS2_PLACEMENT_3D ( 'NONE', #30783, #36441, #8316 ) ;
#8254 = FACE_BOUND ( 'NONE', #5395, .T. ) ;
#8255 = VERTEX_POINT ( 'NONE', #15931 ) ;
#8256 = ORIENTED_EDGE ( 'NONE', *, *, #32963, .T. ) ;
#8257 = LINE ( 'NONE', #5263, #25434 ) ;
#8258 = ORIENTED_EDGE ( 'NONE', *, *, #15040, .F. ) ;
#8259 = AXIS2_PLACEMENT_3D ( 'NONE', #20161, #17521, #18081 ) ;
#8260 = DIRECTION ( 'NONE',  ( 0.000000000000000000, 0.000000000000000000, 1.000000000000000000 ) ) ;
#8261 = DIRECTION ( 'NONE',  ( 0.000000000000000000, 0.000000000000000000, -1.000000000000000000 ) ) ;
#8262 = EDGE_CURVE ( 'NONE', #23780, #22507, #25793, .T. ) ;
#8263 = CIRCLE ( 'NONE', #24430, 2.000000000000001776 ) ;
#8264 = CARTESIAN_POINT ( 'NONE',  ( -4.279621169095561228, 62.97617850287782915, -4.999999999999997335 ) ) ;
#8265 = EDGE_LOOP ( 'NONE', ( #33661, #11069, #20677, #35870 ) ) ;
#8266 = ADVANCED_FACE ( 'NONE', ( #36006 ), #3745, .F. ) ;
#8267 = ORIENTED_EDGE ( 'NONE', *, *, #15163, .T. ) ;
#8268 = AXIS2_PLACEMENT_3D ( 'NONE', #29953, #12508, #18529 ) ;
#8269 = CIRCLE ( 'NONE', #1678, 2.000000000000001776 ) ;
#8270 = ORIENTED_EDGE ( 'NONE', *, *, #4537, .T. ) ;
#8271 = AXIS2_PLACEMENT_3D ( 'NONE', #23011, #17561, #28986 ) ;
#8272 = ADVANCED_FACE ( 'NONE', ( #7131 ), #9740, .F. ) ;
#8273 = VERTEX_POINT ( 'NONE', #1480 ) ;
#8274 = AXIS2_PLACEMENT_3D ( 'NONE', #12354, #3579, #28866 ) ;
#8275 = VERTEX_POINT ( 'NONE', #18173 ) ;
#8276 = CARTESIAN_POINT ( 'NONE',  ( -12.00000337463128908, 69.28203230275516944, -9.999999999999998224 ) ) ;
#8277 = LINE ( 'NONE', #24972, #25161 ) ;
#8278 = EDGE_CURVE ( 'NONE', #31054, #29052, #7308, .T. ) ;
#8279 = CARTESIAN_POINT ( 'NONE',  ( 6.532899837730827386, 0.000000000000000000, -5.700000000000001066 ) ) ;
#8280 = CARTESIAN_POINT ( 'NONE',  ( 0.000000000000000000, 0.000000000000000000, 32.50000000000000000 ) ) ;
#8281 = CARTESIAN_POINT ( 'NONE',  ( 5.253679167943698936, -3.068492024352256209, -4.366070081385298174 ) ) ;
#8282 = ADVANCED_FACE ( 'NONE', ( #23820 ), #18744, .T. ) ;
#8283 = ORIENTED_EDGE ( 'NONE', *, *, #897, .F. ) ;
#8284 = DIRECTION ( 'NONE',  ( 1.000000000000000000, 0.000000000000000000, 0.000000000000000000 ) ) ;
#8285 = AXIS2_PLACEMENT_3D ( 'NONE', #25852, #33926, #22856 ) ;
#8286 = CARTESIAN_POINT ( 'NONE',  ( 4.279621169095998212, -62.97617850287780072, 12.49999999999999822 ) ) ;
#8287 = LINE ( 'NONE', #181, #36178 ) ;
#8288 = EDGE_LOOP ( 'NONE', ( #11562, #9328, #11716, #17597 ) ) ;
#8289 = DIRECTION ( 'NONE',  ( 1.000000000000000000, 0.000000000000000000, 0.000000000000000000 ) ) ;
#8290 = DIRECTION ( 'NONE',  ( 0.000000000000000000, 0.000000000000000000, 1.000000000000000000 ) ) ;
#8291 = AXIS2_PLACEMENT_3D ( 'NONE', #4862, #21907, #10285 ) ;
#8292 = ADVANCED_FACE ( 'NONE', ( #1684 ), #4312, .F. ) ;
#8293 = ORIENTED_EDGE ( 'NONE', *, *, #33614, .F. ) ;
#8294 = ADVANCED_FACE ( 'NONE', ( #6932 ), #13121, .F. ) ;
#8295 = ORIENTED_EDGE ( 'NONE', *, *, #9266, .T. ) ;
#8296 = CARTESIAN_POINT ( 'NONE',  ( 68.19171716056558807, -52.81599796988855644, 12.50000000000000000 ) ) ;
#8297 = EDGE_CURVE ( 'NONE', #520, #25333, #18014, .T. ) ;
#8298 = AXIS2_PLACEMENT_3D ( 'NONE', #19365, #30784, #9204 ) ;
#8299 = EDGE_CURVE ( 'NONE', #25770, #2284, #27003, .T. ) ;
#8300 = DIRECTION ( 'NONE',  ( -0.8660254037844379305, 0.5000000000000011102, 0.000000000000000000 ) ) ;
#8301 = CARTESIAN_POINT ( 'NONE',  ( -69.13212189986965939, -2.778182860042805125, -49.86348611802629449 ) ) ;
#8302 = EDGE_CURVE ( 'NONE', #26696, #17068, #24374, .T. ) ;
#8303 = CARTESIAN_POINT ( 'NONE',  ( 44.99999662536849598, -77.94228634059960825, -9.999999999999998224 ) ) ;
#8304 = ORIENTED_EDGE ( 'NONE', *, *, #12992, .F. ) ;
#8305 = ORIENTED_EDGE ( 'NONE', *, *, #21098, .T. ) ;
#8306 = AXIS2_PLACEMENT_3D ( 'NONE', #9562, #32421, #1121 ) ;
#8307 = CIRCLE ( 'NONE', #23249, 1.750000000000018652 ) ;
#8308 = CARTESIAN_POINT ( 'NONE',  ( 0.000000000000000000, 0.000000000000000000, -5.674599999999998090 ) ) ;
#8309 = VECTOR ( 'NONE', #29995, 1000.000000000000000 ) ;
#8310 = EDGE_LOOP ( 'NONE', ( #4734, #2937, #10628, #15493, #14734, #7476, #21866, #22793, #13839, #3492, #33409, #26878 ) ) ;
#8311 = CARTESIAN_POINT ( 'NONE',  ( 36.99999662536855283, 60.62177826491078747, 17.49999999999999645 ) ) ;
#8312 = EDGE_LOOP ( 'NONE', ( #23689, #20270 ) ) ;
#8313 = CIRCLE ( 'NONE', #7098, 2.000000000000001776 ) ;
#8314 = ORIENTED_EDGE ( 'NONE', *, *, #14441, .F. ) ;
#8315 = AXIS2_PLACEMENT_3D ( 'NONE', #4385, #25019, #12796 ) ;
#8316 = DIRECTION ( 'NONE',  ( 1.000000000000000000, 0.000000000000000000, 0.000000000000000000 ) ) ;
#8317 = CARTESIAN_POINT ( 'NONE',  ( -73.00000337463100664, -43.30127018922202353, -9.999999999999998224 ) ) ;
#8318 = ORIENTED_EDGE ( 'NONE', *, *, #24301, .T. ) ;
#8319 = VERTEX_POINT ( 'NONE', #32242 ) ;
#8320 = DIRECTION ( 'NONE',  ( 0.000000000000000000, 0.000000000000000000, -1.000000000000000000 ) ) ;
#8321 = DIRECTION ( 'NONE',  ( 0.000000000000000000, 0.000000000000000000, 1.000000000000000000 ) ) ;
#8322 = FACE_OUTER_BOUND ( 'NONE', #24689, .T. ) ;
#8323 = DIRECTION ( 'NONE',  ( 0.000000000000000000, 0.000000000000000000, 1.000000000000000000 ) ) ;
#8324 = ORIENTED_EDGE ( 'NONE', *, *, #6821, .F. ) ;
#8325 = DIRECTION ( 'NONE',  ( 1.000000000000000000, 0.000000000000000000, 0.000000000000000000 ) ) ;
#8326 = FACE_BOUND ( 'NONE', #17428, .T. ) ;
#8327 = AXIS2_PLACEMENT_3D ( 'NONE', #3649, #17350, #256 ) ;
#8328 = CARTESIAN_POINT ( 'NONE',  ( -37.50000000000000000, 103.4105893997321886, -19.99999999999999645 ) ) ;
#8329 = CYLINDRICAL_SURFACE ( 'NONE', #28843, 2.500000000000000444 ) ;
#8330 = CARTESIAN_POINT ( 'NONE',  ( -4.279621169095561228, 62.97617850287782915, -4.999999999999997335 ) ) ;
#8331 = DIRECTION ( 'NONE',  ( 0.000000000000000000, 0.000000000000000000, -1.000000000000000000 ) ) ;
#8332 = CARTESIAN_POINT ( 'NONE',  ( -52.39915983220772233, -35.19434990244957362, -4.999999999999997335 ) ) ;
#8333 = CIRCLE ( 'NONE', #11319, 27.00000000000001066 ) ;
#8334 = DIRECTION ( 'NONE',  ( 1.000000000000000000, 0.000000000000000000, 0.000000000000000000 ) ) ;
#8335 = ORIENTED_EDGE ( 'NONE', *, *, #34866, .T. ) ;
#8336 = DIRECTION ( 'NONE',  ( 0.000000000000000000, 0.000000000000000000, 1.000000000000000000 ) ) ;
#8337 = CARTESIAN_POINT ( 'NONE',  ( -5.000000000000000888, -0.4954705650270051498, -2.700341035846709481E-15 ) ) ;
#8338 = DIRECTION ( 'NONE',  ( 0.000000000000000000, 0.000000000000000000, 1.000000000000000000 ) ) ;
#8339 = CIRCLE ( 'NONE', #22701, 2.000000000000001776 ) ;
#8340 = VERTEX_POINT ( 'NONE', #6570 ) ;
#8341 = ADVANCED_FACE ( 'NONE', ( #20998 ), #29802, .F. ) ;
#8342 = ORIENTED_EDGE ( 'NONE', *, *, #7192, .F. ) ;
#8343 = VERTEX_POINT ( 'NONE', #927 ) ;
#8344 = ADVANCED_FACE ( 'NONE', ( #12351 ), #32428, .T. ) ;
#8345 = EDGE_CURVE ( 'NONE', #11561, #5584, #18615, .T. ) ;
#8346 = CYLINDRICAL_SURFACE ( 'NONE', #15954, 2.000000000000001776 ) ;
#8347 = CARTESIAN_POINT ( 'NONE',  ( -111.8061974404896262, 19.22934205795090534, 27.50000000000000000 ) ) ;
#8348 = ORIENTED_EDGE ( 'NONE', *, *, #16090, .F. ) ;
#8349 = CARTESIAN_POINT ( 'NONE',  ( 66.99999662536839651, -43.30127018922199511, 17.49999999999999645 ) ) ;
#8350 = AXIS2_PLACEMENT_3D ( 'NONE', #12532, #1462, #35988 ) ;
#8351 = VERTEX_POINT ( 'NONE', #1128 ) ;
#8352 = CARTESIAN_POINT ( 'NONE',  ( 20.26402367686958428, -109.7457339126789151, 32.50000000000000711 ) ) ;
#8353 = VERTEX_POINT ( 'NONE', #1304 ) ;
#8354 = AXIS2_PLACEMENT_3D ( 'NONE', #6723, #15548, #20980 ) ;
#8355 = CARTESIAN_POINT ( 'NONE',  ( 0.000000000000000000, 0.000000000000000000, -10.00000000000000000 ) ) ;
#8356 = ORIENTED_EDGE ( 'NONE', *, *, #22485, .F. ) ;
#8357 = CYLINDRICAL_SURFACE ( 'NONE', #19014, 2.000000000000000000 ) ;
#8358 = DIRECTION ( 'NONE',  ( 0.000000000000000000, 0.000000000000000000, -1.000000000000000000 ) ) ;
#8359 = AXIS2_PLACEMENT_3D ( 'NONE', #16592, #16789, #13785 ) ;
#8360 = EDGE_LOOP ( 'NONE', ( #20679, #10568, #20480, #25399, #35579, #18853, #8988, #28562 ) ) ;
#8361 = DIRECTION ( 'NONE',  ( 0.000000000000000000, 0.000000000000000000, -1.000000000000000000 ) ) ;
#8362 = AXIS2_PLACEMENT_3D ( 'NONE', #10649, #33539, #1449 ) ;
#8363 = EDGE_CURVE ( 'NONE', #2722, #3797, #3110, .T. ) ;
#8364 = DIRECTION ( 'NONE',  ( 0.000000000000000000, 0.000000000000000000, -1.000000000000000000 ) ) ;
#8365 = CARTESIAN_POINT ( 'NONE',  ( 15.97563234535730814, -90.60231327712320137, -4.999999999999997335 ) ) ;
#8366 = AXIS2_PLACEMENT_3D ( 'NONE', #18502, #10408, #4250 ) ;
#8367 = ORIENTED_EDGE ( 'NONE', *, *, #2544, .F. ) ;
#8368 = CARTESIAN_POINT ( 'NONE',  ( 82.99999662536831124, -25.98076211353319565, 12.50000000000000000 ) ) ;
#8369 = CARTESIAN_POINT ( 'NONE',  ( -5.000003374631307729, 77.94228634059957983, -5.000000000000000000 ) ) ;
#8370 = VERTEX_POINT ( 'NONE', #2595 ) ;
#8371 = CIRCLE ( 'NONE', #13149, 2.541999999999999815 ) ;
#8372 = DIRECTION ( 'NONE',  ( 1.000000000000000000, 0.000000000000000000, 0.000000000000000000 ) ) ;
#8373 = CARTESIAN_POINT ( 'NONE',  ( 76.99999662536836809, 8.660254037844394404, 12.50000000000000000 ) ) ;
#8374 = FACE_OUTER_BOUND ( 'NONE', #8643, .T. ) ;
#8375 = FACE_OUTER_BOUND ( 'NONE', #6401, .T. ) ;
#8376 = ORIENTED_EDGE ( 'NONE', *, *, #21797, .F. ) ;
#8377 = EDGE_LOOP ( 'NONE', ( #33138, #23680 ) ) ;
#8378 = CIRCLE ( 'NONE', #19169, 3.499999999999989342 ) ;
#8379 = CYLINDRICAL_SURFACE ( 'NONE', #20151, 3.500000000000003109 ) ;
#8380 = CARTESIAN_POINT ( 'NONE',  ( 56.67878100130369035, -27.78182860042797131, -4.999999999999997335 ) ) ;
#8381 = VERTEX_POINT ( 'NONE', #25127 ) ;
#8382 = VERTEX_POINT ( 'NONE', #16854 ) ;
#8383 = EDGE_CURVE ( 'NONE', #12339, #36437, #22222, .T. ) ;
#8384 = DIRECTION ( 'NONE',  ( 0.000000000000000000, 0.000000000000000000, 1.000000000000000000 ) ) ;
#8385 = CARTESIAN_POINT ( 'NONE',  ( -55.00000337463109901, -60.62177826491083010, -5.000000000000000000 ) ) ;
#8386 = CARTESIAN_POINT ( 'NONE',  ( 11.99999662536865763, -86.60254037844400443, -9.999999999999998224 ) ) ;
#8387 = CIRCLE ( 'NONE', #35936, 2.000000000000001776 ) ;
#8388 = ORIENTED_EDGE ( 'NONE', *, *, #22864, .T. ) ;
#8389 = ORIENTED_EDGE ( 'NONE', *, *, #15831, .T. ) ;
#8390 = CARTESIAN_POINT ( 'NONE',  ( -2.374207310413330682E-13, -68.00000000000000000, 12.49999999999999822 ) ) ;
#8391 = CIRCLE ( 'NONE', #23257, 2.000000000000001776 ) ;
#8392 = FACE_OUTER_BOUND ( 'NONE', #28447, .T. ) ;
#8393 = ORIENTED_EDGE ( 'NONE', *, *, #8262, .F. ) ;
#8394 = CARTESIAN_POINT ( 'NONE',  ( 44.99999662536851019, 77.94228634059959404, -9.999999999999998224 ) ) ;
#8395 = ORIENTED_EDGE ( 'NONE', *, *, #22037, .F. ) ;
#8397 = CIRCLE ( 'NONE', #13178, 2.000000000000001776 ) ;
#8396 = FACE_BOUND ( 'NONE', #19664, .T. ) ;
#8398 = CARTESIAN_POINT ( 'NONE',  ( -47.00000337463111322, 60.62177826491077326, -9.999999999999998224 ) ) ;
#8399 = EDGE_CURVE ( 'NONE', #33068, #12455, #644, .T. ) ;
#8400 = AXIS2_PLACEMENT_3D ( 'NONE', #30106, #24868, #24304 ) ;
#8401 = ORIENTED_EDGE ( 'NONE', *, *, #27109, .T. ) ;
#8402 = ADVANCED_FACE ( 'NONE', ( #21922 ), #7856, .T. ) ;
#8403 = DIRECTION ( 'NONE',  ( 0.000000000000000000, 0.000000000000000000, 1.000000000000000000 ) ) ;
#8404 = CARTESIAN_POINT ( 'NONE',  ( -85.00000337463092137, -8.660254037844422825, 12.50000000000000000 ) ) ;
#8405 = CARTESIAN_POINT ( 'NONE',  ( 44.99999662536851019, -60.62177826491080168, -9.999999999999998224 ) ) ;
#8406 = DIRECTION ( 'NONE',  ( 0.000000000000000000, 0.000000000000000000, 1.000000000000000000 ) ) ;
#8407 = VERTEX_POINT ( 'NONE', #36176 ) ;
#8408 = CIRCLE ( 'NONE', #12586, 2.000000000000000000 ) ;
#8409 = DIRECTION ( 'NONE',  ( -1.000000000000000000, -0.000000000000000000, -0.000000000000000000 ) ) ;
#8410 = ADVANCED_FACE ( 'NONE', ( #18927 ), #13291, .F. ) ;
#8411 = DIRECTION ( 'NONE',  ( 1.000000000000000000, 0.000000000000000000, 0.000000000000000000 ) ) ;
#8412 = DIRECTION ( 'NONE',  ( 1.000000000000000000, 0.000000000000000000, 0.000000000000000000 ) ) ;
#8413 = VERTEX_POINT ( 'NONE', #30356 ) ;
#8414 = EDGE_CURVE ( 'NONE', #4196, #8015, #27599, .T. ) ;
#8415 = ORIENTED_EDGE ( 'NONE', *, *, #1152, .T. ) ;
#8416 = VECTOR ( 'NONE', #20262, 1000.000000000000000 ) ;
#8417 = ORIENTED_EDGE ( 'NONE', *, *, #8868, .T. ) ;
#8418 = DIRECTION ( 'NONE',  ( 1.000000000000000000, 0.000000000000000000, 0.000000000000000000 ) ) ;
#8419 = DIRECTION ( 'NONE',  ( 1.000000000000000000, 0.000000000000000000, 0.000000000000000000 ) ) ;
#8420 = CARTESIAN_POINT ( 'NONE',  ( -13.89091430021420237, -62.33939050065180254, 12.49999999999999822 ) ) ;
#8421 = LINE ( 'NONE', #14219, #26550 ) ;
#8422 = EDGE_CURVE ( 'NONE', #14720, #942, #33605, .T. ) ;
#8423 = CARTESIAN_POINT ( 'NONE',  ( -85.00000337463092137, -25.98076211353322051, -5.000000000000000000 ) ) ;
#8424 = CARTESIAN_POINT ( 'NONE',  ( -77.93337901593650940, -72.12093275448718543, 32.50001250000000397 ) ) ;
#8425 = CARTESIAN_POINT ( 'NONE',  ( 64.99999662536841072, 25.98076211353318854, 17.49999999999999645 ) ) ;
#8426 = CARTESIAN_POINT ( 'NONE',  ( -6.000000000000000000, 145.0000000000000568, 27.50000000000000000 ) ) ;
#8427 = ORIENTED_EDGE ( 'NONE', *, *, #21645, .T. ) ;
#8428 = ORIENTED_EDGE ( 'NONE', *, *, #3506, .T. ) ;
#8429 = DIRECTION ( 'NONE',  ( -1.000000000000000000, -0.000000000000000000, -0.000000000000000000 ) ) ;
#8430 = CARTESIAN_POINT ( 'NONE',  ( 74.99999662536836809, -8.660254037844401509, -9.999999999999998224 ) ) ;
#8431 = CARTESIAN_POINT ( 'NONE',  ( 6.249999999999998224, 3.673940397442060854E-16, -3.000000000000000888 ) ) ;
#8432 = CARTESIAN_POINT ( 'NONE',  ( -82.00000337463094979, 17.32050807568878525, 17.49999999999999645 ) ) ;
#8433 = VERTEX_POINT ( 'NONE', #19670 ) ;
#8434 = UNCERTAINTY_MEASURE_WITH_UNIT (LENGTH_MEASURE( 1.000000000000000082E-05 ), #30742, 'distance_accuracy_value', 'NONE');
#8435 = ADVANCED_FACE ( 'NONE', ( #33565 ), #31101, .F. ) ;
#8436 = FACE_BOUND ( 'NONE', #26342, .T. ) ;
#8437 = ORIENTED_EDGE ( 'NONE', *, *, #34019, .T. ) ;
#8438 = VERTEX_POINT ( 'NONE', #14020 ) ;
#8439 = EDGE_CURVE ( 'NONE', #31907, #28198, #12620, .T. ) ;
#8440 = DIRECTION ( 'NONE',  ( -1.000000000000000000, 0.000000000000000000, 0.000000000000000000 ) ) ;
#8441 = ORIENTED_EDGE ( 'NONE', *, *, #27036, .F. ) ;
#8442 = CYLINDRICAL_SURFACE ( 'NONE', #2964, 2.000000000000001776 ) ;
#8443 = DIRECTION ( 'NONE',  ( 1.000000000000000000, 0.000000000000000000, 0.000000000000000000 ) ) ;
#8444 = DIRECTION ( 'NONE',  ( -0.000000000000000000, -0.8660254037844413721, 0.4999999999999952816 ) ) ;
#8445 = VERTEX_POINT ( 'NONE', #21732 ) ;
#8446 = ORIENTED_EDGE ( 'NONE', *, *, #18065, .T. ) ;
#8447 = EDGE_CURVE ( 'NONE', #3051, #3447, #10846, .T. ) ;
#8448 = EDGE_LOOP ( 'NONE', ( #16159, #37080, #15150, #23412 ) ) ;
#8449 = VERTEX_POINT ( 'NONE', #24742 ) ;
#8450 = ADVANCED_FACE ( 'NONE', ( #7682 ), #19133, .F. ) ;
#8451 = EDGE_LOOP ( 'NONE', ( #1326, #18200, #15528, #11717 ) ) ;
#8452 = CARTESIAN_POINT ( 'NONE',  ( -47.00000337463111322, 60.62177826491077326, -9.999999999999998224 ) ) ;
#8453 = CARTESIAN_POINT ( 'NONE',  ( -75.00000337463097821, 25.98076211353318854, -9.999999999999998224 ) ) ;
#8454 = DIRECTION ( 'NONE',  ( 0.000000000000000000, 0.000000000000000000, -1.000000000000000000 ) ) ;
#8455 = DIRECTION ( 'NONE',  ( -1.000000000000000000, 0.000000000000000000, 0.000000000000000000 ) ) ;
#8456 = LINE ( 'NONE', #13886, #25529 ) ;
#8457 = ORIENTED_EDGE ( 'NONE', *, *, #9866, .F. ) ;
#8458 = LINE ( 'NONE', #2467, #10537 ) ;
#8459 = DIRECTION ( 'NONE',  ( 0.000000000000000000, 0.000000000000000000, 1.000000000000000000 ) ) ;
#8460 = LINE ( 'NONE', #5835, #16445 ) ;
#8461 = EDGE_LOOP ( 'NONE', ( #16036, #26770, #33752, #35525 ) ) ;
#8462 = CARTESIAN_POINT ( 'NONE',  ( -106.7731239591675205, 98.28784258493142545, 27.50000000000000000 ) ) ;
#8463 = DIRECTION ( 'NONE',  ( -0.000000000000000000, 0.000000000000000000, -1.000000000000000000 ) ) ;
#8464 = VERTEX_POINT ( 'NONE', #27720 ) ;
#8465 = EDGE_LOOP ( 'NONE', ( #32277, #11285 ) ) ;
#8466 = ADVANCED_FACE ( 'NONE', ( #25294 ), #2036, .F. ) ;
#8467 = DIRECTION ( 'NONE',  ( 0.000000000000000000, 0.000000000000000000, 1.000000000000000000 ) ) ;
#8468 = CARTESIAN_POINT ( 'NONE',  ( -5.284804376168104945, 3.015249596956793177, -4.366192694417977194 ) ) ;
#8469 = PLANE ( 'NONE',  #19276 ) ;
#8470 = CARTESIAN_POINT ( 'NONE',  ( -70.80619744048887299, 84.18124734178336155, 27.50000000000000000 ) ) ;
#8471 = ORIENTED_EDGE ( 'NONE', *, *, #24185, .T. ) ;
#8472 = ORIENTED_EDGE ( 'NONE', *, *, #19145, .F. ) ;
#8473 = CARTESIAN_POINT ( 'NONE',  ( 0.000000000000000000, 0.000000000000000000, -6.000000000000000000 ) ) ;
#8474 = ADVANCED_FACE ( 'NONE', ( #10678 ), #22120, .F. ) ;
#8475 = CARTESIAN_POINT ( 'NONE',  ( -145.0000000000000000, 6.000000000001517009, 32.55002500000000509 ) ) ;
#8476 = EDGE_LOOP ( 'NONE', ( #18313, #5350, #24397, #33592 ) ) ;
#8477 = VECTOR ( 'NONE', #16564, 1000.000000000000000 ) ;
#8478 = EDGE_CURVE ( 'NONE', #28544, #3789, #19817, .T. ) ;
#8479 = ADVANCED_FACE ( 'NONE', ( #11406 ), #25673, .F. ) ;
#8480 = VECTOR ( 'NONE', #25307, 1000.000000000000000 ) ;
#8481 = DIRECTION ( 'NONE',  ( 0.000000000000000000, 0.000000000000000000, 1.000000000000000000 ) ) ;
#8482 = VERTEX_POINT ( 'NONE', #11219 ) ;
#8483 = VERTEX_POINT ( 'NONE', #3532 ) ;
#8484 = DIRECTION ( 'NONE',  ( -0.5000000000000014433, -0.8660254037844378194, 0.000000000000000000 ) ) ;
#8485 = CARTESIAN_POINT ( 'NONE',  ( -45.00000337463111322, 60.62177826491077326, -9.999999999999998224 ) ) ;
#8486 = DIRECTION ( 'NONE',  ( 1.000000000000000000, 0.000000000000000000, 0.000000000000000000 ) ) ;
#8487 = ORIENTED_EDGE ( 'NONE', *, *, #3511, .T. ) ;
#8488 = EDGE_LOOP ( 'NONE', ( #10278, #5573, #15998, #17044 ) ) ;
#8489 = LINE ( 'NONE', #22753, #25116 ) ;
#8490 = LINE ( 'NONE', #6402, #2912 ) ;
#8491 = CARTESIAN_POINT ( 'NONE',  ( 84.88770958243756581, -10.65709945499362554, 12.50000000000000000 ) ) ;
#8492 = DIRECTION ( 'NONE',  ( 0.000000000000000000, 0.000000000000000000, 1.000000000000000000 ) ) ;
#8493 = EDGE_CURVE ( 'NONE', #22989, #3582, #16824, .T. ) ;
#8494 = ORIENTED_EDGE ( 'NONE', *, *, #18044, .T. ) ;
#8495 = FACE_OUTER_BOUND ( 'NONE', #19416, .T. ) ;
#8496 = FACE_BOUND ( 'NONE', #29784, .T. ) ;
#8497 = CARTESIAN_POINT ( 'NONE',  ( 64.99999662536841072, -25.98076211353320275, 12.50000000000000000 ) ) ;
#8498 = DIRECTION ( 'NONE',  ( 0.000000000000000000, 0.000000000000000000, 1.000000000000000000 ) ) ;
#8499 = DIRECTION ( 'NONE',  ( 0.000000000000000000, -0.4999999999999990563, 0.8660254037844391517 ) ) ;
#8500 = CARTESIAN_POINT ( 'NONE',  ( 34.99999662536855283, -60.62177826491080168, 17.49999999999999645 ) ) ;
#8501 = CARTESIAN_POINT ( 'NONE',  ( -22.62085422049824501, 105.9441492178757898, 27.49998800000000543 ) ) ;
#8502 = AXIS2_PLACEMENT_3D ( 'NONE', #8119, #19563, #36799 ) ;
#8503 = DIRECTION ( 'NONE',  ( 0.000000000000000000, 0.000000000000000000, 1.000000000000000000 ) ) ;
#8504 = ORIENTED_EDGE ( 'NONE', *, *, #18049, .T. ) ;
#8505 = CARTESIAN_POINT ( 'NONE',  ( 56.99999662536844625, 43.30127018922198801, -5.000000000000000000 ) ) ;
#8506 = DIRECTION ( 'NONE',  ( 0.000000000000000000, 0.000000000000000000, 1.000000000000000000 ) ) ;
#8507 = LINE ( 'NONE', #25386, #29493 ) ;
#8508 = ORIENTED_EDGE ( 'NONE', *, *, #31425, .T. ) ;
#8509 = EDGE_LOOP ( 'NONE', ( #36451, #28937, #2269, #17596, #31311, #24321, #33282, #29857, #26100, #24984, #13129, #28209 ) ) ;
#8510 = EDGE_CURVE ( 'NONE', #36669, #3287, #8776, .T. ) ;
#8511 = VERTEX_POINT ( 'NONE', #2790 ) ;
#8512 = CARTESIAN_POINT ( 'NONE',  ( -51.68138994340220904, -113.8157894736842053, 32.50000000000000000 ) ) ;
#8513 = CARTESIAN_POINT ( 'NONE',  ( -85.00000337463092137, -25.98076211353322051, 12.50000000000000000 ) ) ;
#8514 = ADVANCED_FACE ( 'NONE', ( #5591 ), #31781, .T. ) ;
#8515 = LINE ( 'NONE', #19946, #12410 ) ;
#8516 = VERTEX_POINT ( 'NONE', #5787 ) ;
#8517 = EDGE_CURVE ( 'NONE', #1626, #2314, #13819, .T. ) ;
#8518 = CARTESIAN_POINT ( 'NONE',  ( -61.25926521283079751, 32.16008401677975570, 12.49999999999999645 ) ) ;
#8519 = VERTEX_POINT ( 'NONE', #31983 ) ;
#8520 = DIRECTION ( 'NONE',  ( 1.000000000000000000, 0.000000000000000000, 0.000000000000000000 ) ) ;
#8522 = ADVANCED_FACE ( 'NONE', ( #14216 ), #17762, .F. ) ;
#8521 = ORIENTED_EDGE ( 'NONE', *, *, #4463, .F. ) ;
#8523 = CYLINDRICAL_SURFACE ( 'NONE', #15369, 2.000000000000001776 ) ;
#8524 = ORIENTED_EDGE ( 'NONE', *, *, #32549, .T. ) ;
#8525 = ADVANCED_FACE ( 'NONE', ( #37106 ), #14575, .F. ) ;
#8526 = ORIENTED_EDGE ( 'NONE', *, *, #4360, .T. ) ;
#8527 = CARTESIAN_POINT ( 'NONE',  ( 79.99999662536832545, -17.32050807568879591, -9.999999999999998224 ) ) ;
#8528 = DIRECTION ( 'NONE',  ( 0.000000000000000000, 0.000000000000000000, -1.000000000000000000 ) ) ;
#8529 = CIRCLE ( 'NONE', #28270, 20.00000000000001066 ) ;
#8530 = ORIENTED_EDGE ( 'NONE', *, *, #11671, .T. ) ;
#8531 = CARTESIAN_POINT ( 'NONE',  ( 74.99999662536836809, -8.660254037844401509, -5.000000000000000000 ) ) ;
#8532 = ITEM_DEFINED_TRANSFORMATION ( 'NONE', 'NONE', #14177,  #21385 ) ;
#8533 = EDGE_CURVE ( 'NONE', #33319, #23244, #31187, .T. ) ;
#8534 = DIRECTION ( 'NONE',  ( 1.000000000000000000, 0.000000000000000000, 0.000000000000000000 ) ) ;
#8535 = EDGE_CURVE ( 'NONE', #13708, #36567, #6639, .T. ) ;
#8536 = CARTESIAN_POINT ( 'NONE',  ( -72.00000337463100664, 17.32050807568877460, 12.50000000000000000 ) ) ;
#8537 = EDGE_CURVE ( 'NONE', #25534, #35280, #16235, .T. ) ;
#8538 = ORIENTED_EDGE ( 'NONE', *, *, #18238, .T. ) ;
#8539 = DIRECTION ( 'NONE',  ( 0.000000000000000000, 0.000000000000000000, 1.000000000000000000 ) ) ;
#8540 = DIRECTION ( 'NONE',  ( 0.000000000000000000, 0.000000000000000000, 1.000000000000000000 ) ) ;
#8541 = EDGE_CURVE ( 'NONE', #20425, #816, #26212, .T. ) ;
#8542 = ORIENTED_EDGE ( 'NONE', *, *, #21202, .T. ) ;
#8543 = CARTESIAN_POINT ( 'NONE',  ( 0.000000000000000000, 84.16276890242652087, -34.97964607176039920 ) ) ;
#8544 = DIRECTION ( 'NONE',  ( 1.000000000000000000, 0.000000000000000000, 0.000000000000000000 ) ) ;
#8545 = CYLINDRICAL_SURFACE ( 'NONE', #10011, 2.000000000000001776 ) ;
#8546 = CARTESIAN_POINT ( 'NONE',  ( -67.00000337463104927, -25.98076211353322051, -9.999999999999998224 ) ) ;
#8547 = AXIS2_PLACEMENT_3D ( 'NONE', #28, #28162, #22174 ) ;
#8548 = ORIENTED_EDGE ( 'NONE', *, *, #5759, .T. ) ;
#8549 = ORIENTED_EDGE ( 'NONE', *, *, #25717, .F. ) ;
#8550 = DIRECTION ( 'NONE',  ( 0.000000000000000000, 0.000000000000000000, 1.000000000000000000 ) ) ;
#8551 = CARTESIAN_POINT ( 'NONE',  ( 64.99999662536839651, 60.62177826491078747, -9.999999999999998224 ) ) ;
#8552 = ORIENTED_EDGE ( 'NONE', *, *, #7592, .F. ) ;
#8553 = EDGE_LOOP ( 'NONE', ( #14654, #28193 ) ) ;
#8554 = CARTESIAN_POINT ( 'NONE',  ( 4.999999999999997335, -0.9835753746177055001, -0.05800540215398956867 ) ) ;
#8555 = CARTESIAN_POINT ( 'NONE',  ( -20.00000337463122690, 86.60254037844397601, 12.50000000000000000 ) ) ;
#8556 = AXIS2_PLACEMENT_3D ( 'NONE', #5142, #30462, #33825 ) ;
#8557 = LINE ( 'NONE', #19991, #29621 ) ;
#8558 = EDGE_CURVE ( 'NONE', #25301, #12879, #668, .T. ) ;
#8559 = ORIENTED_EDGE ( 'NONE', *, *, #35027, .F. ) ;
#8560 = ORIENTED_EDGE ( 'NONE', *, *, #18598, .F. ) ;
#8561 = FACE_OUTER_BOUND ( 'NONE', #34382, .T. ) ;
#8562 = DIRECTION ( 'NONE',  ( -1.000000000000000000, 0.000000000000000000, 0.000000000000000000 ) ) ;
#8563 = ORIENTED_EDGE ( 'NONE', *, *, #13251, .T. ) ;
#8564 = DIRECTION ( 'NONE',  ( -0.5000000000000101030, -0.8660254037844328234, 0.000000000000000000 ) ) ;
#8565 = ORIENTED_EDGE ( 'NONE', *, *, #32059, .T. ) ;
#8566 = FACE_BOUND ( 'NONE', #20135, .T. ) ;
#8567 = CIRCLE ( 'NONE', #18141, 2.000000000000001776 ) ;
#8568 = FACE_OUTER_BOUND ( 'NONE', #7237, .T. ) ;
#8569 = DIRECTION ( 'NONE',  ( -0.000000000000000000, -0.000000000000000000, 1.000000000000000000 ) ) ;
#8570 = ORIENTED_EDGE ( 'NONE', *, *, #36220, .T. ) ;
#8571 = CARTESIAN_POINT ( 'NONE',  ( 47.63139720814418610, 27.49999999999988987, -16.00000000000000000 ) ) ;
#8572 = CARTESIAN_POINT ( 'NONE',  ( 3.750000000000001776, 0.000000000000000000, 2.266666666666999674 ) ) ;
#8573 = VECTOR ( 'NONE', #5425, 1000.000000000000000 ) ;
#8574 = DIRECTION ( 'NONE',  ( 0.000000000000000000, 0.000000000000000000, 1.000000000000000000 ) ) ;
#8575 = DIRECTION ( 'NONE',  ( 0.000000000000000000, 0.000000000000000000, -1.000000000000000000 ) ) ;
#8576 = ADVANCED_FACE ( 'NONE', ( #23215, #20217, #14767, #6142, #34116, #5976, #523 ), #17407, .F. ) ;
#8577 = ORIENTED_EDGE ( 'NONE', *, *, #29139, .F. ) ;
#8578 = CARTESIAN_POINT ( 'NONE',  ( -58.88972745734155723, 34.00000000000049027, 12.49999999999999822 ) ) ;
#8579 = CARTESIAN_POINT ( 'NONE',  ( -43.19957991610399972, -47.04203867989563292, 12.49999999999999822 ) ) ;
#8580 = CARTESIAN_POINT ( 'NONE',  ( 0.000000000000000000, 0.000000000000000000, 4.700000000000000178 ) ) ;
#8581 = ORIENTED_EDGE ( 'NONE', *, *, #23047, .F. ) ;
#8582 = ORIENTED_EDGE ( 'NONE', *, *, #36845, .T. ) ;
#8583 = VERTEX_POINT ( 'NONE', #11950 ) ;
#8584 = AXIS2_PLACEMENT_3D ( 'NONE', #26124, #11330, #22782 ) ;
#8585 = AXIS2_PLACEMENT_3D ( 'NONE', #31820, #20572, #20232 ) ;
#8586 = CARTESIAN_POINT ( 'NONE',  ( 0.000000000000000000, 89.94802294027088863, -23.00000000000000000 ) ) ;
#8587 = DIRECTION ( 'NONE',  ( -0.8660254037844453689, -0.4999999999999882871, 0.000000000000000000 ) ) ;
#8588 = CARTESIAN_POINT ( 'NONE',  ( 106.1304126751635835, -55.40976756914862023, 32.50000000000002132 ) ) ;
#8589 = DIRECTION ( 'NONE',  ( -0.000000000000000000, 1.000000000000000000, 0.000000000000000000 ) ) ;
#8590 = DIRECTION ( 'NONE',  ( 1.000000000000000000, 0.000000000000000000, 0.000000000000000000 ) ) ;
#8591 = ADVANCED_FACE ( 'NONE', ( #34836 ), #9132, .T. ) ;
#8592 = CARTESIAN_POINT ( 'NONE',  ( 69.61830985333858735, 36.60425714729669977, -5.000000000000000000 ) ) ;
#8593 = ADVANCED_FACE ( 'NONE', ( #15521 ), #32757, .F. ) ;
#8594 = VERTEX_POINT ( 'NONE', #15698 ) ;
#8595 = ORIENTED_EDGE ( 'NONE', *, *, #29123, .T. ) ;
#8596 = DIRECTION ( 'NONE',  ( 0.7071067811865486830, 0.000000000000000000, 0.7071067811865464625 ) ) ;
#8597 = VECTOR ( 'NONE', #25216, 1000.000000000000000 ) ;
#8598 = FACE_OUTER_BOUND ( 'NONE', #18952, .T. ) ;
#8599 = DIRECTION ( 'NONE',  ( 0.000000000000000000, 0.000000000000000000, -1.000000000000000000 ) ) ;
#8600 = CARTESIAN_POINT ( 'NONE',  ( 51.13139720814399425, -27.50000000000022737, -10.00000000000000000 ) ) ;
#8601 = ORIENTED_EDGE ( 'NONE', *, *, #31624, .T. ) ;
#8602 = AXIS2_PLACEMENT_3D ( 'NONE', #8380, #28408, #34424 ) ;
#8603 = EDGE_CURVE ( 'NONE', #5113, #9816, #12020, .T. ) ;
#8604 = FACE_BOUND ( 'NONE', #15764, .T. ) ;
#8605 = ORIENTED_EDGE ( 'NONE', *, *, #28294, .T. ) ;
#8606 = VERTEX_POINT ( 'NONE', #10079 ) ;
#8607 = CARTESIAN_POINT ( 'NONE',  ( 102.5304832720488832, -102.5304832720499633, 27.50000000000000000 ) ) ;
#8608 = ORIENTED_EDGE ( 'NONE', *, *, #11336, .F. ) ;
#8609 = CARTESIAN_POINT ( 'NONE',  ( 17.55872235085560007, 89.94802294027088863, 32.49999999999999289 ) ) ;
#8610 = AXIS2_PLACEMENT_3D ( 'NONE', #29753, #18528, #26766 ) ;
#8611 = CARTESIAN_POINT ( 'NONE',  ( 19.99999662536858835, 69.28203230275516944, -9.999999999999998224 ) ) ;
#8612 = CARTESIAN_POINT ( 'NONE',  ( -72.28378166042018904, -61.53067111003240797, -4.999999999999997335 ) ) ;
#8613 = EDGE_CURVE ( 'NONE', #37066, #31750, #34807, .T. ) ;
#8614 = VERTEX_POINT ( 'NONE', #35768 ) ;
#8615 = ORIENTED_EDGE ( 'NONE', *, *, #22699, .F. ) ;
#8616 = ORIENTED_EDGE ( 'NONE', *, *, #9854, .F. ) ;
#8617 = AXIS2_PLACEMENT_3D ( 'NONE', #31711, #396, #26639 ) ;
#8618 = ORIENTED_EDGE ( 'NONE', *, *, #29451, .F. ) ;
#8619 = ORIENTED_EDGE ( 'NONE', *, *, #25633, .F. ) ;
#8620 = DIRECTION ( 'NONE',  ( 0.000000000000000000, 0.000000000000000000, 1.000000000000000000 ) ) ;
#8621 = PRESENTATION_LAYER_ASSIGNMENT (  '', '', ( #20571 ) ) ;
#8622 = CARTESIAN_POINT ( 'NONE',  ( -33.99999999999945288, 58.88972745734214698, -49.86561046011506448 ) ) ;
#8623 = LINE ( 'NONE', #23441, #6499 ) ;
#8624 = DIRECTION ( 'NONE',  ( -1.000000000000000000, 0.000000000000000000, 0.000000000000000000 ) ) ;
#8625 = CARTESIAN_POINT ( 'NONE',  ( 4.999999999999999112, -3.130590339601100780, -4.027780737902369346 ) ) ;
#8626 = VERTEX_POINT ( 'NONE', #15318 ) ;
#8627 = CYLINDRICAL_SURFACE ( 'NONE', #4550, 2.000000000000001776 ) ;
#8628 = DIRECTION ( 'NONE',  ( 1.000000000000000000, 0.000000000000000000, 0.000000000000000000 ) ) ;
#8629 = EDGE_CURVE ( 'NONE', #9668, #26406, #7260, .T. ) ;
#8630 = LINE ( 'NONE', #28317, #33793 ) ;
#8631 = ORIENTED_EDGE ( 'NONE', *, *, #20204, .F. ) ;
#8632 = LINE ( 'NONE', #2843, #19672 ) ;
#8633 = LINE ( 'NONE', #17616, #23182 ) ;
#8634 = VERTEX_POINT ( 'NONE', #24320 ) ;
#8635 = CIRCLE ( 'NONE', #846, 3.000000000000003997 ) ;
#8636 = ORIENTED_EDGE ( 'NONE', *, *, #683, .F. ) ;
#8637 = CARTESIAN_POINT ( 'NONE',  ( -55.00000337463110611, -43.30127018922202353, -9.999999999999998224 ) ) ;
#8638 = DIRECTION ( 'NONE',  ( 0.000000000000000000, 0.000000000000000000, 1.000000000000000000 ) ) ;
#8639 = FACE_OUTER_BOUND ( 'NONE', #36520, .T. ) ;
#8640 = CARTESIAN_POINT ( 'NONE',  ( -5.029394918168152984, -2.903722509865350965, -4.151004066889661281 ) ) ;
#8641 = EDGE_CURVE ( 'NONE', #23192, #20237, #21279, .T. ) ;
#8642 = ORIENTED_EDGE ( 'NONE', *, *, #8739, .T. ) ;
#8643 = EDGE_LOOP ( 'NONE', ( #12348, #18447, #22807, #26446 ) ) ;
#8644 = AXIS2_PLACEMENT_3D ( 'NONE', #34861, #8990, #3905 ) ;
#8645 = CARTESIAN_POINT ( 'NONE',  ( -2.448772250512182280E-15, 99.94802294027086020, -11.00000000000000000 ) ) ;
#8646 = CYLINDRICAL_SURFACE ( 'NONE', #16513, 1.999999999999998224 ) ;
#8647 = AXIS2_PLACEMENT_3D ( 'NONE', #27336, #1100, #18151 ) ;
#8648 = DIRECTION ( 'NONE',  ( 0.000000000000000000, 0.000000000000000000, 1.000000000000000000 ) ) ;
#8649 = EDGE_CURVE ( 'NONE', #32403, #35238, #27858, .T. ) ;
#8650 = AXIS2_PLACEMENT_3D ( 'NONE', #6741, #9570, #9372 ) ;
#8651 = EDGE_LOOP ( 'NONE', ( #23370, #35292, #35083, #9376 ) ) ;
#8652 = DIRECTION ( 'NONE',  ( 1.000000000000000000, 0.000000000000000000, 0.000000000000000000 ) ) ;
#8653 = EDGE_LOOP ( 'NONE', ( #35010, #19933 ) ) ;
#8654 = ORIENTED_EDGE ( 'NONE', *, *, #13180, .T. ) ;
#8655 = DIRECTION ( 'NONE',  ( 0.000000000000000000, 0.000000000000000000, 1.000000000000000000 ) ) ;
#8656 = CIRCLE ( 'NONE', #6949, 3.000000000000002665 ) ;
#8657 = DIRECTION ( 'NONE',  ( 0.000000000000000000, 0.000000000000000000, 1.000000000000000000 ) ) ;
#8658 = EDGE_LOOP ( 'NONE', ( #27899, #10390 ) ) ;
#8659 = AXIS2_PLACEMENT_3D ( 'NONE', #29417, #16619, #25419 ) ;
#8660 = ORIENTED_EDGE ( 'NONE', *, *, #17205, .F. ) ;
#8661 = DIRECTION ( 'NONE',  ( 0.000000000000000000, 0.000000000000000000, 1.000000000000000000 ) ) ;
#8662 = DIRECTION ( 'NONE',  ( 1.000000000000000000, 0.000000000000000000, 0.000000000000000000 ) ) ;
#8663 = CARTESIAN_POINT ( 'NONE',  ( 3.352586340487470729, 3.837886065734355423, -0.05822226285683193558 ) ) ;
#8664 = ADVANCED_FACE ( 'NONE', ( #20957 ), #29671, .T. ) ;
#8665 = VERTEX_POINT ( 'NONE', #4270 ) ;
#8666 = FACE_OUTER_BOUND ( 'NONE', #1444, .T. ) ;
#8667 = FACE_BOUND ( 'NONE', #17430, .T. ) ;
#8668 = LINE ( 'NONE', #6221, #3449 ) ;
#8669 = FACE_OUTER_BOUND ( 'NONE', #27270, .T. ) ;
#8670 = CARTESIAN_POINT ( 'NONE',  ( -7.000003374631269537, -77.94228634059960825, 12.50000000000000000 ) ) ;
#8671 = CARTESIAN_POINT ( 'NONE',  ( 5.236872748402764621, 8.442024233997350580E-14, -4.057689166958447835 ) ) ;
#8672 = EDGE_CURVE ( 'NONE', #21445, #15730, #19496, .T. ) ;
#8673 = VECTOR ( 'NONE', #1200, 1000.000000000000000 ) ;
#8674 = VECTOR ( 'NONE', #22630, 1000.000000000000000 ) ;
#8675 = SURFACE_STYLE_USAGE ( .BOTH. , #3781 ) ;
#8676 = ADVANCED_FACE ( 'NONE', ( #29388 ), #26070, .T. ) ;
#8677 = DIRECTION ( 'NONE',  ( 1.000000000000000000, 0.000000000000000000, 0.000000000000000000 ) ) ;
#8678 = VERTEX_POINT ( 'NONE', #6524 ) ;
#8679 = LINE ( 'NONE', #31196, #30368 ) ;
#8680 = DIRECTION ( 'NONE',  ( 1.000000000000000000, 0.000000000000000000, 0.000000000000000000 ) ) ;
#8681 = CARTESIAN_POINT ( 'NONE',  ( 84.99999662536831124, -25.98076211353319565, -5.000000000000000000 ) ) ;
#8682 = ORIENTED_EDGE ( 'NONE', *, *, #3052, .T. ) ;
#8683 = VERTEX_POINT ( 'NONE', #35224 ) ;
#8684 = ORIENTED_EDGE ( 'NONE', *, *, #2824, .T. ) ;
#8685 = CIRCLE ( 'NONE', #30812, 2.000000000000001776 ) ;
#8686 = CARTESIAN_POINT ( 'NONE',  ( -58.00000337463104216, 51.96152422706639129, 12.50000000000000000 ) ) ;
#8687 = DIRECTION ( 'NONE',  ( 1.000000000000000000, 0.000000000000000000, 0.000000000000000000 ) ) ;
#8688 = CIRCLE ( 'NONE', #26645, 2.000000000000000000 ) ;
#8689 = CARTESIAN_POINT ( 'NONE',  ( 49.99999662536848177, -51.96152422706640550, -5.000000000000000000 ) ) ;
#8690 = ORIENTED_EDGE ( 'NONE', *, *, #24013, .T. ) ;
#8691 = CIRCLE ( 'NONE', #23060, 2.000000000000001776 ) ;
#8692 = AXIS2_PLACEMENT_3D ( 'NONE', #13130, #33574, #12729 ) ;
#8693 = FACE_OUTER_BOUND ( 'NONE', #27094, .T. ) ;
#8694 = EDGE_CURVE ( 'NONE', #5072, #5817, #32648, .T. ) ;
#8695 = ORIENTED_EDGE ( 'NONE', *, *, #23248, .T. ) ;
#8696 = CYLINDRICAL_SURFACE ( 'NONE', #4805, 2.000000000000001776 ) ;
#8697 = ORIENTED_EDGE ( 'NONE', *, *, #1490, .T. ) ;
#8698 = FACE_OUTER_BOUND ( 'NONE', #29792, .T. ) ;
#8699 = ORIENTED_EDGE ( 'NONE', *, *, #16938, .F. ) ;
#8700 = CONICAL_SURFACE ( 'NONE', #2086, 5.000000000000000888, 1.047197551196596299 ) ;
#8701 = ORIENTED_EDGE ( 'NONE', *, *, #107, .F. ) ;
#8702 = AXIS2_PLACEMENT_3D ( 'NONE', #27436, #30054, #24243 ) ;
#8703 = CARTESIAN_POINT ( 'NONE',  ( -23.00000337463120559, 77.94228634059957983, -9.999999999999998224 ) ) ;
#8704 = CARTESIAN_POINT ( 'NONE',  ( 16.99999662536863454, -77.94228634059960825, 12.50000000000000000 ) ) ;
#8705 = APPLICATION_CONTEXT ( 'automotive_design' ) ;
#8706 = VERTEX_POINT ( 'NONE', #32389 ) ;
#8707 = DIRECTION ( 'NONE',  ( 0.000000000000000000, 0.000000000000000000, 1.000000000000000000 ) ) ;
#8708 = DIRECTION ( 'NONE',  ( -1.000000000000000000, 0.000000000000000000, 0.000000000000000000 ) ) ;
#8709 = DIRECTION ( 'NONE',  ( 0.000000000000000000, 0.000000000000000000, -1.000000000000000000 ) ) ;
#8710 = ADVANCED_FACE ( 'NONE', ( #18525 ), #700, .F. ) ;
#8711 = CIRCLE ( 'NONE', #12270, 65.00000000000000000 ) ;
#8712 = ORIENTED_EDGE ( 'NONE', *, *, #19270, .F. ) ;
#8713 = CARTESIAN_POINT ( 'NONE',  ( -70.00000337463100664, -17.32050807568882078, -9.999999999999998224 ) ) ;
#8714 = DIRECTION ( 'NONE',  ( 0.000000000000000000, 1.000000000000000000, -1.625241993126352989E-15 ) ) ;
#8715 = ORIENTED_EDGE ( 'NONE', *, *, #8930, .F. ) ;
#8716 = EDGE_CURVE ( 'NONE', #5893, #12977, #8120, .T. ) ;
#8717 = DIRECTION ( 'NONE',  ( 1.000000000000000000, 0.000000000000000000, 0.000000000000000000 ) ) ;
#8718 = DIRECTION ( 'NONE',  ( 0.000000000000000000, 0.000000000000000000, 1.000000000000000000 ) ) ;
#8719 = DIRECTION ( 'NONE',  ( 1.000000000000000000, 0.000000000000000000, 0.000000000000000000 ) ) ;
#8720 = AXIS2_PLACEMENT_3D ( 'NONE', #33434, #36785, #24998 ) ;
#8721 = AXIS2_PLACEMENT_3D ( 'NONE', #1045, #21485, #15106 ) ;
#8722 = CARTESIAN_POINT ( 'NONE',  ( 25.00000000000000000, 3.061616997868383043E-15, -15.00000000000000000 ) ) ;
#8723 = EDGE_CURVE ( 'NONE', #30459, #17896, #6701, .T. ) ;
#8724 = CIRCLE ( 'NONE', #11709, 2.999999999999999556 ) ;
#8725 = VERTEX_POINT ( 'NONE', #12505 ) ;
#8726 = EDGE_CURVE ( 'NONE', #27343, #27468, #12290, .T. ) ;
#8727 = FACE_OUTER_BOUND ( 'NONE', #35035, .T. ) ;
#8728 = DIRECTION ( 'NONE',  ( 1.000000000000000000, 0.000000000000000000, 0.000000000000000000 ) ) ;
#8729 = EDGE_CURVE ( 'NONE', #1857, #24169, #5740, .T. ) ;
#8730 = ORIENTED_EDGE ( 'NONE', *, *, #29066, .T. ) ;
#8731 = AXIS2_PLACEMENT_3D ( 'NONE', #19433, #27508, #1824 ) ;
#8732 = ORIENTED_EDGE ( 'NONE', *, *, #24447, .T. ) ;
#8733 = ORIENTED_EDGE ( 'NONE', *, *, #34747, .F. ) ;
#8734 = DIRECTION ( 'NONE',  ( -0.7071067811865561215, -0.7071067811865389130, 0.000000000000000000 ) ) ;
#8735 = CARTESIAN_POINT ( 'NONE',  ( -62.97617850287781494, -4.279621169095772615, -4.999999999999997335 ) ) ;
#8736 = CARTESIAN_POINT ( 'NONE',  ( -95.00000000000001421, 1.163414459189985801E-14, -10.00000000000000000 ) ) ;
#8737 = EDGE_CURVE ( 'NONE', #22752, #24628, #25084, .T. ) ;
#8738 = AXIS2_PLACEMENT_3D ( 'NONE', #27626, #1379, #35705 ) ;
#8739 = EDGE_CURVE ( 'NONE', #13777, #14961, #20102, .T. ) ;
#8740 = EDGE_CURVE ( 'NONE', #10971, #15901, #11104, .T. ) ;
#8741 = AXIS2_PLACEMENT_3D ( 'NONE', #4395, #27804, #30453 ) ;
#8742 = DIRECTION ( 'NONE',  ( 1.000000000000000000, 0.000000000000000000, 0.000000000000000000 ) ) ;
#8744 = EDGE_CURVE ( 'NONE', #8936, #24850, #10258, .T. ) ;
#8743 = ORIENTED_EDGE ( 'NONE', *, *, #11274, .T. ) ;
#8745 = EDGE_CURVE ( 'NONE', #19466, #5465, #3935, .T. ) ;
#8746 = TOROIDAL_SURFACE ( 'NONE', #18231, 3.866666666667000651, 1.133333333332999793 ) ;
#8747 = DIRECTION ( 'NONE',  ( 1.000000000000000000, 0.000000000000000000, 0.000000000000000000 ) ) ;
#8748 = EDGE_LOOP ( 'NONE', ( #21671, #11461, #7163, #20905 ) ) ;
#8749 =( GEOMETRIC_REPRESENTATION_CONTEXT ( 3 ) GLOBAL_UNCERTAINTY_ASSIGNED_CONTEXT ( ( #5443 ) ) GLOBAL_UNIT_ASSIGNED_CONTEXT ( ( #4517, #27389, #35348 ) ) REPRESENTATION_CONTEXT ( 'NONE', 'WORKASPACE' ) );
#8750 = CARTESIAN_POINT ( 'NONE',  ( 0.000000000000000000, 0.000000000000000000, -5.000000000000000000 ) ) ;
#8751 = CIRCLE ( 'NONE', #9949, 150.0000000000000284 ) ;
#8752 = AXIS2_PLACEMENT_3D ( 'NONE', #34532, #6037, #20824 ) ;
#8753 = AXIS2_PLACEMENT_3D ( 'NONE', #10582, #27462, #33078 ) ;
#8754 = CIRCLE ( 'NONE', #25541, 2.000000000000001776 ) ;
#8755 = CARTESIAN_POINT ( 'NONE',  ( -2.775557561562891351E-14, 19.94802294027085310, -11.00000000000000000 ) ) ;
#8756 = DIRECTION ( 'NONE',  ( 0.8660254037844415942, 0.4999999999999949485, 0.000000000000000000 ) ) ;
#8757 = DIRECTION ( 'NONE',  ( 1.000000000000000000, 0.000000000000000000, 0.000000000000000000 ) ) ;
#8758 = CIRCLE ( 'NONE', #33898, 2.000000000000001776 ) ;
#8759 = DIRECTION ( 'NONE',  ( -0.000000000000000000, -0.000000000000000000, 1.000000000000000000 ) ) ;
#8760 = DIRECTION ( 'NONE',  ( 0.000000000000000000, 0.4999999999999953926, 0.8660254037844412611 ) ) ;
#8761 = CARTESIAN_POINT ( 'NONE',  ( 72.72667006429044534, -101.6652913307183610, 32.50002500000000083 ) ) ;
#8762 = ORIENTED_EDGE ( 'NONE', *, *, #19494, .T. ) ;
#8763 = DIRECTION ( 'NONE',  ( 0.000000000000000000, 0.000000000000000000, 1.000000000000000000 ) ) ;
#8764 = FACE_BOUND ( 'NONE', #31766, .T. ) ;
#8765 = CARTESIAN_POINT ( 'NONE',  ( 34.99999662536855283, -60.62177826491080168, -9.999999999999998224 ) ) ;
#8766 = AXIS2_PLACEMENT_3D ( 'NONE', #28545, #19757, #5330 ) ;
#8767 = ORIENTED_EDGE ( 'NONE', *, *, #26741, .T. ) ;
#8768 = ORIENTED_EDGE ( 'NONE', *, *, #16334, .T. ) ;
#8769 = CIRCLE ( 'NONE', #30313, 3.000000000000000444 ) ;
#8770 = VERTEX_POINT ( 'NONE', #36131 ) ;
#8771 = AXIS2_PLACEMENT_3D ( 'NONE', #23003, #33714, #30880 ) ;
#8772 = AXIS2_PLACEMENT_3D ( 'NONE', #25581, #22781, #7957 ) ;
#8773 = CIRCLE ( 'NONE', #9354, 3.500000000000003109 ) ;
#8774 = AXIS2_PLACEMENT_3D ( 'NONE', #5386, #28238, #2555 ) ;
#8775 = AXIS2_PLACEMENT_3D ( 'NONE', #32471, #15984, #27033 ) ;
#8776 = LINE ( 'NONE', #36908, #26393 ) ;
#8777 = AXIS2_PLACEMENT_3D ( 'NONE', #4825, #31048, #36510 ) ;
#8778 = CARTESIAN_POINT ( 'NONE',  ( -47.00000337463111322, 60.62177826491077326, 17.49999999999999645 ) ) ;
#8779 = FACE_OUTER_BOUND ( 'NONE', #23492, .T. ) ;
#8780 = CYLINDRICAL_SURFACE ( 'NONE', #12397, 65.00000000000000000 ) ;
#8781 = CARTESIAN_POINT ( 'NONE',  ( 6.808388610744110674E-13, 65.00000000000000000, 12.49999999999999822 ) ) ;
#8782 = EDGE_LOOP ( 'NONE', ( #24762, #34870, #15490, #31347 ) ) ;
#8783 = CIRCLE ( 'NONE', #32708, 2.000000000000001776 ) ;
#8784 = VERTEX_POINT ( 'NONE', #10632 ) ;
#8785 = LINE ( 'NONE', #27921, #5701 ) ;
#8786 = CARTESIAN_POINT ( 'NONE',  ( -70.00000337463100664, -17.32050807568882078, -9.999999999999998224 ) ) ;
#8787 = EDGE_CURVE ( 'NONE', #27221, #14606, #27308, .T. ) ;
#8788 = DIRECTION ( 'NONE',  ( -1.000000000000000000, 0.000000000000000000, 0.000000000000000000 ) ) ;
#8789 = VERTEX_POINT ( 'NONE', #36518 ) ;
#8790 = VECTOR ( 'NONE', #13881, 1000.000000000000000 ) ;
#8791 = CIRCLE ( 'NONE', #29742, 2.000000000000001776 ) ;
#8792 = DIRECTION ( 'NONE',  ( 0.000000000000000000, 0.000000000000000000, 1.000000000000000000 ) ) ;
#8793 = ORIENTED_EDGE ( 'NONE', *, *, #33830, .F. ) ;
#8794 = VERTEX_POINT ( 'NONE', #30675 ) ;
#8795 = DIRECTION ( 'NONE',  ( 0.000000000000000000, 0.000000000000000000, 1.000000000000000000 ) ) ;
#8796 = EDGE_LOOP ( 'NONE', ( #9766, #35220, #26287, #16667, #25042 ) ) ;
#8798 = CIRCLE ( 'NONE', #25015, 30.00000000000000000 ) ;
#8797 = SHAPE_REPRESENTATION_RELATIONSHIP ( 'NONE' , 'NONE' ,  #35880, #1854 ) ;
#8799 = VECTOR ( 'NONE', #9931, 1000.000000000000000 ) ;
#8800 = DIRECTION ( 'NONE',  ( -1.000000000000000000, 0.000000000000000000, 0.000000000000000000 ) ) ;
#8801 = CIRCLE ( 'NONE', #10010, 2.000000000000001776 ) ;
#8802 = CIRCLE ( 'NONE', #15394, 2.000000000000001776 ) ;
#8803 = CARTESIAN_POINT ( 'NONE',  ( 66.00000000000000000, 2.994873747314852478E-16, -2.445500000000000007 ) ) ;
#8804 = ORIENTED_EDGE ( 'NONE', *, *, #22911, .T. ) ;
#8805 = VERTEX_POINT ( 'NONE', #22076 ) ;
#8806 = ORIENTED_EDGE ( 'NONE', *, *, #1069, .F. ) ;
#8807 = EDGE_CURVE ( 'NONE', #6042, #33391, #2738, .T. ) ;
#8808 = VECTOR ( 'NONE', #31172, 1000.000000000000000 ) ;
#8809 = EDGE_LOOP ( 'NONE', ( #23642, #23929, #30346, #28485 ) ) ;
#8810 = ORIENTED_EDGE ( 'NONE', *, *, #7377, .F. ) ;
#8811 = CARTESIAN_POINT ( 'NONE',  ( 0.000000000000000000, 0.000000000000000000, -5.000000000000000000 ) ) ;
#8812 = DIRECTION ( 'NONE',  ( 1.000000000000000000, 0.000000000000000000, 0.000000000000000000 ) ) ;
#8813 = CYLINDRICAL_SURFACE ( 'NONE', #3504, 2.000000000000001776 ) ;
#8814 = DIRECTION ( 'NONE',  ( -1.000000000000000000, 0.000000000000000000, 0.000000000000000000 ) ) ;
#8815 = CARTESIAN_POINT ( 'NONE',  ( 42.97377950131529190, 96.90768712682505281, 27.49999999999999645 ) ) ;
#8816 = ORIENTED_EDGE ( 'NONE', *, *, #9959, .F. ) ;
#8817 = DIRECTION ( 'NONE',  ( 0.000000000000000000, -0.000000000000000000, -1.000000000000000000 ) ) ;
#8818 = AXIS2_PLACEMENT_3D ( 'NONE', #12584, #35482, #21204 ) ;
#8819 = EDGE_CURVE ( 'NONE', #6561, #19630, #24882, .T. ) ;
#8820 = CARTESIAN_POINT ( 'NONE',  ( 4.242640687119251908, -4.242640687119325626, 27.50000000000000000 ) ) ;
#8821 = CIRCLE ( 'NONE', #21997, 2.000000000000001776 ) ;
#8822 = CARTESIAN_POINT ( 'NONE',  ( 0.000000000000000000, 0.000000000000000000, 0.000000000000000000 ) ) ;
#8823 = ORIENTED_EDGE ( 'NONE', *, *, #851, .F. ) ;
#8824 = CYLINDRICAL_SURFACE ( 'NONE', #4096, 5.750000000000002665 ) ;
#8825 = LINE ( 'NONE', #20438, #17188 ) ;
#8826 = ORIENTED_EDGE ( 'NONE', *, *, #20513, .T. ) ;
#8827 = ORIENTED_EDGE ( 'NONE', *, *, #30070, .F. ) ;
#8828 = AXIS2_PLACEMENT_3D ( 'NONE', #5533, #8358, #16799 ) ;
#8829 = DIRECTION ( 'NONE',  ( 0.000000000000000000, 0.000000000000000000, 1.000000000000000000 ) ) ;
#8830 = CARTESIAN_POINT ( 'NONE',  ( -82.00000337463094979, -17.32050807568882078, -5.000000000000000000 ) ) ;
#8831 = EDGE_CURVE ( 'NONE', #9651, #20361, #21901, .T. ) ;
#8832 = DIRECTION ( 'NONE',  ( 0.000000000000000000, 0.000000000000000000, -1.000000000000000000 ) ) ;
#8833 = CARTESIAN_POINT ( 'NONE',  ( 21.99999662536862033, -86.60254037844400443, -9.999999999999998224 ) ) ;
#8834 = ORIENTED_EDGE ( 'NONE', *, *, #32258, .T. ) ;
#8835 = CIRCLE ( 'NONE', #17226, 2.000000000000001776 ) ;
#8836 = CARTESIAN_POINT ( 'NONE',  ( -86.45172111230354517, 31.46585318596159553, -49.86348611802629449 ) ) ;
#8837 = LINE ( 'NONE', #23279, #22535 ) ;
#8838 = CARTESIAN_POINT ( 'NONE',  ( -26.97173872511423198, 77.60723454213314199, 12.50000000000000000 ) ) ;
#8839 = AXIS2_PLACEMENT_3D ( 'NONE', #28566, #14333, #20131 ) ;
#8840 = VERTEX_POINT ( 'NONE', #7635 ) ;
#8841 = AXIS2_PLACEMENT_3D ( 'NONE', #8927, #286, #34258 ) ;
#8842 = AXIS2_PLACEMENT_3D ( 'NONE', #27198, #12390, #20847 ) ;
#8843 = CARTESIAN_POINT ( 'NONE',  ( 6.249999999999998224, 0.000000000000000000, 0.000000000000000000 ) ) ;
#8844 = ORIENTED_EDGE ( 'NONE', *, *, #13415, .F. ) ;
#8845 = VERTEX_POINT ( 'NONE', #4642 ) ;
#8846 = CARTESIAN_POINT ( 'NONE',  ( 5.000000000000000000, 2.886751345948125991, -6.000000000000000000 ) ) ;
#8847 = CIRCLE ( 'NONE', #14232, 2.000000000000001776 ) ;
#8848 = EDGE_CURVE ( 'NONE', #15428, #16100, #32038, .T. ) ;
#8849 = DIRECTION ( 'NONE',  ( 1.000000000000000000, 0.000000000000000000, 0.000000000000000000 ) ) ;
#8850 = ORIENTED_EDGE ( 'NONE', *, *, #16174, .T. ) ;
#8851 = VERTEX_POINT ( 'NONE', #13624 ) ;
#8852 = CARTESIAN_POINT ( 'NONE',  ( 64.99999662536839651, 60.62177826491078747, -9.999999999999998224 ) ) ;
#8853 = EDGE_CURVE ( 'NONE', #20458, #36216, #33279, .T. ) ;
#8854 = CARTESIAN_POINT ( 'NONE',  ( -52.39915983220772233, -35.19434990244957362, -4.999999999999997335 ) ) ;
#8855 = DIRECTION ( 'NONE',  ( 0.000000000000000000, 0.000000000000000000, -1.000000000000000000 ) ) ;
#8856 = AXIS2_PLACEMENT_3D ( 'NONE', #24582, #9932, #10303 ) ;
#8857 = ORIENTED_EDGE ( 'NONE', *, *, #20630, .T. ) ;
#8858 = LINE ( 'NONE', #11647, #6971 ) ;
#8859 = FACE_BOUND ( 'NONE', #9630, .T. ) ;
#8860 = EDGE_CURVE ( 'NONE', #3561, #18462, #313, .T. ) ;
#8861 = FACE_OUTER_BOUND ( 'NONE', #28606, .T. ) ;
#8862 = CARTESIAN_POINT ( 'NONE',  ( 0.000000000000000000, 85.61789592134881843, -27.49999999999990408 ) ) ;
#8863 = VECTOR ( 'NONE', #34414, 1000.000000000000000 ) ;
#8864 = CARTESIAN_POINT ( 'NONE',  ( 0.000000000000000000, 0.000000000000000000, -5.000000000000000000 ) ) ;
#8865 = DIRECTION ( 'NONE',  ( 0.000000000000000000, 0.000000000000000000, 1.000000000000000000 ) ) ;
#8866 = PRODUCT ( 'ventilated rotor', 'ventilated rotor', '', ( #30293 ) ) ;
#8867 = DIRECTION ( 'NONE',  ( -0.5000000000000101030, -0.8660254037844328234, 0.000000000000000000 ) ) ;
#8868 = EDGE_CURVE ( 'NONE', #27851, #16300, #30853, .T. ) ;
#8869 = AXIS2_PLACEMENT_3D ( 'NONE', #33018, #36032, #30388 ) ;
#8870 = DIRECTION ( 'NONE',  ( -1.000000000000000000, 0.000000000000000000, 0.000000000000000000 ) ) ;
#8871 = EDGE_LOOP ( 'NONE', ( #27816, #22008, #34634, #25872 ) ) ;
#8872 = CARTESIAN_POINT ( 'NONE',  ( 53.72396900529356145, 62.16182810592437846, 12.50000000000000000 ) ) ;
#8873 = VECTOR ( 'NONE', #31022, 1000.000000000000000 ) ;
#8874 = CIRCLE ( 'NONE', #29828, 95.00000000000001421 ) ;
#8875 = DIRECTION ( 'NONE',  ( 1.000000000000000000, 0.000000000000000000, 0.000000000000000000 ) ) ;
#8876 = CARTESIAN_POINT ( 'NONE',  ( -65.00000337463102085, 43.30127018922198801, 12.50000000000000000 ) ) ;
#8877 = ORIENTED_EDGE ( 'NONE', *, *, #30157, .T. ) ;
#8878 = EDGE_LOOP ( 'NONE', ( #177, #26588 ) ) ;
#8879 = EDGE_LOOP ( 'NONE', ( #2520, #12254, #19740, #17577, #9139, #17055 ) ) ;
#8880 = AXIS2_PLACEMENT_3D ( 'NONE', #15616, #13335, #4915 ) ;
#8881 = DIRECTION ( 'NONE',  ( -1.000000000000000000, 0.000000000000000000, 0.000000000000000000 ) ) ;
#8882 = DIRECTION ( 'NONE',  ( 0.000000000000000000, 0.000000000000000000, 1.000000000000000000 ) ) ;
#8883 = CYLINDRICAL_SURFACE ( 'NONE', #32167, 30.00000000000001421 ) ;
#8884 = ORIENTED_EDGE ( 'NONE', *, *, #14252, .T. ) ;
#8885 = CIRCLE ( 'NONE', #29245, 2.000000000000001776 ) ;
#8886 = CARTESIAN_POINT ( 'NONE',  ( 15.97563234535730814, -90.60231327712320137, 12.49999999999999822 ) ) ;
#8887 = EDGE_CURVE ( 'NONE', #6244, #18009, #27678, .T. ) ;
#8888 = ORIENTED_EDGE ( 'NONE', *, *, #4738, .T. ) ;
#8889 = CARTESIAN_POINT ( 'NONE',  ( -19.04446855847336195, -111.2114855601511607, 32.50000000000000711 ) ) ;
#8890 = VERTEX_POINT ( 'NONE', #1992 ) ;
#8891 = DIRECTION ( 'NONE',  ( 1.000000000000000000, 0.000000000000000000, 0.000000000000000000 ) ) ;
#8892 = AXIS2_PLACEMENT_3D ( 'NONE', #33553, #3605, #35991 ) ;
#8893 = VERTEX_POINT ( 'NONE', #16431 ) ;
#8894 = VERTEX_POINT ( 'NONE', #27859 ) ;
#8895 = ADVANCED_FACE ( 'NONE', ( #2182 ), #31865, .F. ) ;
#8896 = CARTESIAN_POINT ( 'NONE',  ( 0.000000000000000000, 0.000000000000000000, 0.000000000000000000 ) ) ;
#8897 = CARTESIAN_POINT ( 'NONE',  ( 3.453178355211938388, -3.779809238954861428, -0.7375898304884541679 ) ) ;
#8898 = CIRCLE ( 'NONE', #6494, 2.000000000000000000 ) ;
#8899 = ADVANCED_FACE ( 'NONE', ( #28716 ), #29765, .F. ) ;
#8900 = DIRECTION ( 'NONE',  ( 0.000000000000000000, 0.000000000000000000, 1.000000000000000000 ) ) ;
#8901 = ORIENTED_EDGE ( 'NONE', *, *, #10042, .T. ) ;
#8902 = LINE ( 'NONE', #32324, #11312 ) ;
#8903 = DIRECTION ( 'NONE',  ( -0.8660254037844449249, -0.4999999999999888423, 0.000000000000000000 ) ) ;
#8904 = DIRECTION ( 'NONE',  ( 0.000000000000000000, 0.000000000000000000, 1.000000000000000000 ) ) ;
#8905 = AXIS2_PLACEMENT_3D ( 'NONE', #10133, #32610, #32813 ) ;
#8906 = ORIENTED_EDGE ( 'NONE', *, *, #29451, .T. ) ;
#8907 = DIRECTION ( 'NONE',  ( 0.000000000000000000, -0.000000000000000000, -1.000000000000000000 ) ) ;
#8908 = DIRECTION ( 'NONE',  ( 1.000000000000000000, 0.000000000000000000, 0.000000000000000000 ) ) ;
#8909 = AXIS2_PLACEMENT_3D ( 'NONE', #36287, #31025, #7791 ) ;
#8910 = VERTEX_POINT ( 'NONE', #28879 ) ;
#8911 = CARTESIAN_POINT ( 'NONE',  ( 102.5304832720488832, -102.5304832720499633, 32.50000000000000000 ) ) ;
#8912 = DIRECTION ( 'NONE',  ( 0.000000000000000000, 0.000000000000000000, 1.000000000000000000 ) ) ;
#8913 = DIRECTION ( 'NONE',  ( -0.000000000000000000, -0.000000000000000000, -1.000000000000000000 ) ) ;
#8914 = AXIS2_PLACEMENT_3D ( 'NONE', #2048, #27924, #2249 ) ;
#8915 = CARTESIAN_POINT ( 'NONE',  ( -2.500000000000000888, 4.330127018922190985, -3.620524600599875686 ) ) ;
#8916 = AXIS2_PLACEMENT_3D ( 'NONE', #20841, #21026, #18202 ) ;
#8917 = CARTESIAN_POINT ( 'NONE',  ( 37.99999662536853151, -69.28203230275519786, 17.49999999999999645 ) ) ;
#8918 = EDGE_CURVE ( 'NONE', #23562, #4442, #4101, .T. ) ;
#8919 = ORIENTED_EDGE ( 'NONE', *, *, #14680, .F. ) ;
#8920 = DIRECTION ( 'NONE',  ( -0.000000000000000000, -0.000000000000000000, 1.000000000000000000 ) ) ;
#8921 = CARTESIAN_POINT ( 'NONE',  ( 24.99999662536859546, -77.94228634059960825, -5.000000000000000000 ) ) ;
#8922 = ORIENTED_EDGE ( 'NONE', *, *, #21943, .T. ) ;
#8923 = ORIENTED_EDGE ( 'NONE', *, *, #29972, .F. ) ;
#8924 = ORIENTED_EDGE ( 'NONE', *, *, #20598, .T. ) ;
#8925 = AXIS2_PLACEMENT_3D ( 'NONE', #15347, #12328, #30340 ) ;
#8926 = CARTESIAN_POINT ( 'NONE',  ( -58.88972745734155723, 34.00000000000049027, 12.49999999999999822 ) ) ;
#8927 = CARTESIAN_POINT ( 'NONE',  ( 59.99999662536842493, 51.96152422706639129, -9.999999999999998224 ) ) ;
#8928 = VECTOR ( 'NONE', #16921, 1000.000000000000000 ) ;
#8929 = CARTESIAN_POINT ( 'NONE',  ( -65.00000337463102085, 43.30127018922198801, 17.49999999999999645 ) ) ;
#8930 = EDGE_CURVE ( 'NONE', #22685, #16751, #34462, .T. ) ;
#8931 = DIRECTION ( 'NONE',  ( -0.000000000000000000, -0.000000000000000000, 1.000000000000000000 ) ) ;
#8932 = VERTEX_POINT ( 'NONE', #12001 ) ;
#8933 = CIRCLE ( 'NONE', #549, 33.00000000000001421 ) ;
#8934 = EDGE_CURVE ( 'NONE', #14791, #16685, #18282, .T. ) ;
#8935 = CARTESIAN_POINT ( 'NONE',  ( 39.99999662536853151, 69.28203230275518365, 12.50000000000000000 ) ) ;
#8936 = VERTEX_POINT ( 'NONE', #23459 ) ;
#8937 = FACE_BOUND ( 'NONE', #12914, .T. ) ;
#8938 = AXIS2_PLACEMENT_3D ( 'NONE', #25272, #11188, #2573 ) ;
#8939 = ADVANCED_FACE ( 'NONE', ( #18339 ), #25736, .F. ) ;
#8940 = AXIS2_PLACEMENT_3D ( 'NONE', #4852, #32969, #27697 ) ;
#8941 = DIRECTION ( 'NONE',  ( 0.000000000000000000, 0.000000000000000000, 1.000000000000000000 ) ) ;
#8942 = ADVANCED_FACE ( 'NONE', ( #195 ), #5650, .F. ) ;
#8943 = CARTESIAN_POINT ( 'NONE',  ( -50.00000337463112032, -51.96152422706641971, 17.49999999999999645 ) ) ;
#8944 = AXIS2_PLACEMENT_3D ( 'NONE', #20352, #31772, #6101 ) ;
#8945 = EDGE_CURVE ( 'NONE', #15238, #30923, #11687, .T. ) ;
#8946 = DIRECTION ( 'NONE',  ( -0.000000000000000000, -0.000000000000000000, 1.000000000000000000 ) ) ;
#8947 = CYLINDRICAL_SURFACE ( 'NONE', #288, 2.000000000000001776 ) ;
#8948 = CIRCLE ( 'NONE', #28700, 2.000000000000001776 ) ;
#8949 = CIRCLE ( 'NONE', #22749, 2.000000000000001776 ) ;
#8950 = FACE_OUTER_BOUND ( 'NONE', #29666, .T. ) ;
#8951 = CARTESIAN_POINT ( 'NONE',  ( -11.64413683707582337, -85.46375806488710225, 12.50000000000000000 ) ) ;
#8952 = ORIENTED_EDGE ( 'NONE', *, *, #22400, .F. ) ;
#8953 = DIRECTION ( 'NONE',  ( -0.000000000000000000, -0.000000000000000000, -1.000000000000000000 ) ) ;
#8954 = CIRCLE ( 'NONE', #31118, 5.750000000000002665 ) ;
#8955 = CARTESIAN_POINT ( 'NONE',  ( 79.99999662536833966, 17.32050807568879236, -9.999999999999998224 ) ) ;
#8956 = DIRECTION ( 'NONE',  ( -1.000000000000000000, 0.000000000000000000, 0.000000000000000000 ) ) ;
#8957 = EDGE_CURVE ( 'NONE', #22752, #3013, #14466, .T. ) ;
#8958 = ADVANCED_FACE ( 'NONE', ( #34897 ), #1522, .T. ) ;
#8959 = EDGE_LOOP ( 'NONE', ( #32351, #5010 ) ) ;
#8960 = ORIENTED_EDGE ( 'NONE', *, *, #11879, .F. ) ;
#8961 = ADVANCED_FACE ( 'NONE', ( #28522 ), #23278, .T. ) ;
#8962 = ORIENTED_EDGE ( 'NONE', *, *, #34641, .T. ) ;
#8963 = CARTESIAN_POINT ( 'NONE',  ( 84.99999662536832545, 25.98076211353319565, -9.999999999999998224 ) ) ;
#8964 = CIRCLE ( 'NONE', #15552, 2.000000000000001776 ) ;
#8965 = CARTESIAN_POINT ( 'NONE',  ( 0.000000000000000000, 0.000000000000000000, 12.49999999999999822 ) ) ;
#8966 = AXIS2_PLACEMENT_3D ( 'NONE', #25603, #19960, #37040 ) ;
#8967 = AXIS2_PLACEMENT_3D ( 'NONE', #24421, #35862, #1344 ) ;
#8968 = DIRECTION ( 'NONE',  ( 0.000000000000000000, 0.000000000000000000, 1.000000000000000000 ) ) ;
#8969 = CARTESIAN_POINT ( 'NONE',  ( -86.45172111230354517, 31.46585318596159553, 12.49999999999999822 ) ) ;
#8970 = DIRECTION ( 'NONE',  ( -0.000000000000000000, -0.000000000000000000, -1.000000000000000000 ) ) ;
#8971 = CIRCLE ( 'NONE', #27558, 3.000000000000002665 ) ;
#8972 = CARTESIAN_POINT ( 'NONE',  ( -65.00000337463102085, 60.62177826491077326, -9.999999999999998224 ) ) ;
#8973 = ORIENTED_EDGE ( 'NONE', *, *, #28616, .F. ) ;
#8974 = VERTEX_POINT ( 'NONE', #32045 ) ;
#8975 = DIRECTION ( 'NONE',  ( 0.000000000000000000, 0.000000000000000000, -1.000000000000000000 ) ) ;
#8976 = EDGE_CURVE ( 'NONE', #23027, #29875, #16526, .T. ) ;
#8977 = AXIS2_PLACEMENT_3D ( 'NONE', #26514, #9260, #17902 ) ;
#8978 = DIRECTION ( 'NONE',  ( 0.000000000000000000, -0.000000000000000000, -1.000000000000000000 ) ) ;
#8979 = ADVANCED_FACE ( 'NONE', ( #26274 ), #9024, .F. ) ;
#8980 = DIRECTION ( 'NONE',  ( 1.000000000000000000, 0.000000000000000000, 0.000000000000000000 ) ) ;
#8981 = VERTEX_POINT ( 'NONE', #22905 ) ;
#8982 = CIRCLE ( 'NONE', #8400, 2.000000000000001776 ) ;
#8983 = CARTESIAN_POINT ( 'NONE',  ( 67.99999662536838230, 34.64101615137758472, 17.49999999999999645 ) ) ;
#8984 = VERTEX_POINT ( 'NONE', #20278 ) ;
#8985 = EDGE_LOOP ( 'NONE', ( #24021, #564 ) ) ;
#8986 = EDGE_CURVE ( 'NONE', #27172, #7448, #20082, .T. ) ;
#8987 = CARTESIAN_POINT ( 'NONE',  ( -17.00000337463126243, 77.94228634059957983, 12.50000000000000000 ) ) ;
#8988 = ORIENTED_EDGE ( 'NONE', *, *, #15128, .F. ) ;
#8989 = AXIS2_PLACEMENT_3D ( 'NONE', #16149, #10499, #30575 ) ;
#8990 = DIRECTION ( 'NONE',  ( 0.000000000000000000, 0.000000000000000000, 1.000000000000000000 ) ) ;
#8991 = FACE_BOUND ( 'NONE', #27129, .T. ) ;
#8992 = VECTOR ( 'NONE', #28863, 1000.000000000000000 ) ;
#8993 = EDGE_LOOP ( 'NONE', ( #13235, #35587 ) ) ;
#8994 = ORIENTED_EDGE ( 'NONE', *, *, #15925, .T. ) ;
#8995 = CIRCLE ( 'NONE', #21592, 2.000000000000001776 ) ;
#8996 = ADVANCED_FACE ( 'NONE', ( #11626 ), #34531, .T. ) ;
#8997 = VERTEX_POINT ( 'NONE', #5013 ) ;
#8998 = EDGE_CURVE ( 'NONE', #10704, #23016, #18311, .T. ) ;
#8999 = VERTEX_POINT ( 'NONE', #4664 ) ;
#9000 = ORIENTED_EDGE ( 'NONE', *, *, #30048, .T. ) ;
#9001 = EDGE_CURVE ( 'NONE', #9038, #3252, #9895, .T. ) ;
#9002 = DIRECTION ( 'NONE',  ( 0.5000000000000038858, 0.8660254037844363761, 0.000000000000000000 ) ) ;
#9003 = EDGE_CURVE ( 'NONE', #22352, #34844, #7653, .T. ) ;
#9004 = FACE_OUTER_BOUND ( 'NONE', #34136, .T. ) ;
#9005 = CARTESIAN_POINT ( 'NONE',  ( 108.3061974404897825, -19.22934205795014151, 27.50000000000000000 ) ) ;
#9006 = DIRECTION ( 'NONE',  ( 1.000000000000000000, 0.000000000000000000, 0.000000000000000000 ) ) ;
#9007 = DIRECTION ( 'NONE',  ( 1.000000000000000000, 0.000000000000000000, 0.000000000000000000 ) ) ;
#9008 = ORIENTED_EDGE ( 'NONE', *, *, #27912, .F. ) ;
#9009 = DIRECTION ( 'NONE',  ( -1.000000000000000000, 0.000000000000000000, 0.000000000000000000 ) ) ;
#9010 = CARTESIAN_POINT ( 'NONE',  ( -3.057313426867661832, -4.281874658697595315, -4.057628883416056098 ) ) ;
#9011 = DIRECTION ( 'NONE',  ( 1.000000000000000000, 0.000000000000000000, 0.000000000000000000 ) ) ;
#9012 = ORIENTED_EDGE ( 'NONE', *, *, #4776, .F. ) ;
#9013 = DIRECTION ( 'NONE',  ( 0.000000000000000000, 0.000000000000000000, 1.000000000000000000 ) ) ;
#9014 = CARTESIAN_POINT ( 'NONE',  ( 0.000000000000000000, 0.000000000000000000, -25.03750572909317285 ) ) ;
#9015 = ORIENTED_EDGE ( 'NONE', *, *, #30057, .F. ) ;
#9016 = ORIENTED_EDGE ( 'NONE', *, *, #28873, .F. ) ;
#9017 = CARTESIAN_POINT ( 'NONE',  ( 37.99999662536853151, -69.28203230275519786, -9.999999999999998224 ) ) ;
#9018 = CARTESIAN_POINT ( 'NONE',  ( -59.13646009116099833, 70.47608876694653190, -49.22241343995295892 ) ) ;
#9019 = AXIS2_PLACEMENT_3D ( 'NONE', #28275, #16303, #22292 ) ;
#9020 = DIRECTION ( 'NONE',  ( -0.000000000000000000, -0.000000000000000000, -1.000000000000000000 ) ) ;
#9021 = CARTESIAN_POINT ( 'NONE',  ( 79.99999662536833966, 34.64101615137759183, -9.999999999999998224 ) ) ;
#9022 = ORIENTED_EDGE ( 'NONE', *, *, #20128, .T. ) ;
#9023 = ADVANCED_FACE ( 'NONE', ( #24899 ), #33541, .F. ) ;
#9024 = CYLINDRICAL_SURFACE ( 'NONE', #5765, 2.000000000000001776 ) ;
#9025 = CARTESIAN_POINT ( 'NONE',  ( -5.000000000000000888, 0.4965892259340443649, -0.01450341304856691757 ) ) ;
#9026 = DIRECTION ( 'NONE',  ( 0.000000000000000000, 0.000000000000000000, 1.000000000000000000 ) ) ;
#9027 = ORIENTED_EDGE ( 'NONE', *, *, #22, .F. ) ;
#9028 = DIRECTION ( 'NONE',  ( 0.000000000000000000, 0.000000000000000000, 1.000000000000000000 ) ) ;
#9029 = VERTEX_POINT ( 'NONE', #32968 ) ;
#9030 = CARTESIAN_POINT ( 'NONE',  ( -41.00000000000000000, 103.4105893997321886, -19.99999999999999645 ) ) ;
#9031 = LINE ( 'NONE', #29075, #10999 ) ;
#9032 = DIRECTION ( 'NONE',  ( 1.000000000000000000, 0.000000000000000000, 0.000000000000000000 ) ) ;
#9033 = ORIENTED_EDGE ( 'NONE', *, *, #30558, .T. ) ;
#9034 = EDGE_LOOP ( 'NONE', ( #33361, #6885, #23497, #25388 ) ) ;
#9035 = CARTESIAN_POINT ( 'NONE',  ( 27.99999662536855993, 69.28203230275518365, -5.000000000000000000 ) ) ;
#9036 = CARTESIAN_POINT ( 'NONE',  ( 5.999999999999998224, 6.123233995736766282E-16, -5.000000000000000000 ) ) ;
#9037 = CYLINDRICAL_SURFACE ( 'NONE', #13707, 2.000000000000001776 ) ;
#9038 = VERTEX_POINT ( 'NONE', #1653 ) ;
#9039 = DIRECTION ( 'NONE',  ( -1.000000000000000000, 0.000000000000000000, 0.000000000000000000 ) ) ;
#9040 = AXIS2_PLACEMENT_3D ( 'NONE', #27363, #26993, #18575 ) ;
#9041 = EDGE_CURVE ( 'NONE', #26406, #6520, #19107, .T. ) ;
#9042 = FACE_BOUND ( 'NONE', #4929, .T. ) ;
#9043 = DIRECTION ( 'NONE',  ( 0.000000000000000000, 0.000000000000000000, 1.000000000000000000 ) ) ;
#9044 = CARTESIAN_POINT ( 'NONE',  ( -90.00000337463090716, -1.040834085586084257E-14, 17.49999999999999645 ) ) ;
#9045 = LINE ( 'NONE', #1169, #14704 ) ;
#9046 = CARTESIAN_POINT ( 'NONE',  ( -27.00000337463121625, -77.94228634059963667, 12.50000000000000000 ) ) ;
#9047 = CARTESIAN_POINT ( 'NONE',  ( -80.00000337463094979, -2.428612866367529932E-14, -9.999999999999998224 ) ) ;
#9048 = CARTESIAN_POINT ( 'NONE',  ( -82.27241335952211898, -47.49999999999924682, 32.50002500000000083 ) ) ;
#9049 = ORIENTED_EDGE ( 'NONE', *, *, #925, .F. ) ;
#9050 = DIRECTION ( 'NONE',  ( 0.000000000000000000, 0.000000000000000000, -1.000000000000000000 ) ) ;
#9051 = FACE_BOUND ( 'NONE', #32229, .T. ) ;
#9052 = DIRECTION ( 'NONE',  ( 1.000000000000000000, 0.000000000000000000, 0.000000000000000000 ) ) ;
#9053 = EDGE_LOOP ( 'NONE', ( #6959, #36530, #27729, #13430 ) ) ;
#9054 = ORIENTED_EDGE ( 'NONE', *, *, #9739, .T. ) ;
#9055 = ORIENTED_EDGE ( 'NONE', *, *, #29588, .F. ) ;
#9056 = DIRECTION ( 'NONE',  ( 0.000000000000000000, 0.000000000000000000, 1.000000000000000000 ) ) ;
#9057 = DIRECTION ( 'NONE',  ( 0.000000000000000000, 0.000000000000000000, 1.000000000000000000 ) ) ;
#9058 = DIRECTION ( 'NONE',  ( 0.000000000000000000, 0.000000000000000000, 1.000000000000000000 ) ) ;
#9059 = ORIENTED_EDGE ( 'NONE', *, *, #9445, .T. ) ;
#9060 = AXIS2_PLACEMENT_3D ( 'NONE', #12165, #15019, #9751 ) ;
#9061 = EDGE_CURVE ( 'NONE', #24391, #13923, #8758, .T. ) ;
#9062 = CYLINDRICAL_SURFACE ( 'NONE', #25700, 33.00000000000001421 ) ;
#9063 = ORIENTED_EDGE ( 'NONE', *, *, #17873, .F. ) ;
#9064 = DIRECTION ( 'NONE',  ( 0.000000000000000000, 0.000000000000000000, -1.000000000000000000 ) ) ;
#9065 = PRODUCT_DEFINITION ( 'UNKNOWN', '', #2189, #149 ) ;
#9066 = ORIENTED_EDGE ( 'NONE', *, *, #17790, .T. ) ;
#9067 = CARTESIAN_POINT ( 'NONE',  ( 4.999996625368676284, -77.94228634059960825, -9.999999999999998224 ) ) ;
#9068 = ORIENTED_EDGE ( 'NONE', *, *, #2210, .T. ) ;
#9069 = ORIENTED_EDGE ( 'NONE', *, *, #22572, .F. ) ;
#9070 = EDGE_CURVE ( 'NONE', #31694, #26322, #10554, .T. ) ;
#9071 = DIRECTION ( 'NONE',  ( 1.000000000000000000, 0.000000000000000000, 0.000000000000000000 ) ) ;
#9072 = DIRECTION ( 'NONE',  ( -0.000000000000000000, -0.000000000000000000, 1.000000000000000000 ) ) ;
#9073 = CARTESIAN_POINT ( 'NONE',  ( -80.00000337463094979, -17.32050807568882078, -9.999999999999998224 ) ) ;
#9074 = ORIENTED_EDGE ( 'NONE', *, *, #23385, .T. ) ;
#9075 = LINE ( 'NONE', #11693, #15494 ) ;
#9076 = FACE_OUTER_BOUND ( 'NONE', #25047, .T. ) ;
#9077 = LINE ( 'NONE', #20692, #20261 ) ;
#9078 = ORIENTED_EDGE ( 'NONE', *, *, #2624, .F. ) ;
#9079 = CARTESIAN_POINT ( 'NONE',  ( 1.999996625368672287, 86.60254037844397601, -5.000000000000000000 ) ) ;
#9080 = FACE_OUTER_BOUND ( 'NONE', #25614, .T. ) ;
#9081 = CIRCLE ( 'NONE', #1893, 2.000000000000001776 ) ;
#9082 = ORIENTED_EDGE ( 'NONE', *, *, #12379, .F. ) ;
#9083 = EDGE_CURVE ( 'NONE', #21528, #16067, #21888, .T. ) ;
#9084 = CYLINDRICAL_SURFACE ( 'NONE', #23214, 3.000000000000002665 ) ;
#9085 = AXIS2_PLACEMENT_3D ( 'NONE', #33985, #28327, #379 ) ;
#9086 = CARTESIAN_POINT ( 'NONE',  ( -40.00000337463113453, -69.28203230275519786, 17.49999999999999645 ) ) ;
#9087 = CARTESIAN_POINT ( 'NONE',  ( -58.88972745734155723, 34.00000000000049027, -49.22241343995295892 ) ) ;
#9088 = CARTESIAN_POINT ( 'NONE',  ( 0.000000000000000000, 89.94802294027088863, 32.49999999999999289 ) ) ;
#9089 = LINE ( 'NONE', #18085, #24512 ) ;
#9090 = CARTESIAN_POINT ( 'NONE',  ( 62.99999662536842493, 43.30127018922200222, -9.999999999999998224 ) ) ;
#9091 = ORIENTED_EDGE ( 'NONE', *, *, #30727, .F. ) ;
#9092 = CARTESIAN_POINT ( 'NONE',  ( 76.99999662536836809, 25.98076211353319565, 12.50000000000000000 ) ) ;
#9093 = CARTESIAN_POINT ( 'NONE',  ( -63.00000337463102085, 25.98076211353317433, 17.49999999999999645 ) ) ;
#9094 = PLANE ( 'NONE',  #12160 ) ;
#9096 = EDGE_CURVE ( 'NONE', #14947, #2754, #21532, .T. ) ;
#9095 = ORIENTED_EDGE ( 'NONE', *, *, #32301, .F. ) ;
#9097 = EDGE_LOOP ( 'NONE', ( #22892, #3010, #35727, #8415 ) ) ;
#9098 = ORIENTED_EDGE ( 'NONE', *, *, #34645, .F. ) ;
#9099 = EDGE_CURVE ( 'NONE', #9326, #15905, #22517, .T. ) ;
#9100 = DIRECTION ( 'NONE',  ( 1.000000000000000000, 0.000000000000000000, 0.000000000000000000 ) ) ;
#9101 = LINE ( 'NONE', #6288, #23220 ) ;
#9102 = LINE ( 'NONE', #9283, #32643 ) ;
#9103 = CIRCLE ( 'NONE', #30064, 2.000000000000000000 ) ;
#9104 = DIRECTION ( 'NONE',  ( 0.000000000000000000, 0.000000000000000000, 1.000000000000000000 ) ) ;
#9105 = ORIENTED_EDGE ( 'NONE', *, *, #7302, .T. ) ;
#9106 = DIRECTION ( 'NONE',  ( 0.000000000000000000, 0.000000000000000000, 1.000000000000000000 ) ) ;
#9107 = ADVANCED_FACE ( 'NONE', ( #18898 ), #12694, .T. ) ;
#9108 = ORIENTED_EDGE ( 'NONE', *, *, #16661, .F. ) ;
#9109 = FACE_BOUND ( 'NONE', #20920, .T. ) ;
#9110 = EDGE_CURVE ( 'NONE', #32261, #24840, #9336, .T. ) ;
#9111 = CARTESIAN_POINT ( 'NONE',  ( 0.000000000000000000, 0.000000000000000000, -15.00000000000000000 ) ) ;
#9112 = CARTESIAN_POINT ( 'NONE',  ( 4.897544501024384282E-15, 69.94802294027087441, -19.99999999999999645 ) ) ;
#9113 = EDGE_LOOP ( 'NONE', ( #29560, #541, #25039, #6726, #1858 ) ) ;
#9114 = LINE ( 'NONE', #28806, #20631 ) ;
#9115 =( NAMED_UNIT ( * ) PLANE_ANGLE_UNIT ( ) SI_UNIT ( $, .RADIAN. ) );
#9116 = CARTESIAN_POINT ( 'NONE',  ( 67.99999662536838230, -17.32050807568879947, -9.999999999999998224 ) ) ;
#9117 = AXIS2_PLACEMENT_3D ( 'NONE', #35090, #31874, #20834 ) ;
#9118 = CIRCLE ( 'NONE', #11527, 2.000000000000001776 ) ;
#9119 = DIRECTION ( 'NONE',  ( 0.000000000000000000, 0.000000000000000000, 1.000000000000000000 ) ) ;
#9120 = DIRECTION ( 'NONE',  ( 0.000000000000000000, 0.000000000000000000, 1.000000000000000000 ) ) ;
#9121 = ORIENTED_EDGE ( 'NONE', *, *, #16543, .T. ) ;
#9122 = CYLINDRICAL_SURFACE ( 'NONE', #2232, 2.000000000000001776 ) ;
#9123 = DIRECTION ( 'NONE',  ( 0.000000000000000000, 0.000000000000000000, 1.000000000000000000 ) ) ;
#9124 = CARTESIAN_POINT ( 'NONE',  ( -19.31922176934808633, 76.99660315353983719, -19.99999999999999645 ) ) ;
#9125 = VERTEX_POINT ( 'NONE', #32777 ) ;
#9126 = EDGE_CURVE ( 'NONE', #21452, #35244, #24715, .T. ) ;
#9127 = ORIENTED_EDGE ( 'NONE', *, *, #22966, .T. ) ;
#9128 = AXIS2_PLACEMENT_3D ( 'NONE', #16301, #13465, #1862 ) ;
#9129 = VERTEX_POINT ( 'NONE', #29964 ) ;
#9130 = CARTESIAN_POINT ( 'NONE',  ( 74.99999662536835388, -25.98076211353319565, -9.999999999999998224 ) ) ;
#9131 = EDGE_CURVE ( 'NONE', #24647, #20619, #4567, .T. ) ;
#9132 = PLANE ( 'NONE',  #23422 ) ;
#9133 = EDGE_CURVE ( 'NONE', #20202, #16545, #8148, .T. ) ;
#9134 = DIRECTION ( 'NONE',  ( 0.000000000000000000, 0.000000000000000000, -1.000000000000000000 ) ) ;
#9135 = DIRECTION ( 'NONE',  ( 0.000000000000000000, 0.000000000000000000, -1.000000000000000000 ) ) ;
#9136 = CARTESIAN_POINT ( 'NONE',  ( 31.83425564451589196, 89.42901512340320380, -5.000000000000011546 ) ) ;
#9137 = CARTESIAN_POINT ( 'NONE',  ( 84.99999662536831124, -25.98076211353319565, -9.999999999999998224 ) ) ;
#9138 = EDGE_LOOP ( 'NONE', ( #16835, #29398, #14431, #17781 ) ) ;
#9139 = ORIENTED_EDGE ( 'NONE', *, *, #25907, .T. ) ;
#9140 = CIRCLE ( 'NONE', #31304, 2.000000000000001776 ) ;
#9141 = CARTESIAN_POINT ( 'NONE',  ( -34.60911769017402406, 75.98085615278088767, 12.50000000000000000 ) ) ;
#9142 = CYLINDRICAL_SURFACE ( 'NONE', #26544, 30.00000000000001421 ) ;
#9143 = DIRECTION ( 'NONE',  ( -0.000000000000000000, -0.000000000000000000, 1.000000000000000000 ) ) ;
#9144 = ORIENTED_EDGE ( 'NONE', *, *, #8807, .T. ) ;
#9145 = EDGE_CURVE ( 'NONE', #16686, #9342, #965, .T. ) ;
#9146 = FACE_BOUND ( 'NONE', #20648, .T. ) ;
#9147 = EDGE_LOOP ( 'NONE', ( #17328, #36391, #164, #32399 ) ) ;
#9148 = CIRCLE ( 'NONE', #27115, 3.500000000000003109 ) ;
#9149 = ORIENTED_EDGE ( 'NONE', *, *, #27411, .T. ) ;
#9150 = CARTESIAN_POINT ( 'NONE',  ( 29.99999662536856349, 69.28203230275518365, -5.000000000000000000 ) ) ;
#9151 = ORIENTED_EDGE ( 'NONE', *, *, #34396, .F. ) ;
#9152 = FACE_OUTER_BOUND ( 'NONE', #17944, .T. ) ;
#9153 = CARTESIAN_POINT ( 'NONE',  ( 2.925285743277526329, 4.084588180558403891, -5.989444439476610427 ) ) ;
#9154 = CARTESIAN_POINT ( 'NONE',  ( 39.27785635698568711, -86.50000000000001421, 32.50000000000000000 ) ) ;
#9155 = ORIENTED_EDGE ( 'NONE', *, *, #35306, .T. ) ;
#9156 = VERTEX_POINT ( 'NONE', #33339 ) ;
#9157 = AXIS2_PLACEMENT_3D ( 'NONE', #23129, #28375, #19782 ) ;
#9158 = VERTEX_POINT ( 'NONE', #10274 ) ;
#9159 = VERTEX_POINT ( 'NONE', #1842 ) ;
#9160 = AXIS2_PLACEMENT_3D ( 'NONE', #9534, #35781, #35237 ) ;
#9161 = EDGE_CURVE ( 'NONE', #34031, #34992, #15937, .T. ) ;
#9162 = EDGE_LOOP ( 'NONE', ( #14890, #6265, #11326, #32054 ) ) ;
#9163 = DIRECTION ( 'NONE',  ( -0.000000000000000000, -0.000000000000000000, 1.000000000000000000 ) ) ;
#9164 = CARTESIAN_POINT ( 'NONE',  ( -20.00000337463122690, 86.60254037844397601, -9.999999999999998224 ) ) ;
#9165 = ADVANCED_FACE ( 'NONE', ( #22999 ), #2956, .F. ) ;
#9166 = EDGE_LOOP ( 'NONE', ( #29432, #652 ) ) ;
#9167 = FACE_OUTER_BOUND ( 'NONE', #16611, .T. ) ;
#9168 = CARTESIAN_POINT ( 'NONE',  ( 80.47882414735005341, 72.44490339922796807, 32.49999999999998579 ) ) ;
#9169 = DIRECTION ( 'NONE',  ( 0.000000000000000000, 0.000000000000000000, -1.000000000000000000 ) ) ;
#9170 = ORIENTED_EDGE ( 'NONE', *, *, #29414, .T. ) ;
#9171 = FACE_OUTER_BOUND ( 'NONE', #7441, .T. ) ;
#9172 = AXIS2_PLACEMENT_3D ( 'NONE', #2369, #30104, #24865 ) ;
#9173 = ADVANCED_FACE ( 'NONE', ( #25827 ), #28625, .F. ) ;
#9174 = DIRECTION ( 'NONE',  ( -0.000000000000000000, -0.000000000000000000, -1.000000000000000000 ) ) ;
#9175 = DIRECTION ( 'NONE',  ( 0.000000000000000000, 0.000000000000000000, 1.000000000000000000 ) ) ;
#9176 = ORIENTED_EDGE ( 'NONE', *, *, #22572, .T. ) ;
#9177 = CARTESIAN_POINT ( 'NONE',  ( 3.108933952041194271, 78.59334852315024023, 12.50000000000000000 ) ) ;
#9178 = EDGE_CURVE ( 'NONE', #19731, #18123, #2755, .T. ) ;
#9179 = CARTESIAN_POINT ( 'NONE',  ( -30.00000337463119848, -69.28203230275522628, -9.999999999999998224 ) ) ;
#9180 = ADVANCED_FACE ( 'NONE', ( #31251 ), #14384, .T. ) ;
#9181 = AXIS2_PLACEMENT_3D ( 'NONE', #31775, #3286, #17180 ) ;
#9182 = ORIENTED_EDGE ( 'NONE', *, *, #10544, .F. ) ;
#9183 = ORIENTED_EDGE ( 'NONE', *, *, #3045, .T. ) ;
#9184 = LINE ( 'NONE', #9378, #18850 ) ;
#9185 = FACE_OUTER_BOUND ( 'NONE', #13229, .T. ) ;
#9186 = CYLINDRICAL_SURFACE ( 'NONE', #7897, 33.00000000000001421 ) ;
#9187 =( REPRESENTATION_RELATIONSHIP ('NONE','NONE', #15268, #34443 ) REPRESENTATION_RELATIONSHIP_WITH_TRANSFORMATION ( #19412 )SHAPE_REPRESENTATION_RELATIONSHIP( ) );
#9188 = DIRECTION ( 'NONE',  ( 1.000000000000000000, 0.000000000000000000, 0.000000000000000000 ) ) ;
#9189 = ORIENTED_EDGE ( 'NONE', *, *, #31314, .T. ) ;
#9190 = ADVANCED_FACE ( 'NONE', ( #11383, #33705, #19645, #31428, #25443, #14190, #30872, #11191, #22440, #34091, #25649, #20189, #31617, #5208, #5567, #22268, #5953, #17004, #17384, #2404, #10998, #2204, #13641, #34266, #25102, #13829, #33890, #10838, #8011, #19450, #16646, #5753, #28076, #25275, #8566, #19999, #36700, #5402, #16836, #28254, #2575, #36882, #22643, #8396, #19828, #23193, #3851, #31957, #20534, #12476, #26733, #3300, #32364, #21106, #6296, #15293, #31790, #23383, #6119, #1050, #18104, #6848, #17547, #23942, #12268, #35394, #9679, #32531, #14738, #28803, #11921, #3128, #9109, #14552, #35194, #15110, #34639, #25992, #20726, #20373, #26183, #9500, #294, #11730, #28971, #8937, #499, #17733, #29529, #32162, #34817, #29173, #3681, #3505, #14941, #26372, #678, #12089, #23549, #34993, #9291, #6500, #26542, #17935, #29366, #853, #23744, #20934, #6680, #32727, #16238, #7601, #7416, #19054, #29921, #1411, #13395, #33490, #18290, #15495, #10405, #7053, #7242, #1241, #21842, #10051, #27655, #18675, #21667, #30279, #12658, #29719, #22043, #4053, #24853, #36292, #15676, #4614, #33286, #18856 ), #4804, .T. ) ;
#9191 = CARTESIAN_POINT ( 'NONE',  ( 79.99999662536833966, 17.32050807568879236, -9.999999999999998224 ) ) ;
#9192 = DIRECTION ( 'NONE',  ( 1.000000000000000000, 0.000000000000000000, 0.000000000000000000 ) ) ;
#9193 = EDGE_CURVE ( 'NONE', #29609, #31054, #20133, .T. ) ;
#9194 = CARTESIAN_POINT ( 'NONE',  ( 5.000000000000002665, -2.886751345948134873, -5.553418012614792509 ) ) ;
#9195 = AXIS2_PLACEMENT_3D ( 'NONE', #18321, #10260, #13255 ) ;
#9196 = EDGE_CURVE ( 'NONE', #18736, #8614, #24939, .T. ) ;
#9197 = ORIENTED_EDGE ( 'NONE', *, *, #13181, .T. ) ;
#9198 = ADVANCED_FACE ( 'NONE', ( #26925 ), #24675, .F. ) ;
#9199 = CARTESIAN_POINT ( 'NONE',  ( -85.00000337463092137, -25.98076211353322051, 12.50000000000000000 ) ) ;
#9200 = EDGE_LOOP ( 'NONE', ( #16780, #27396, #29159, #20574 ) ) ;
#9201 = CARTESIAN_POINT ( 'NONE',  ( -72.00000337463100664, 51.96152422706637708, 12.50000000000000000 ) ) ;
#9202 = LINE ( 'NONE', #6595, #36175 ) ;
#9203 = VECTOR ( 'NONE', #2081, 1000.000000000000000 ) ;
#9204 = DIRECTION ( 'NONE',  ( 1.000000000000000000, 0.000000000000000000, 0.000000000000000000 ) ) ;
#9205 = ORIENTED_EDGE ( 'NONE', *, *, #25346, .F. ) ;
#9206 = VERTEX_POINT ( 'NONE', #27097 ) ;
#9207 = CARTESIAN_POINT ( 'NONE',  ( -6.069707180676227632E-15, 5.773502691896268857, -5.700000000000000178 ) ) ;
#9208 = LINE ( 'NONE', #20638, #7654 ) ;
#9209 = CARTESIAN_POINT ( 'NONE',  ( 62.19434990244977257, -52.39915983220758022, -4.999999999999997335 ) ) ;
#9210 = VERTEX_POINT ( 'NONE', #9846 ) ;
#9211 = FACE_OUTER_BOUND ( 'NONE', #30486, .T. ) ;
#9212 = FACE_BOUND ( 'NONE', #36289, .T. ) ;
#9213 = DIRECTION ( 'NONE',  ( 1.000000000000000000, 0.000000000000000000, 0.000000000000000000 ) ) ;
#9214 = DIRECTION ( 'NONE',  ( -0.000000000000000000, -0.000000000000000000, 1.000000000000000000 ) ) ;
#9215 = PLANE ( 'NONE',  #20693 ) ;
#9216 = VERTEX_POINT ( 'NONE', #21286 ) ;
#9217 = DIRECTION ( 'NONE',  ( -1.000000000000000000, 0.000000000000000000, 0.000000000000000000 ) ) ;
#9218 = COLOUR_RGB ( '', 0.09019608, 0.27058824, 0.51372549) ;
#9219 = DIRECTION ( 'NONE',  ( 1.000000000000000000, 0.000000000000000000, 0.000000000000000000 ) ) ;
#9220 = DIRECTION ( 'NONE',  ( 0.000000000000000000, 0.000000000000000000, 1.000000000000000000 ) ) ;
#9221 = ORIENTED_EDGE ( 'NONE', *, *, #17457, .T. ) ;
#9222 = CARTESIAN_POINT ( 'NONE',  ( 3.000000000000000000, 2.935248768560057453, -3.903127820947815962E-15 ) ) ;
#9223 = CARTESIAN_POINT ( 'NONE',  ( 59.99999662536843914, -34.64101615137759893, 12.50000000000000000 ) ) ;
#9224 = CARTESIAN_POINT ( 'NONE',  ( 1.999996625368672287, 86.60254037844397601, -9.999999999999998224 ) ) ;
#9225 = VECTOR ( 'NONE', #4157, 1000.000000000000000 ) ;
#9226 = ORIENTED_EDGE ( 'NONE', *, *, #8044, .T. ) ;
#9227 = VERTEX_POINT ( 'NONE', #18499 ) ;
#9228 = VERTEX_POINT ( 'NONE', #15852 ) ;
#9229 = AXIS2_PLACEMENT_3D ( 'NONE', #30357, #13674, #33166 ) ;
#9230 = DIRECTION ( 'NONE',  ( 1.000000000000000000, 0.000000000000000000, 0.000000000000000000 ) ) ;
#9231 = FACE_OUTER_BOUND ( 'NONE', #23205, .T. ) ;
#9232 = CARTESIAN_POINT ( 'NONE',  ( 82.99999662536832545, 8.660254037844394404, -5.000000000000000000 ) ) ;
#9233 = EDGE_LOOP ( 'NONE', ( #930, #8052, #16369, #19779, #12946, #5152 ) ) ;
#9234 = VERTEX_POINT ( 'NONE', #12835 ) ;
#9235 = ORIENTED_EDGE ( 'NONE', *, *, #4540, .F. ) ;
#9236 =( BOUNDED_CURVE ( )  B_SPLINE_CURVE ( 3, ( #31604, #23732, #17924, #6490 ),
 .UNSPECIFIED., .F., .F. ) 
 B_SPLINE_CURVE_WITH_KNOTS ( ( 4, 4 ),
 ( 0.000000000000000000, 1.570796326794907438 ),
 .UNSPECIFIED. ) 
 CURVE ( )  GEOMETRIC_REPRESENTATION_ITEM ( )  RATIONAL_B_SPLINE_CURVE ( ( 1.000000000000000000, 0.8047378541243623840, 0.8047378541243623840, 1.000000000000000000 ) ) 
 REPRESENTATION_ITEM ( '' )  );
#9237 = LINE ( 'NONE', #11677, #9525 ) ;
#9238 = ORIENTED_EDGE ( 'NONE', *, *, #17772, .F. ) ;
#9239 = EDGE_CURVE ( 'NONE', #19593, #31910, #29704, .T. ) ;
#9240 = CARTESIAN_POINT ( 'NONE',  ( 6.532899837730827386, 0.000000000000000000, -5.132899837730832360 ) ) ;
#9241 = AXIS2_PLACEMENT_3D ( 'NONE', #14805, #34503, #9002 ) ;
#9242 = EDGE_LOOP ( 'NONE', ( #26798, #19086, #16947, #27586 ) ) ;
#9243 = CARTESIAN_POINT ( 'NONE',  ( 101.7384897088143560, -110.2237710830540180, 32.55002500000000509 ) ) ;
#9244 = EDGE_LOOP ( 'NONE', ( #31173, #21139 ) ) ;
#9245 = EDGE_LOOP ( 'NONE', ( #36968, #14080, #17600, #29572 ) ) ;
#9246 = AXIS2_PLACEMENT_3D ( 'NONE', #5050, #13479, #4702 ) ;
#9247 = DIRECTION ( 'NONE',  ( 0.000000000000000000, 0.000000000000000000, 1.000000000000000000 ) ) ;
#9248 = CYLINDRICAL_SURFACE ( 'NONE', #17221, 33.00000000000001421 ) ;
#9249 = LINE ( 'NONE', #26142, #13457 ) ;
#9250 = EDGE_LOOP ( 'NONE', ( #7783, #2613 ) ) ;
#9251 = ORIENTED_EDGE ( 'NONE', *, *, #24473, .F. ) ;
#9252 = DIRECTION ( 'NONE',  ( 0.000000000000000000, 0.000000000000000000, 1.000000000000000000 ) ) ;
#9253 = CIRCLE ( 'NONE', #5067, 2.000000000000001776 ) ;
#9254 = CARTESIAN_POINT ( 'NONE',  ( 79.99999662536833966, -3.469446951953614189E-15, 12.50000000000000000 ) ) ;
#9255 = AXIS2_PLACEMENT_3D ( 'NONE', #19322, #33585, #36581 ) ;
#9256 = CARTESIAN_POINT ( 'NONE',  ( -37.00000337463116296, 77.94228634059957983, -9.999999999999998224 ) ) ;
#9257 = ORIENTED_EDGE ( 'NONE', *, *, #36264, .T. ) ;
#9258 = CIRCLE ( 'NONE', #21849, 27.00000000000001421 ) ;
#9259 = DIRECTION ( 'NONE',  ( 1.000000000000000000, 0.000000000000000000, 0.000000000000000000 ) ) ;
#9260 = DIRECTION ( 'NONE',  ( 0.000000000000000000, 0.000000000000000000, -1.000000000000000000 ) ) ;
#9261 = ORIENTED_EDGE ( 'NONE', *, *, #27481, .T. ) ;
#9262 = DIRECTION ( 'NONE',  ( 0.000000000000000000, -0.000000000000000000, -1.000000000000000000 ) ) ;
#9263 = DIRECTION ( 'NONE',  ( 0.000000000000000000, 0.000000000000000000, 1.000000000000000000 ) ) ;
#9264 = DIRECTION ( 'NONE',  ( -0.000000000000000000, -0.000000000000000000, 1.000000000000000000 ) ) ;
#9265 = EDGE_CURVE ( 'NONE', #2172, #15620, #1552, .T. ) ;
#9266 = EDGE_CURVE ( 'NONE', #22867, #16872, #13230, .T. ) ;
#9267 = DIRECTION ( 'NONE',  ( 0.000000000000000000, 0.000000000000000000, 1.000000000000000000 ) ) ;
#9268 = CARTESIAN_POINT ( 'NONE',  ( 79.99999662536832545, -17.32050807568879591, 12.50000000000000000 ) ) ;
#9269 = AXIS2_PLACEMENT_3D ( 'NONE', #3131, #20378, #29179 ) ;
#9270 = DIRECTION ( 'NONE',  ( 1.000000000000000000, 0.000000000000000000, 0.000000000000000000 ) ) ;
#9271 = EDGE_LOOP ( 'NONE', ( #32796, #1010 ) ) ;
#9273 = VECTOR ( 'NONE', #25621, 1000.000000000000000 ) ;
#9272 = FACE_OUTER_BOUND ( 'NONE', #36067, .T. ) ;
#9274 = CARTESIAN_POINT ( 'NONE',  ( -65.00000000000000000, 0.000000000000000000, -4.999999999999997335 ) ) ;
#9275 = CARTESIAN_POINT ( 'NONE',  ( 59.99999662536845335, 34.64101615137759893, -9.999999999999998224 ) ) ;
#9276 = ORIENTED_EDGE ( 'NONE', *, *, #13251, .F. ) ;
#9278 = ORIENTED_EDGE ( 'NONE', *, *, #12739, .T. ) ;
#9277 = ADVANCED_FACE ( 'NONE', ( #33095 ), #27279, .F. ) ;
#9279 = ORIENTED_EDGE ( 'NONE', *, *, #15092, .T. ) ;
#9280 = CARTESIAN_POINT ( 'NONE',  ( 4.654160418576254177E-15, -6.066067634115602125, -4.359491423763670603 ) ) ;
#9281 = B_SPLINE_CURVE_WITH_KNOTS ( 'NONE', 3,
 ( #31092, #30344, #22658, #30889, #4681, #11206, #27543, #16664 ),
 .UNSPECIFIED., .F., .F.,
 ( 4, 2, 2, 4 ),
 ( 0.002921158011986722466, 0.003648658599403074854, 0.004376159186819426374, 0.005831160361652130281 ),
 .UNSPECIFIED. ) ;
#9282 = CARTESIAN_POINT ( 'NONE',  ( 0.000000000000000000, -55.00000000000000000, -5.000000000000000000 ) ) ;
#9283 = CARTESIAN_POINT ( 'NONE',  ( 52.99999662536846046, -43.30127018922200222, -9.999999999999998224 ) ) ;
#9284 = AXIS2_PLACEMENT_3D ( 'NONE', #29674, #14520, #34781 ) ;
#9285 = LINE ( 'NONE', #16866, #8480 ) ;
#9286 = DIRECTION ( 'NONE',  ( 0.000000000000000000, 0.000000000000000000, 1.000000000000000000 ) ) ;
#9287 = ORIENTED_EDGE ( 'NONE', *, *, #30744, .F. ) ;
#9288 = EDGE_CURVE ( 'NONE', #21337, #14745, #2146, .T. ) ;
#9289 = CYLINDRICAL_SURFACE ( 'NONE', #11373, 2.000000000000001776 ) ;
#9290 = ORIENTED_EDGE ( 'NONE', *, *, #4436, .F. ) ;
#9291 = FACE_BOUND ( 'NONE', #25342, .T. ) ;
#9292 = CYLINDRICAL_SURFACE ( 'NONE', #17939, 2.000000000000001776 ) ;
#9293 = VECTOR ( 'NONE', #5537, 1000.000000000000000 ) ;
#9294 = DIRECTION ( 'NONE',  ( 1.000000000000000000, 0.000000000000000000, 0.000000000000000000 ) ) ;
#9295 = CIRCLE ( 'NONE', #3332, 2.000000000000001776 ) ;
#9296 = EDGE_LOOP ( 'NONE', ( #8283, #3282 ) ) ;
#9297 = CARTESIAN_POINT ( 'NONE',  ( 65.00000000000000000, 7.960204194457797252E-15, 17.49999999999999645 ) ) ;
#9298 = DIRECTION ( 'NONE',  ( 0.3123845849830090282, 0.9499557205812244609, 0.000000000000000000 ) ) ;
#9299 = AXIS2_PLACEMENT_3D ( 'NONE', #36529, #13262, #25438 ) ;
#9300 = AXIS2_PLACEMENT_3D ( 'NONE', #11376, #22634, #19823 ) ;
#9301 = DIRECTION ( 'NONE',  ( 0.000000000000000000, 0.000000000000000000, 1.000000000000000000 ) ) ;
#9302 = CYLINDRICAL_SURFACE ( 'NONE', #20355, 2.000000000000001776 ) ;
#9303 = DIRECTION ( 'NONE',  ( 1.000000000000000000, 0.000000000000000000, 0.000000000000000000 ) ) ;
#9304 = ADVANCED_FACE ( 'NONE', ( #7796 ), #81, .T. ) ;
#9305 = EDGE_LOOP ( 'NONE', ( #25086, #32776, #28388, #26047 ) ) ;
#9306 = PLANE ( 'NONE',  #21481 ) ;
#9307 = DIRECTION ( 'NONE',  ( 0.000000000000000000, 0.000000000000000000, 1.000000000000000000 ) ) ;
#9308 = DIRECTION ( 'NONE',  ( 0.000000000000000000, 0.000000000000000000, 1.000000000000000000 ) ) ;
#9309 = EDGE_CURVE ( 'NONE', #6244, #31374, #27887, .T. ) ;
#9310 = AXIS2_PLACEMENT_3D ( 'NONE', #6462, #5919, #17351 ) ;
#9311 = VECTOR ( 'NONE', #6880, 1000.000000000000000 ) ;
#9312 = ORIENTED_EDGE ( 'NONE', *, *, #26552, .F. ) ;
#9313 = ORIENTED_EDGE ( 'NONE', *, *, #33435, .T. ) ;
#9314 = EDGE_LOOP ( 'NONE', ( #8304, #13299, #22943, #30322, #26776, #2657 ) ) ;
#9315 = EDGE_CURVE ( 'NONE', #8449, #4001, #20712, .T. ) ;
#9316 = CARTESIAN_POINT ( 'NONE',  ( 16.49657687835809128, -93.55673653615983199, 12.49999999999999822 ) ) ;
#9317 = CARTESIAN_POINT ( 'NONE',  ( 44.99999662536849598, -77.94228634059960825, -9.999999999999998224 ) ) ;
#9318 = CARTESIAN_POINT ( 'NONE',  ( 7.122621931239992550E-13, 68.00000000000000000, -4.999999999999997335 ) ) ;
#9319 = ADVANCED_FACE ( 'NONE', ( #34229 ), #8523, .F. ) ;
#9320 = DIRECTION ( 'NONE',  ( 0.000000000000000000, 0.000000000000000000, 1.000000000000000000 ) ) ;
#9321 = DIRECTION ( 'NONE',  ( 0.000000000000000000, 0.000000000000000000, -1.000000000000000000 ) ) ;
#9322 = AXIS2_PLACEMENT_3D ( 'NONE', #1727, #10339, #2636 ) ;
#9323 = CIRCLE ( 'NONE', #23715, 1.999999999999998224 ) ;
#9324 = CARTESIAN_POINT ( 'NONE',  ( -67.30619744049063513, -84.18124734178186941, 32.50000000000000000 ) ) ;
#9325 = VECTOR ( 'NONE', #24108, 1000.000000000000000 ) ;
#9326 = VERTEX_POINT ( 'NONE', #19405 ) ;
#9327 = CIRCLE ( 'NONE', #35091, 2.000000000000001776 ) ;
#9328 = ORIENTED_EDGE ( 'NONE', *, *, #32739, .F. ) ;
#9329 = CYLINDRICAL_SURFACE ( 'NONE', #21271, 1.999999999999998224 ) ;
#9330 = CIRCLE ( 'NONE', #7551, 2.000000000000001776 ) ;
#9331 = CARTESIAN_POINT ( 'NONE',  ( 0.000000000000000000, 0.000000000000000000, -6.000000000000000000 ) ) ;
#9332 = VERTEX_POINT ( 'NONE', #27829 ) ;
#9333 = CARTESIAN_POINT ( 'NONE',  ( 74.99999662536836809, 25.98076211353319565, -5.000000000000000000 ) ) ;
#9334 = ORIENTED_EDGE ( 'NONE', *, *, #19829, .F. ) ;
#9335 = AXIS2_PLACEMENT_3D ( 'NONE', #9487, #15097, #26526 ) ;
#9336 = CIRCLE ( 'NONE', #19526, 3.000000000000000888 ) ;
#9337 = EDGE_CURVE ( 'NONE', #22341, #28072, #17745, .T. ) ;
#9338 = FACE_BOUND ( 'NONE', #11328, .T. ) ;
#9339 = ORIENTED_EDGE ( 'NONE', *, *, #32051, .F. ) ;
#9340 = ORIENTED_EDGE ( 'NONE', *, *, #14181, .F. ) ;
#9341 = DIRECTION ( 'NONE',  ( 1.000000000000000000, 0.000000000000000000, 0.000000000000000000 ) ) ;
#9342 = VERTEX_POINT ( 'NONE', #28213 ) ;
#9343 =( NAMED_UNIT ( * ) PLANE_ANGLE_UNIT ( ) SI_UNIT ( $, .RADIAN. ) );
#9344 = AXIS2_PLACEMENT_3D ( 'NONE', #22409, #5722, #7982 ) ;
#9345 = ADVANCED_FACE ( 'NONE', ( #25594 ), #10793, .F. ) ;
#9346 = FACE_OUTER_BOUND ( 'NONE', #15798, .T. ) ;
#9347 = DIRECTION ( 'NONE',  ( 0.000000000000000000, 0.000000000000000000, 1.000000000000000000 ) ) ;
#9348 = CARTESIAN_POINT ( 'NONE',  ( 0.000000000000000000, 0.000000000000000000, 12.49999999999999822 ) ) ;
#9349 = EDGE_CURVE ( 'NONE', #27267, #10069, #30651, .T. ) ;
#9350 = EDGE_LOOP ( 'NONE', ( #12440, #32328 ) ) ;
#9351 = ORIENTED_EDGE ( 'NONE', *, *, #268, .T. ) ;
#9352 = COLOUR_RGB ( '', 0.40784314, 0.44705882, 0.49803922) ;
#9353 = AXIS2_PLACEMENT_3D ( 'NONE', #5354, #22944, #33655 ) ;
#9354 = AXIS2_PLACEMENT_3D ( 'NONE', #32496, #16012, #12436 ) ;
#9355 = ORIENTED_EDGE ( 'NONE', *, *, #30818, .T. ) ;
#9356 = AXIS2_PLACEMENT_3D ( 'NONE', #29820, #1142, #12932 ) ;
#9357 = CONICAL_SURFACE ( 'NONE', #3987, 2.445500000000000007, 0.7853981633974616017 ) ;
#9358 = ORIENTED_EDGE ( 'NONE', *, *, #31702, .T. ) ;
#9359 = CIRCLE ( 'NONE', #5758, 2.000000000000001776 ) ;
#9360 = ORIENTED_EDGE ( 'NONE', *, *, #36399, .T. ) ;
#9361 = CARTESIAN_POINT ( 'NONE',  ( 82.99999662536832545, 8.660254037844394404, -9.999999999999998224 ) ) ;
#9362 = DIRECTION ( 'NONE',  ( 0.000000000000000000, 0.000000000000000000, 1.000000000000000000 ) ) ;
#9363 = ORIENTED_EDGE ( 'NONE', *, *, #34907, .T. ) ;
#9364 = DIRECTION ( 'NONE',  ( 0.000000000000000000, 0.000000000000000000, 1.000000000000000000 ) ) ;
#9365 = FACE_OUTER_BOUND ( 'NONE', #8782, .T. ) ;
#9366 = CARTESIAN_POINT ( 'NONE',  ( 40.99999999999999289, -103.4105893997321743, 32.50000000000000000 ) ) ;
#9367 = EDGE_LOOP ( 'NONE', ( #31206, #11260, #27309, #12425 ) ) ;
#9368 = LINE ( 'NONE', #17273, #12848 ) ;
#9369 = AXIS2_PLACEMENT_3D ( 'NONE', #34776, #20491, #11681 ) ;
#9370 = DIRECTION ( 'NONE',  ( 1.000000000000000000, 0.000000000000000000, 0.000000000000000000 ) ) ;
#9371 = EDGE_CURVE ( 'NONE', #10781, #5113, #8783, .T. ) ;
#9372 = DIRECTION ( 'NONE',  ( 1.000000000000000000, 0.000000000000000000, 0.000000000000000000 ) ) ;
#9373 = ORIENTED_EDGE ( 'NONE', *, *, #19394, .T. ) ;
#9374 = DIRECTION ( 'NONE',  ( 0.000000000000000000, 0.000000000000000000, 1.000000000000000000 ) ) ;
#9375 = DIRECTION ( 'NONE',  ( 0.000000000000000000, 0.000000000000000000, 1.000000000000000000 ) ) ;
#9376 = ORIENTED_EDGE ( 'NONE', *, *, #10337, .F. ) ;
#9377 = ORIENTED_EDGE ( 'NONE', *, *, #17465, .F. ) ;
#9378 = CARTESIAN_POINT ( 'NONE',  ( -3.750000000000001776, 4.592425496802576930E-16, 13.31572692736085095 ) ) ;
#9379 = CIRCLE ( 'NONE', #20748, 33.00000000000001421 ) ;
#9380 = DIRECTION ( 'NONE',  ( 0.000000000000000000, 0.000000000000000000, 1.000000000000000000 ) ) ;
#9381 = CARTESIAN_POINT ( 'NONE',  ( 64.99999662536841072, -25.98076211353320275, -9.999999999999998224 ) ) ;
#9382 = CARTESIAN_POINT ( 'NONE',  ( -4.999999999999999112, 0.5616961504262225624, -0.5576671450146215570 ) ) ;
#9383 = AXIS2_PLACEMENT_3D ( 'NONE', #34097, #36706, #122 ) ;
#9384 = ORIENTED_EDGE ( 'NONE', *, *, #1147, .F. ) ;
#9385 = VECTOR ( 'NONE', #8550, 1000.000000000000000 ) ;
#9386 = CARTESIAN_POINT ( 'NONE',  ( -5.000000000000000000, 0.9888715124523126399, -0.07061148569344741222 ) ) ;
#9387 = CARTESIAN_POINT ( 'NONE',  ( -60.00000337463108480, -51.96152422706641971, 12.50000000000000000 ) ) ;
#9388 = AXIS2_PLACEMENT_3D ( 'NONE', #7987, #30305, #5180 ) ;
#9389 = EDGE_CURVE ( 'NONE', #26415, #21303, #19598, .T. ) ;
#9390 = ORIENTED_EDGE ( 'NONE', *, *, #13295, .T. ) ;
#9391 = EDGE_CURVE ( 'NONE', #7069, #30820, #26128, .T. ) ;
#9392 = LINE ( 'NONE', #3209, #6397 ) ;
#9393 = EDGE_LOOP ( 'NONE', ( #14648, #16085 ) ) ;
#9394 = CARTESIAN_POINT ( 'NONE',  ( -3.374631334790434423E-06, 69.28203230275516944, 12.50000000000000000 ) ) ;
#9395 = AXIS2_PLACEMENT_3D ( 'NONE', #21751, #29623, #32833 ) ;
#9396 = EDGE_CURVE ( 'NONE', #23264, #15061, #31029, .T. ) ;
#9397 = DIRECTION ( 'NONE',  ( 1.000000000000000000, 0.000000000000000000, 0.000000000000000000 ) ) ;
#9398 = CYLINDRICAL_SURFACE ( 'NONE', #32193, 2.000000000000001776 ) ;
#9399 = ORIENTED_EDGE ( 'NONE', *, *, #28684, .F. ) ;
#9400 = VERTEX_POINT ( 'NONE', #13790 ) ;
#9401 = ADVANCED_FACE ( 'NONE', ( #2705 ), #16795, .F. ) ;
#9402 = CIRCLE ( 'NONE', #35177, 2.000000000000000000 ) ;
#9403 = EDGE_CURVE ( 'NONE', #24339, #22350, #7586, .T. ) ;
#9404 = CIRCLE ( 'NONE', #7628, 2.000000000000001776 ) ;
#9405 = CARTESIAN_POINT ( 'NONE',  ( 35.19434990244975126, -52.39915983220758022, 12.49999999999999822 ) ) ;
#9406 = CARTESIAN_POINT ( 'NONE',  ( 0.000000000000000000, 0.000000000000000000, 5.000000000000000000 ) ) ;
#9407 = AXIS2_PLACEMENT_3D ( 'NONE', #28748, #25935, #5347 ) ;
#9408 = ORIENTED_EDGE ( 'NONE', *, *, #32810, .F. ) ;
#9409 = DIRECTION ( 'NONE',  ( -1.000000000000000000, 0.000000000000000000, 0.000000000000000000 ) ) ;
#9410 = CARTESIAN_POINT ( 'NONE',  ( -3.374631303565411855E-06, -86.60254037844400443, 17.49999999999999645 ) ) ;
#9411 = SURFACE_STYLE_FILL_AREA ( #28479 ) ;
#9412 = DIRECTION ( 'NONE',  ( 0.000000000000000000, 0.000000000000000000, -1.000000000000000000 ) ) ;
#9413 = CARTESIAN_POINT ( 'NONE',  ( 4.999999999999999112, 2.886751345948125991, -3.984345921091767551 ) ) ;
#9414 = DIRECTION ( 'NONE',  ( 0.000000000000000000, 0.000000000000000000, 1.000000000000000000 ) ) ;
#9415 = ADVANCED_FACE ( 'NONE', ( #30823 ), #5160, .F. ) ;
#9416 = AXIS2_PLACEMENT_3D ( 'NONE', #8527, #14142, #25602 ) ;
#9417 = ORIENTED_EDGE ( 'NONE', *, *, #27127, .T. ) ;
#9418 = DIRECTION ( 'NONE',  ( 0.000000000000000000, 0.000000000000000000, 1.000000000000000000 ) ) ;
#9419 = AXIS2_PLACEMENT_3D ( 'NONE', #31108, #2041, #33570 ) ;
#9420 = EDGE_CURVE ( 'NONE', #14513, #27693, #12949, .T. ) ;
#9421 = CIRCLE ( 'NONE', #17190, 2.000000000000001776 ) ;
#9422 = CARTESIAN_POINT ( 'NONE',  ( -43.00000337463112743, -60.62177826491080168, -9.999999999999998224 ) ) ;
#9423 = EDGE_CURVE ( 'NONE', #25244, #5952, #2798, .T. ) ;
#9424 = DIRECTION ( 'NONE',  ( -1.000000000000000000, 0.000000000000000000, 0.000000000000000000 ) ) ;
#9425 = VERTEX_POINT ( 'NONE', #17342 ) ;
#9426 = EDGE_CURVE ( 'NONE', #19493, #31662, #442, .T. ) ;
#9427 = CARTESIAN_POINT ( 'NONE',  ( 71.99999662536839651, -3.469446951953614189E-15, -9.999999999999998224 ) ) ;
#9428 = LINE ( 'NONE', #23489, #27320 ) ;
#9429 = DIRECTION ( 'NONE',  ( 0.5000000000000039968, 0.8660254037844363761, 0.000000000000000000 ) ) ;
#9430 = AXIS2_PLACEMENT_3D ( 'NONE', #24871, #25246, #36674 ) ;
#9431 = ORIENTED_EDGE ( 'NONE', *, *, #855, .T. ) ;
#9432 = EDGE_LOOP ( 'NONE', ( #1280, #24860, #5321, #33944, #7824 ) ) ;
#9433 = EDGE_LOOP ( 'NONE', ( #492, #13691, #35973, #6794 ) ) ;
#9434 = AXIS2_PLACEMENT_3D ( 'NONE', #8689, #26126, #22783 ) ;
#9435 = LINE ( 'NONE', #26317, #35216 ) ;
#9436 = CARTESIAN_POINT ( 'NONE',  ( -80.00000337463094979, 17.32050807568878525, -9.999999999999998224 ) ) ;
#9437 = LINE ( 'NONE', #21049, #22018 ) ;
#9438 = EDGE_LOOP ( 'NONE', ( #9543, #33120, #7711, #16413 ) ) ;
#9439 = EDGE_LOOP ( 'NONE', ( #10166, #19060 ) ) ;
#9440 = CIRCLE ( 'NONE', #20224, 27.00000000000001066 ) ;
#9441 = CIRCLE ( 'NONE', #32171, 2.000000000000001776 ) ;
#9442 = ORIENTED_EDGE ( 'NONE', *, *, #32948, .T. ) ;
#9443 = AXIS2_PLACEMENT_3D ( 'NONE', #11643, #5869, #2669 ) ;
#9444 = DIRECTION ( 'NONE',  ( 1.000000000000000000, 0.000000000000000000, 0.000000000000000000 ) ) ;
#9445 = EDGE_CURVE ( 'NONE', #36367, #36578, #6994, .T. ) ;
#9446 = AXIS2_PLACEMENT_3D ( 'NONE', #18427, #26112, #422 ) ;
#9447 = EDGE_LOOP ( 'NONE', ( #9555, #20038, #11595, #31111 ) ) ;
#9448 = CARTESIAN_POINT ( 'NONE',  ( -10.00000337463128730, 69.28203230275516944, -9.999999999999998224 ) ) ;
#9449 = ORIENTED_EDGE ( 'NONE', *, *, #24022, .F. ) ;
#9450 = CARTESIAN_POINT ( 'NONE',  ( -36.97203788308986105, 58.48108235278859013, 12.49999999999999645 ) ) ;
#9451 = ORIENTED_EDGE ( 'NONE', *, *, #9878, .F. ) ;
#9452 = ORIENTED_EDGE ( 'NONE', *, *, #17058, .F. ) ;
#9453 = AXIS2_PLACEMENT_3D ( 'NONE', #24100, #27268, #22033 ) ;
#9454 = AXIS2_PLACEMENT_3D ( 'NONE', #15248, #1199, #18066 ) ;
#9455 = DIRECTION ( 'NONE',  ( -0.000000000000000000, -0.000000000000000000, -1.000000000000000000 ) ) ;
#9456 = CARTESIAN_POINT ( 'NONE',  ( 3.675296855064185575, -3.651569063273171434, -0.8655517945778166133 ) ) ;
#9457 = DIRECTION ( 'NONE',  ( 1.000000000000000000, 0.000000000000000000, 0.000000000000000000 ) ) ;
#9458 = VERTEX_POINT ( 'NONE', #6079 ) ;
#9459 = EDGE_LOOP ( 'NONE', ( #12655, #4098, #29470, #17836 ) ) ;
#9460 = EDGE_CURVE ( 'NONE', #20372, #7276, #32315, .T. ) ;
#9461 = CYLINDRICAL_SURFACE ( 'NONE', #7732, 3.000000000000002665 ) ;
#9462 = AXIS2_PLACEMENT_3D ( 'NONE', #37053, #28597, #8174 ) ;
#9463 = CARTESIAN_POINT ( 'NONE',  ( -31.46585318596190106, -86.45172111230344569, -4.999999999999997335 ) ) ;
#9464 = DIRECTION ( 'NONE',  ( 0.000000000000000000, 0.000000000000000000, 1.000000000000000000 ) ) ;
#9465 = CARTESIAN_POINT ( 'NONE',  ( -80.00000337463096400, -34.64101615137762025, 12.50000000000000000 ) ) ;
#9466 = EDGE_LOOP ( 'NONE', ( #29547, #14807 ) ) ;
#9467 = FACE_OUTER_BOUND ( 'NONE', #29019, .T. ) ;
#9469 = AXIS2_PLACEMENT_3D ( 'NONE', #20291, #26457, #26093 ) ;
#9468 = CARTESIAN_POINT ( 'NONE',  ( -2.775557561562891351E-14, 19.94802294027085310, -19.99999999999999645 ) ) ;
#9470 = EDGE_LOOP ( 'NONE', ( #4369, #11788, #31532, #32674, #15160, #16126 ) ) ;
#9471 = FACE_OUTER_BOUND ( 'NONE', #23439, .T. ) ;
#9472 = AXIS2_PLACEMENT_3D ( 'NONE', #26918, #32153, #1233 ) ;
#9473 = AXIS2_PLACEMENT_3D ( 'NONE', #4345, #18206, #26851 ) ;
#9474 = DIRECTION ( 'NONE',  ( 0.000000000000000000, 0.000000000000000000, 1.000000000000000000 ) ) ;
#9475 = CARTESIAN_POINT ( 'NONE',  ( -65.00000337463102085, 60.62177826491077326, -9.999999999999998224 ) ) ;
#9477 = CIRCLE ( 'NONE', #17837, 95.00000000000001421 ) ;
#9476 = DIRECTION ( 'NONE',  ( -1.000000000000000000, 0.000000000000000000, 0.000000000000000000 ) ) ;
#9478 = EDGE_CURVE ( 'NONE', #2491, #10475, #22543, .T. ) ;
#9479 = FACE_OUTER_BOUND ( 'NONE', #23212, .T. ) ;
#9480 = VECTOR ( 'NONE', #14276, 999.9999999999998863 ) ;
#9481 = EDGE_CURVE ( 'NONE', #4400, #5554, #36345, .T. ) ;
#9482 = ADVANCED_FACE ( 'NONE', ( #8698 ), #6251, .T. ) ;
#9483 = DIRECTION ( 'NONE',  ( -1.000000000000000000, 0.000000000000000000, 0.000000000000000000 ) ) ;
#9484 = VERTEX_POINT ( 'NONE', #9450 ) ;
#9485 = DIRECTION ( 'NONE',  ( -1.000000000000000000, 0.000000000000000000, 0.000000000000000000 ) ) ;
#9486 = DIRECTION ( 'NONE',  ( -1.000000000000000000, 0.000000000000000000, 0.000000000000000000 ) ) ;
#9487 = CARTESIAN_POINT ( 'NONE',  ( 108.3061974404898820, 19.22934205794938478, 27.50000000000000000 ) ) ;
#9488 = ORIENTED_EDGE ( 'NONE', *, *, #2306, .F. ) ;
#9489 = ORIENTED_EDGE ( 'NONE', *, *, #12289, .F. ) ;
#9490 = EDGE_LOOP ( 'NONE', ( #2955, #24895, #14011, #15026 ) ) ;
#9491 = DIRECTION ( 'NONE',  ( 0.000000000000000000, 0.000000000000000000, 1.000000000000000000 ) ) ;
#9492 = DIRECTION ( 'NONE',  ( 3.469446951953612611E-15, 1.000000000000000000, 0.000000000000000000 ) ) ;
#9493 = AXIS2_PLACEMENT_3D ( 'NONE', #127, #23010, #7858 ) ;
#9494 = CARTESIAN_POINT ( 'NONE',  ( -5.000000000000000888, 0.9828435001097632906, -5.956909652965543422 ) ) ;
#9495 = VECTOR ( 'NONE', #8070, 1000.000000000000000 ) ;
#9496 = CARTESIAN_POINT ( 'NONE',  ( -37.50000000000000000, 103.4105893997321886, -19.99999999999999645 ) ) ;
#9497 = ORIENTED_EDGE ( 'NONE', *, *, #30847, .T. ) ;
#9498 = DIRECTION ( 'NONE',  ( 0.000000000000000000, 0.000000000000000000, 1.000000000000000000 ) ) ;
#9499 = ORIENTED_EDGE ( 'NONE', *, *, #34088, .T. ) ;
#9500 = FACE_BOUND ( 'NONE', #25874, .T. ) ;
#9501 = EDGE_CURVE ( 'NONE', #8706, #17922, #35725, .T. ) ;
#9502 = AXIS2_PLACEMENT_3D ( 'NONE', #26517, #14909, #32132 ) ;
#9503 = AXIS2_PLACEMENT_3D ( 'NONE', #36731, #33568, #19307 ) ;
#9504 = DIRECTION ( 'NONE',  ( 1.000000000000000000, 0.000000000000000000, 0.000000000000000000 ) ) ;
#9505 = DIRECTION ( 'NONE',  ( 0.000000000000000000, 0.000000000000000000, 1.000000000000000000 ) ) ;
#9506 = VERTEX_POINT ( 'NONE', #26133 ) ;
#9507 = CARTESIAN_POINT ( 'NONE',  ( -12.00000337463125000, -86.60254037844400443, -9.999999999999998224 ) ) ;
#9508 = CARTESIAN_POINT ( 'NONE',  ( -45.00000337463111322, 77.94228634059959404, -5.000000000000000000 ) ) ;
#9509 = AXIS2_PLACEMENT_3D ( 'NONE', #22553, #28735, #19920 ) ;
#9510 = CARTESIAN_POINT ( 'NONE',  ( -55.00000337463109901, -60.62177826491083010, -9.999999999999998224 ) ) ;
#9511 = DIRECTION ( 'NONE',  ( 0.000000000000000000, 0.000000000000000000, 1.000000000000000000 ) ) ;
#9512 = EDGE_LOOP ( 'NONE', ( #17565, #25951, #8888, #13741 ) ) ;
#9513 = DIRECTION ( 'NONE',  ( 0.000000000000000000, 0.000000000000000000, 1.000000000000000000 ) ) ;
#9514 = DIRECTION ( 'NONE',  ( 0.000000000000000000, 0.000000000000000000, 1.000000000000000000 ) ) ;
#9515 = LINE ( 'NONE', #1620, #15988 ) ;
#9516 = ORIENTED_EDGE ( 'NONE', *, *, #7506, .F. ) ;
#9517 = EDGE_LOOP ( 'NONE', ( #26742, #20297, #20612, #15849 ) ) ;
#9518 = CIRCLE ( 'NONE', #30473, 2.000000000000000000 ) ;
#9519 = EDGE_CURVE ( 'NONE', #8231, #20602, #2205, .T. ) ;
#9520 = ORIENTED_EDGE ( 'NONE', *, *, #21087, .F. ) ;
#9521 = AXIS2_PLACEMENT_3D ( 'NONE', #7563, #15812, #7378 ) ;
#9522 = DIRECTION ( 'NONE',  ( -0.000000000000000000, -0.000000000000000000, -1.000000000000000000 ) ) ;
#9523 = DIRECTION ( 'NONE',  ( 0.000000000000000000, 0.000000000000000000, 1.000000000000000000 ) ) ;
#9524 = DIRECTION ( 'NONE',  ( 0.000000000000000000, 0.000000000000000000, 1.000000000000000000 ) ) ;
#9525 = VECTOR ( 'NONE', #28570, 1000.000000000000000 ) ;
#9526 = DIRECTION ( 'NONE',  ( 1.000000000000000000, 0.000000000000000000, 0.000000000000000000 ) ) ;
#9527 = DIRECTION ( 'NONE',  ( -1.000000000000000000, -1.776356839400250465E-15, 0.000000000000000000 ) ) ;
#9529 = DIRECTION ( 'NONE',  ( 1.000000000000000000, 0.000000000000000000, 0.000000000000000000 ) ) ;
#9528 = VECTOR ( 'NONE', #18942, 1000.000000000000000 ) ;
#9530 = VERTEX_POINT ( 'NONE', #6448 ) ;
#9531 = ORIENTED_EDGE ( 'NONE', *, *, #26797, .F. ) ;
#9532 = DIRECTION ( 'NONE',  ( 0.000000000000000000, 0.000000000000000000, 1.000000000000000000 ) ) ;
#9533 = AXIS2_PLACEMENT_3D ( 'NONE', #3129, #22646, #8209 ) ;
#9534 = CARTESIAN_POINT ( 'NONE',  ( 62.97617850287784336, 4.279621169095339184, 12.49999999999999822 ) ) ;
#9535 = EDGE_LOOP ( 'NONE', ( #14279, #18641, #16516, #2473 ) ) ;
#9536 = AXIS2_PLACEMENT_3D ( 'NONE', #21082, #18836, #16217 ) ;
#9537 = DIRECTION ( 'NONE',  ( 0.000000000000000000, 0.000000000000000000, -1.000000000000000000 ) ) ;
#9538 = ORIENTED_EDGE ( 'NONE', *, *, #35957, .F. ) ;
#9539 = EDGE_CURVE ( 'NONE', #10452, #23651, #29316, .T. ) ;
#9540 = FACE_BOUND ( 'NONE', #26596, .T. ) ;
#9541 = VECTOR ( 'NONE', #15506, 1000.000000000000000 ) ;
#9542 = VERTEX_POINT ( 'NONE', #11875 ) ;
#9543 = ORIENTED_EDGE ( 'NONE', *, *, #26689, .F. ) ;
#9544 = AXIS2_PLACEMENT_3D ( 'NONE', #6908, #35434, #904 ) ;
#9545 = DIRECTION ( 'NONE',  ( 1.000000000000000000, 0.000000000000000000, 0.000000000000000000 ) ) ;
#9546 = ORIENTED_EDGE ( 'NONE', *, *, #23821, .T. ) ;
#9547 = LINE ( 'NONE', #29408, #26628 ) ;
#9548 = ADVANCED_FACE ( 'NONE', ( #25952 ), #808, .F. ) ;
#9549 = CARTESIAN_POINT ( 'NONE',  ( 0.000000000000000000, 0.000000000000000000, -25.03750572909317285 ) ) ;
#9550 = CARTESIAN_POINT ( 'NONE',  ( -30.00000337463119848, -69.28203230275522628, 17.49999999999999645 ) ) ;
#9551 = ORIENTED_EDGE ( 'NONE', *, *, #35104, .T. ) ;
#9552 = VERTEX_POINT ( 'NONE', #20882 ) ;
#9553 = CIRCLE ( 'NONE', #34696, 2.000000000000001776 ) ;
#9554 = ORIENTED_EDGE ( 'NONE', *, *, #25927, .T. ) ;
#9555 = ORIENTED_EDGE ( 'NONE', *, *, #12389, .F. ) ;
#9556 = AXIS2_PLACEMENT_3D ( 'NONE', #1416, #35747, #4619 ) ;
#9557 = ORIENTED_EDGE ( 'NONE', *, *, #8140, .T. ) ;
#9558 = DIRECTION ( 'NONE',  ( 1.000000000000000000, 0.000000000000000000, 0.000000000000000000 ) ) ;
#9559 = ADVANCED_FACE ( 'NONE', ( #23336 ), #20678, .F. ) ;
#9560 = DIRECTION ( 'NONE',  ( 1.000000000000000000, 0.000000000000000000, 0.000000000000000000 ) ) ;
#9561 = ORIENTED_EDGE ( 'NONE', *, *, #9309, .T. ) ;
#9562 = CARTESIAN_POINT ( 'NONE',  ( -10.00000337463128730, 69.28203230275516944, -5.000000000000000000 ) ) ;
#9563 = CARTESIAN_POINT ( 'NONE',  ( 101.0514726702494386, 64.20674970622599176, 32.50000000000001421 ) ) ;
#9564 = AXIS2_PLACEMENT_3D ( 'NONE', #9410, #20846, #33961 ) ;
#9565 = CARTESIAN_POINT ( 'NONE',  ( -85.00000337463092137, 8.660254037844389075, -5.000000000000000000 ) ) ;
#9566 = EDGE_LOOP ( 'NONE', ( #35339, #1201 ) ) ;
#9567 = DIRECTION ( 'NONE',  ( 1.000000000000000000, 0.000000000000000000, 0.000000000000000000 ) ) ;
#9568 = CARTESIAN_POINT ( 'NONE',  ( -22.00000337463122690, 86.60254037844397601, -9.999999999999998224 ) ) ;
#9569 = VECTOR ( 'NONE', #8714, 1000.000000000000000 ) ;
#9570 = DIRECTION ( 'NONE',  ( 0.000000000000000000, 0.000000000000000000, 1.000000000000000000 ) ) ;
#9571 = ORIENTED_EDGE ( 'NONE', *, *, #14257, .T. ) ;
#9572 = CARTESIAN_POINT ( 'NONE',  ( -83.00000337463092137, 25.98076211353317433, -9.999999999999998224 ) ) ;
#9573 = AXIS2_PLACEMENT_3D ( 'NONE', #28811, #33717, #33900 ) ;
#9574 = CARTESIAN_POINT ( 'NONE',  ( 47.99999662536846756, -69.28203230275519786, -9.999999999999998224 ) ) ;
#9575 = ORIENTED_EDGE ( 'NONE', *, *, #21476, .T. ) ;
#9576 = EDGE_CURVE ( 'NONE', #30221, #32244, #18968, .T. ) ;
#9577 = EDGE_LOOP ( 'NONE', ( #31326, #2003, #8074, #15797 ) ) ;
#9578 = CARTESIAN_POINT ( 'NONE',  ( 3.000000000000000000, 1.467624384280024730, -2.542000000000001592 ) ) ;
#9579 = EDGE_CURVE ( 'NONE', #2310, #32307, #5183, .T. ) ;
#9580 = DIRECTION ( 'NONE',  ( -0.000000000000000000, -0.000000000000000000, 1.000000000000000000 ) ) ;
#9581 = CARTESIAN_POINT ( 'NONE',  ( 34.00000000000000000, 103.4105893997321743, 27.50000000000000000 ) ) ;
#9582 = DIRECTION ( 'NONE',  ( 0.000000000000000000, 0.000000000000000000, 1.000000000000000000 ) ) ;
#9583 = ORIENTED_EDGE ( 'NONE', *, *, #9680, .T. ) ;
#9584 = CIRCLE ( 'NONE', #16769, 2.000000000000001776 ) ;
#9585 = EDGE_CURVE ( 'NONE', #20938, #36052, #27332, .T. ) ;
#9586 = CARTESIAN_POINT ( 'NONE',  ( -5.000000000000000000, 0.2466074518009242766, -2.689117849295589213E-15 ) ) ;
#9587 = CARTESIAN_POINT ( 'NONE',  ( -47.00000337463111322, -77.94228634059960825, -5.000000000000000000 ) ) ;
#9588 = ORIENTED_EDGE ( 'NONE', *, *, #9951, .T. ) ;
#9589 = AXIS2_PLACEMENT_3D ( 'NONE', #23484, #23309, #31728 ) ;
#9590 = ADVANCED_FACE ( 'NONE', ( #3456 ), #14889, .F. ) ;
#9591 = DIRECTION ( 'NONE',  ( -1.000000000000000000, 0.000000000000000000, 0.000000000000000000 ) ) ;
#9592 = PRESENTATION_LAYER_ASSIGNMENT (  '', '', ( #19798 ) ) ;
#9593 = VERTEX_POINT ( 'NONE', #20330 ) ;
#9594 = CARTESIAN_POINT ( 'NONE',  ( 26.97173338359068850, -77.60724282659606388, -5.000000000000000000 ) ) ;
#9595 = LINE ( 'NONE', #23647, #34378 ) ;
#9596 = EDGE_CURVE ( 'NONE', #30141, #19642, #17175, .T. ) ;
#9597 = AXIS2_PLACEMENT_3D ( 'NONE', #3336, #887, #12305 ) ;
#9598 = DIRECTION ( 'NONE',  ( 0.000000000000000000, 0.000000000000000000, -1.000000000000000000 ) ) ;
#9599 = EDGE_LOOP ( 'NONE', ( #35243, #24708, #18766, #18733 ) ) ;
#9600 = ORIENTED_EDGE ( 'NONE', *, *, #19863, .T. ) ;
#9601 = AXIS2_PLACEMENT_3D ( 'NONE', #24124, #27293, #4258 ) ;
#9602 = LINE ( 'NONE', #34746, #18510 ) ;
#9603 = VERTEX_POINT ( 'NONE', #32486 ) ;
#9604 = CARTESIAN_POINT ( 'NONE',  ( 0.000000000000000000, 0.000000000000000000, -5.000000000000000000 ) ) ;
#9605 = DIRECTION ( 'NONE',  ( 0.000000000000000000, -0.000000000000000000, 1.000000000000000000 ) ) ;
#9606 = CIRCLE ( 'NONE', #27878, 3.500000000000003109 ) ;
#9607 = DIRECTION ( 'NONE',  ( 1.000000000000000000, 0.000000000000000000, 0.000000000000000000 ) ) ;
#9608 = DIRECTION ( 'NONE',  ( 1.000000000000000000, 0.000000000000000000, 0.000000000000000000 ) ) ;
#9609 = DIRECTION ( 'NONE',  ( -0.7071067811865411334, 0.7071067811865539010, 0.000000000000000000 ) ) ;
#9610 = VERTEX_POINT ( 'NONE', #21794 ) ;
#9611 = DIRECTION ( 'NONE',  ( 0.000000000000000000, 0.000000000000000000, 1.000000000000000000 ) ) ;
#9612 = EDGE_CURVE ( 'NONE', #26170, #12792, #21958, .T. ) ;
#9613 = CARTESIAN_POINT ( 'NONE',  ( -70.00000337463099243, -2.428612866367529932E-14, 17.49999999999999645 ) ) ;
#9614 = AXIS2_PLACEMENT_3D ( 'NONE', #30165, #35626, #29992 ) ;
#9615 = DIRECTION ( 'NONE',  ( 1.000000000000000000, 0.000000000000000000, 0.000000000000000000 ) ) ;
#9616 = ORIENTED_EDGE ( 'NONE', *, *, #36925, .T. ) ;
#9617 = LINE ( 'NONE', #18216, #16648 ) ;
#9618 = CARTESIAN_POINT ( 'NONE',  ( 22.99999662536859901, -77.94228634059960825, 17.49999999999999645 ) ) ;
#9619 = AXIS2_PLACEMENT_3D ( 'NONE', #7864, #1675, #2032 ) ;
#9620 = LINE ( 'NONE', #9224, #20976 ) ;
#9621 = ORIENTED_EDGE ( 'NONE', *, *, #35748, .F. ) ;
#9622 = ADVANCED_FACE ( 'NONE', ( #1924 ), #1196, .F. ) ;
#9623 = EDGE_LOOP ( 'NONE', ( #19320, #27549, #18897, #18229, #3289 ) ) ;
#9624 = EDGE_CURVE ( 'NONE', #32853, #20212, #8178, .T. ) ;
#9625 = CARTESIAN_POINT ( 'NONE',  ( -35.83991598322101169, -56.52018970185248037, -49.22241343995298024 ) ) ;
#9626 = CARTESIAN_POINT ( 'NONE',  ( -85.00000337463092137, -25.98076211353322051, -9.999999999999998224 ) ) ;
#9627 = EDGE_CURVE ( 'NONE', #745, #11213, #1548, .T. ) ;
#9628 = DIRECTION ( 'NONE',  ( 1.000000000000000000, 0.000000000000000000, 0.000000000000000000 ) ) ;
#9629 = ORIENTED_EDGE ( 'NONE', *, *, #7302, .F. ) ;
#9630 = EDGE_LOOP ( 'NONE', ( #32891, #31899 ) ) ;
#9631 = VERTEX_POINT ( 'NONE', #32673 ) ;
#9632 = CYLINDRICAL_SURFACE ( 'NONE', #29039, 2.000000000000001776 ) ;
#9633 = ORIENTED_EDGE ( 'NONE', *, *, #22923, .T. ) ;
#9634 = ORIENTED_EDGE ( 'NONE', *, *, #33516, .F. ) ;
#9635 = DIRECTION ( 'NONE',  ( 1.000000000000000000, 0.000000000000000000, 0.000000000000000000 ) ) ;
#9636 = ORIENTED_EDGE ( 'NONE', *, *, #21790, .T. ) ;
#9637 = EDGE_LOOP ( 'NONE', ( #28683, #16996, #12678, #28604 ) ) ;
#9638 = SURFACE_STYLE_FILL_AREA ( #29487 ) ;
#9639 = CARTESIAN_POINT ( 'NONE',  ( 31.27962116909600709, -62.97617850287780072, -49.86561046011506448 ) ) ;
#9640 = EDGE_CURVE ( 'NONE', #36079, #18409, #36918, .T. ) ;
#9641 = CARTESIAN_POINT ( 'NONE',  ( -86.45172111230354517, 31.46585318596159553, 12.49999999999999822 ) ) ;
#9642 = ORIENTED_EDGE ( 'NONE', *, *, #13544, .F. ) ;
#9643 = ORIENTED_EDGE ( 'NONE', *, *, #7859, .T. ) ;
#9644 = DIRECTION ( 'NONE',  ( 1.000000000000000000, 0.000000000000000000, 0.000000000000000000 ) ) ;
#9645 = CARTESIAN_POINT ( 'NONE',  ( 16.99999662536859901, 77.94228634059957983, 12.50000000000000000 ) ) ;
#9646 = DIRECTION ( 'NONE',  ( 1.000000000000000000, 0.000000000000000000, 0.000000000000000000 ) ) ;
#9647 = DIRECTION ( 'NONE',  ( 1.000000000000000000, 0.000000000000000000, 0.000000000000000000 ) ) ;
#9648 = ORIENTED_EDGE ( 'NONE', *, *, #2319, .F. ) ;
#9649 = DIRECTION ( 'NONE',  ( 0.5000000000000038858, 0.8660254037844362651, 0.000000000000000000 ) ) ;
#9650 = CARTESIAN_POINT ( 'NONE',  ( 0.000000000000000000, 92.82302294027094547, -29.97964607176044893 ) ) ;
#9651 = VERTEX_POINT ( 'NONE', #26882 ) ;
#9652 = CARTESIAN_POINT ( 'NONE',  ( 4.999996625368676284, -77.94228634059960825, 12.50000000000000000 ) ) ;
#9653 = PLANE ( 'NONE',  #5826 ) ;
#9654 = DIRECTION ( 'NONE',  ( -1.000000000000000000, 0.000000000000000000, 0.000000000000000000 ) ) ;
#9655 = DIRECTION ( 'NONE',  ( 1.000000000000000000, 0.000000000000000000, 0.000000000000000000 ) ) ;
#9656 = EDGE_CURVE ( 'NONE', #13843, #9593, #4600, .T. ) ;
#9657 = DIRECTION ( 'NONE',  ( 1.000000000000000000, 0.000000000000000000, 0.000000000000000000 ) ) ;
#9658 = DIRECTION ( 'NONE',  ( 1.000000000000000000, 0.000000000000000000, 0.000000000000000000 ) ) ;
#9659 = ORIENTED_EDGE ( 'NONE', *, *, #25883, .F. ) ;
#9660 = ADVANCED_FACE ( 'NONE', ( #24633 ), #6800, .F. ) ;
#9661 = PLANE ( 'NONE',  #11200 ) ;
#9662 = CIRCLE ( 'NONE', #28232, 1.999999999999998224 ) ;
#9663 = CARTESIAN_POINT ( 'NONE',  ( -108.3061974404900241, -19.22934205794863516, 32.50000000000000000 ) ) ;
#9664 = CARTESIAN_POINT ( 'NONE',  ( 36.99999662536855283, -60.62177826491080168, 17.49999999999999645 ) ) ;
#9665 = ORIENTED_EDGE ( 'NONE', *, *, #31119, .T. ) ;
#9666 = EDGE_CURVE ( 'NONE', #18360, #34031, #14165, .T. ) ;
#9667 = EDGE_LOOP ( 'NONE', ( #25694, #4186 ) ) ;
#9668 = VERTEX_POINT ( 'NONE', #24067 ) ;
#9669 = PLANE ( 'NONE',  #31380 ) ;
#9670 = DIRECTION ( 'NONE',  ( 0.000000000000000000, 0.000000000000000000, -1.000000000000000000 ) ) ;
#9671 = EDGE_CURVE ( 'NONE', #12740, #3455, #13185, .T. ) ;
#9672 = CARTESIAN_POINT ( 'NONE',  ( -27.78182860042817026, -56.67878100130359087, 12.49999999999999822 ) ) ;
#9673 = EDGE_CURVE ( 'NONE', #8255, #35883, #21627, .T. ) ;
#9674 = CARTESIAN_POINT ( 'NONE',  ( -5.000000000000000000, 2.886751345948137981, -5.553418012614792509 ) ) ;
#9675 = CARTESIAN_POINT ( 'NONE',  ( 19.99999662536861678, -86.60254037844400443, -5.000000000000000000 ) ) ;
#9676 = ORIENTED_EDGE ( 'NONE', *, *, #30500, .T. ) ;
#9677 = CARTESIAN_POINT ( 'NONE',  ( 56.99999662536844625, 43.30127018922198801, -9.999999999999998224 ) ) ;
#9678 = ORIENTED_EDGE ( 'NONE', *, *, #8192, .T. ) ;
#9679 = FACE_BOUND ( 'NONE', #1897, .T. ) ;
#9680 = EDGE_CURVE ( 'NONE', #2691, #14791, #36952, .T. ) ;
#9681 = EDGE_CURVE ( 'NONE', #1135, #3002, #33956, .T. ) ;
#9682 = CARTESIAN_POINT ( 'NONE',  ( -70.00000337463099243, 17.32050807568877460, 17.49999999999999645 ) ) ;
#9683 = LINE ( 'NONE', #35397, #12540 ) ;
#9684 = EDGE_CURVE ( 'NONE', #26423, #34827, #18236, .T. ) ;
#9685 = CIRCLE ( 'NONE', #8502, 2.000000000000001776 ) ;
#9686 = EDGE_CURVE ( 'NONE', #6350, #25578, #12374, .T. ) ;
#9687 = DIRECTION ( 'NONE',  ( 0.000000000000000000, 0.000000000000000000, 1.000000000000000000 ) ) ;
#9688 = ORIENTED_EDGE ( 'NONE', *, *, #13106, .F. ) ;
#9689 = CARTESIAN_POINT ( 'NONE',  ( 108.3061974404897825, -19.22934205795014151, 27.50000000000000000 ) ) ;
#9690 = AXIS2_PLACEMENT_3D ( 'NONE', #28876, #31698, #31861 ) ;
#9691 = CARTESIAN_POINT ( 'NONE',  ( 56.99999662536844625, -60.62177826491080168, -9.999999999999998224 ) ) ;
#9692 = CARTESIAN_POINT ( 'NONE',  ( 83.67710222720857871, -27.48074558388131905, 12.50000000000000000 ) ) ;
#9693 = DIRECTION ( 'NONE',  ( 1.000000000000000000, 0.000000000000000000, 0.000000000000000000 ) ) ;
#9694 = ORIENTED_EDGE ( 'NONE', *, *, #16503, .T. ) ;
#9695 = DIRECTION ( 'NONE',  ( 0.000000000000000000, 0.000000000000000000, 1.000000000000000000 ) ) ;
#9696 = CARTESIAN_POINT ( 'NONE',  ( 55.27226924886128501, 77.26562141134559170, 27.50000000000000000 ) ) ;
#9697 = DIRECTION ( 'NONE',  ( -0.000000000000000000, -0.000000000000000000, 1.000000000000000000 ) ) ;
#9698 = ORIENTED_EDGE ( 'NONE', *, *, #27109, .F. ) ;
#9699 = EDGE_LOOP ( 'NONE', ( #31458, #8073, #10912, #142 ) ) ;
#9700 = ORIENTED_EDGE ( 'NONE', *, *, #32932, .T. ) ;
#9701 = CARTESIAN_POINT ( 'NONE',  ( 5.999999999999998224, 0.000000000000000000, 0.000000000000000000 ) ) ;
#9702 = DIRECTION ( 'NONE',  ( -1.000000000000000000, 0.000000000000000000, 0.000000000000000000 ) ) ;
#9703 = CARTESIAN_POINT ( 'NONE',  ( 0.000000000000000000, 0.000000000000000000, 0.000000000000000000 ) ) ;
#9704 = CIRCLE ( 'NONE', #24081, 2.000000000000001776 ) ;
#9705 = DIRECTION ( 'NONE',  ( -1.000000000000000000, 0.000000000000000000, -0.000000000000000000 ) ) ;
#9706 = CARTESIAN_POINT ( 'NONE',  ( 46.99999662536849598, 60.62177826491077326, 17.49999999999999645 ) ) ;
#9707 = CARTESIAN_POINT ( 'NONE',  ( 39.99999662536853151, -69.28203230275519786, 17.49999999999999645 ) ) ;
#9708 = EDGE_LOOP ( 'NONE', ( #3724, #13029 ) ) ;
#9709 = ORIENTED_EDGE ( 'NONE', *, *, #23610, .T. ) ;
#9710 = DIRECTION ( 'NONE',  ( 0.000000000000000000, 0.000000000000000000, 1.000000000000000000 ) ) ;
#9711 = CARTESIAN_POINT ( 'NONE',  ( -33.99999999999945288, 58.88972745734214698, 12.49999999999999822 ) ) ;
#9712 = ORIENTED_EDGE ( 'NONE', *, *, #26850, .T. ) ;
#9713 = DIRECTION ( 'NONE',  ( 1.000000000000000000, -1.047444401652940007E-14, 0.000000000000000000 ) ) ;
#9714 = ORIENTED_EDGE ( 'NONE', *, *, #13793, .T. ) ;
#9715 = FACE_BOUND ( 'NONE', #28586, .T. ) ;
#9716 = EDGE_LOOP ( 'NONE', ( #34718, #33781 ) ) ;
#9717 = ORIENTED_EDGE ( 'NONE', *, *, #21432, .F. ) ;
#9718 = ADVANCED_FACE ( 'NONE', ( #9992, #18635, #30050, #4371, #15804, #12984, #35885, #33054, #7369 ), #30227, .F. ) ;
#9719 = CARTESIAN_POINT ( 'NONE',  ( 69.99999662536839651, -17.32050807568879947, -9.999999999999998224 ) ) ;
#9720 = ORIENTED_EDGE ( 'NONE', *, *, #28400, .F. ) ;
#9721 = PLANE ( 'NONE',  #23635 ) ;
#9722 = CIRCLE ( 'NONE', #30679, 2.000000000000001776 ) ;
#9723 = LINE ( 'NONE', #17106, #17927 ) ;
#9724 = CARTESIAN_POINT ( 'NONE',  ( -0.8333333333333292625, -5.292377467571617977, -3.818275046351179647 ) ) ;
#9725 = EDGE_LOOP ( 'NONE', ( #31498, #479 ) ) ;
#9726 = VERTEX_POINT ( 'NONE', #5655 ) ;
#9727 = EDGE_LOOP ( 'NONE', ( #7912, #16455, #804, #2297 ) ) ;
#9728 = EDGE_LOOP ( 'NONE', ( #27335, #11451 ) ) ;
#9729 = VERTEX_POINT ( 'NONE', #33622 ) ;
#9730 = DIRECTION ( 'NONE',  ( 0.000000000000000000, 0.000000000000000000, -1.000000000000000000 ) ) ;
#9731 = DIRECTION ( 'NONE',  ( 1.000000000000000000, 0.000000000000000000, 0.000000000000000000 ) ) ;
#9732 = ORIENTED_EDGE ( 'NONE', *, *, #30723, .F. ) ;
#9733 = CARTESIAN_POINT ( 'NONE',  ( -37.00000337463116296, 77.94228634059957983, 17.49999999999999645 ) ) ;
#9734 = CARTESIAN_POINT ( 'NONE',  ( 86.78953283892636250, 72.09873182956143012, 32.50000000000000000 ) ) ;
#9735 = CYLINDRICAL_SURFACE ( 'NONE', #18385, 2.000000000000001776 ) ;
#9736 = EDGE_CURVE ( 'NONE', #22407, #1861, #19360, .T. ) ;
#9737 = EDGE_LOOP ( 'NONE', ( #4114, #18839, #36151 ) ) ;
#9738 = CYLINDRICAL_SURFACE ( 'NONE', #21233, 2.000000000000001776 ) ;
#9739 = EDGE_CURVE ( 'NONE', #30643, #26836, #28561, .T. ) ;
#9740 = PLANE ( 'NONE',  #14404 ) ;
#9741 = DIRECTION ( 'NONE',  ( 0.000000000000000000, 0.000000000000000000, 1.000000000000000000 ) ) ;
#9742 = VERTEX_POINT ( 'NONE', #25543 ) ;
#9743 = FACE_OUTER_BOUND ( 'NONE', #21618, .T. ) ;
#9744 = DIRECTION ( 'NONE',  ( 0.000000000000000000, 0.000000000000000000, 1.000000000000000000 ) ) ;
#9745 = ORIENTED_EDGE ( 'NONE', *, *, #30074, .F. ) ;
#9746 = ORIENTED_EDGE ( 'NONE', *, *, #31394, .T. ) ;
#9747 = ADVANCED_FACE ( 'NONE', ( #28171 ), #36986, .F. ) ;
#9748 = CARTESIAN_POINT ( 'NONE',  ( 54.99999662536844625, 43.30127018922198801, 17.49999999999999645 ) ) ;
#9749 = CIRCLE ( 'NONE', #36126, 2.000000000000001776 ) ;
#9750 = DIRECTION ( 'NONE',  ( 0.000000000000000000, 0.000000000000000000, 1.000000000000000000 ) ) ;
#9751 = DIRECTION ( 'NONE',  ( 1.000000000000000000, 0.000000000000000000, 0.000000000000000000 ) ) ;
#9752 = VECTOR ( 'NONE', #13214, 1000.000000000000000 ) ;
#9753 = DIRECTION ( 'NONE',  ( 0.000000000000000000, -0.000000000000000000, 1.000000000000000000 ) ) ;
#9754 = ORIENTED_EDGE ( 'NONE', *, *, #25930, .F. ) ;
#9755 = CARTESIAN_POINT ( 'NONE',  ( -44.13139720814439215, -27.49999999999955591, -10.00000000000000000 ) ) ;
#9756 = DIRECTION ( 'NONE',  ( 0.000000000000000000, 0.000000000000000000, 1.000000000000000000 ) ) ;
#9757 = ORIENTED_EDGE ( 'NONE', *, *, #6127, .F. ) ;
#9758 = EDGE_CURVE ( 'NONE', #15480, #4621, #35752, .T. ) ;
#9759 = LINE ( 'NONE', #15952, #35169 ) ;
#9760 = AXIS2_PLACEMENT_3D ( 'NONE', #8513, #25944, #14506 ) ;
#9761 = VERTEX_POINT ( 'NONE', #36788 ) ;
#9762 = DIRECTION ( 'NONE',  ( -1.000000000000000000, 0.000000000000000000, 0.000000000000000000 ) ) ;
#9763 = AXIS2_PLACEMENT_3D ( 'NONE', #14627, #23454, #378 ) ;
#9764 = CARTESIAN_POINT ( 'NONE',  ( -19.13981058454750794, 60.93295298010998806, 12.49999999999999822 ) ) ;
#9765 = CARTESIAN_POINT ( 'NONE',  ( 2.981146944884248473, 4.052336700773506273, -0.5666985376598466795 ) ) ;
#9766 = ORIENTED_EDGE ( 'NONE', *, *, #13693, .F. ) ;
#9767 = ORIENTED_EDGE ( 'NONE', *, *, #3341, .T. ) ;
#9768 = ORIENTED_EDGE ( 'NONE', *, *, #27321, .T. ) ;
#9769 = CARTESIAN_POINT ( 'NONE',  ( -4.279621169095561228, 62.97617850287782915, -4.999999999999997335 ) ) ;
#9770 = AXIS2_PLACEMENT_3D ( 'NONE', #3238, #5885, #11116 ) ;
#9771 = EDGE_CURVE ( 'NONE', #7161, #29318, #12980, .T. ) ;
#9772 = DIRECTION ( 'NONE',  ( 1.000000000000000000, 0.000000000000000000, 0.000000000000000000 ) ) ;
#9773 = FACE_OUTER_BOUND ( 'NONE', #21956, .T. ) ;
#9774 = DIRECTION ( 'NONE',  ( -1.000000000000000000, 2.210166206429708225E-14, 0.000000000000000000 ) ) ;
#9775 = FACE_OUTER_BOUND ( 'NONE', #5707, .T. ) ;
#9776 = VERTEX_POINT ( 'NONE', #8311 ) ;
#9777 = DIRECTION ( 'NONE',  ( 0.000000000000000000, 0.000000000000000000, -1.000000000000000000 ) ) ;
#9778 = CARTESIAN_POINT ( 'NONE',  ( 54.99999662536844625, 60.62177826491077326, -5.000000000000000000 ) ) ;
#9779 = CARTESIAN_POINT ( 'NONE',  ( 66.99999662536842493, 43.30127018922200222, -9.999999999999998224 ) ) ;
#9780 = ORIENTED_EDGE ( 'NONE', *, *, #29396, .F. ) ;
#9781 = CARTESIAN_POINT ( 'NONE',  ( 64.99999662536841072, -25.98076211353320275, -9.999999999999998224 ) ) ;
#9782 = EDGE_CURVE ( 'NONE', #4684, #20354, #30610, .T. ) ;
#9783 = CARTESIAN_POINT ( 'NONE',  ( -70.00000337463099243, 51.96152422706637708, -9.999999999999998224 ) ) ;
#9784 = CIRCLE ( 'NONE', #34957, 2.000000000000001776 ) ;
#9785 = DIRECTION ( 'NONE',  ( 0.000000000000000000, 0.000000000000000000, 1.000000000000000000 ) ) ;
#9786 = ORIENTED_EDGE ( 'NONE', *, *, #4171, .F. ) ;
#9787 = AXIS2_PLACEMENT_3D ( 'NONE', #891, #4458, #32771 ) ;
#9788 = VERTEX_POINT ( 'NONE', #5110 ) ;
#9789 = ADVANCED_FACE ( 'NONE', ( #4927 ), #13739, .T. ) ;
#9790 = DIRECTION ( 'NONE',  ( 0.000000000000000000, 0.000000000000000000, 1.000000000000000000 ) ) ;
#9791 = DIRECTION ( 'NONE',  ( 1.000000000000000000, 0.000000000000000000, 0.000000000000000000 ) ) ;
#9792 = DIRECTION ( 'NONE',  ( 1.000000000000000000, 0.000000000000000000, 0.000000000000000000 ) ) ;
#9793 = ORIENTED_EDGE ( 'NONE', *, *, #16218, .T. ) ;
#9794 = EDGE_LOOP ( 'NONE', ( #22042, #17425, #27504 ) ) ;
#9795 = ORIENTED_EDGE ( 'NONE', *, *, #16263, .T. ) ;
#9796 = AXIS2_PLACEMENT_3D ( 'NONE', #34353, #8655, #14474 ) ;
#9797 = DIRECTION ( 'NONE',  ( 1.000000000000000000, 0.000000000000000000, 0.000000000000000000 ) ) ;
#9798 = CIRCLE ( 'NONE', #30755, 33.00000000000001421 ) ;
#9799 = ORIENTED_EDGE ( 'NONE', *, *, #2974, .T. ) ;
#9800 = ORIENTED_EDGE ( 'NONE', *, *, #2758, .T. ) ;
#9801 = DIRECTION ( 'NONE',  ( 0.000000000000000000, 0.000000000000000000, 1.000000000000000000 ) ) ;
#9802 = ORIENTED_EDGE ( 'NONE', *, *, #23165, .F. ) ;
#9803 = VECTOR ( 'NONE', #28958, 1000.000000000000000 ) ;
#9804 = ORIENTED_EDGE ( 'NONE', *, *, #22968, .T. ) ;
#9805 = EDGE_CURVE ( 'NONE', #12474, #35136, #34184, .T. ) ;
#9806 = CARTESIAN_POINT ( 'NONE',  ( -35.19434990244938888, 52.39915983220783602, 12.49999999999999822 ) ) ;
#9807 = CYLINDRICAL_SURFACE ( 'NONE', #16668, 100.0000000000000142 ) ;
#9808 = ORIENTED_EDGE ( 'NONE', *, *, #13967, .F. ) ;
#9809 = EDGE_LOOP ( 'NONE', ( #24748, #31427, #14540, #18811, #33513 ) ) ;
#9810 = DIRECTION ( 'NONE',  ( 1.000000000000000000, 0.000000000000000000, 0.000000000000000000 ) ) ;
#9811 = CARTESIAN_POINT ( 'NONE',  ( 53.72396900529356145, 62.16182810592437846, -5.000000000000000000 ) ) ;
#9812 = EDGE_CURVE ( 'NONE', #35512, #22880, #16362, .T. ) ;
#9813 = DIRECTION ( 'NONE',  ( 0.000000000000000000, 0.000000000000000000, 1.000000000000000000 ) ) ;
#9814 = CARTESIAN_POINT ( 'NONE',  ( -12.00000337463127842, -69.28203230275519786, 17.49999999999999645 ) ) ;
#9815 = AXIS2_PLACEMENT_3D ( 'NONE', #10436, #21875, #24138 ) ;
#9816 = VERTEX_POINT ( 'NONE', #28336 ) ;
#9817 = DIRECTION ( 'NONE',  ( 0.000000000000000000, 0.000000000000000000, 1.000000000000000000 ) ) ;
#9819 = EDGE_LOOP ( 'NONE', ( #29770, #7291, #29920, #18450 ) ) ;
#9818 = ADVANCED_FACE ( 'NONE', ( #25194 ), #21991, .F. ) ;
#9820 = DIRECTION ( 'NONE',  ( 0.000000000000000000, 0.000000000000000000, 1.000000000000000000 ) ) ;
#9821 = CARTESIAN_POINT ( 'NONE',  ( -25.00000337463120914, 77.94228634059957983, -9.999999999999998224 ) ) ;
#9822 = DIRECTION ( 'NONE',  ( -0.000000000000000000, -0.000000000000000000, -1.000000000000000000 ) ) ;
#9823 = DIRECTION ( 'NONE',  ( 0.4999999999999919509, -0.8660254037844433705, 0.000000000000000000 ) ) ;
#9824 = AXIS2_PLACEMENT_3D ( 'NONE', #29447, #1153, #3766 ) ;
#9825 = CARTESIAN_POINT ( 'NONE',  ( -102.5304832720503185, -102.5304832720485280, 32.55002500000000509 ) ) ;
#9826 = AXIS2_PLACEMENT_3D ( 'NONE', #4135, #569, #35066 ) ;
#9827 = CARTESIAN_POINT ( 'NONE',  ( -82.00000337463094979, -2.404119930384582903E-14, -9.999999999999998224 ) ) ;
#9828 = VERTEX_POINT ( 'NONE', #19196 ) ;
#9829 = CARTESIAN_POINT ( 'NONE',  ( 90.60231327712337190, 15.97563234535636134, -49.86561046011506448 ) ) ;
#9830 = DIRECTION ( 'NONE',  ( -1.000000000000000000, 0.000000000000000000, 0.000000000000000000 ) ) ;
#9831 = DIRECTION ( 'NONE',  ( 0.000000000000000000, 0.000000000000000000, 1.000000000000000000 ) ) ;
#9832 = EDGE_LOOP ( 'NONE', ( #1099, #34502, #13135, #24131 ) ) ;
#9833 = ORIENTED_EDGE ( 'NONE', *, *, #5642, .F. ) ;
#9834 = ORIENTED_EDGE ( 'NONE', *, *, #13336, .T. ) ;
#9835 = EDGE_CURVE ( 'NONE', #21285, #36512, #22351, .T. ) ;
#9836 = CARTESIAN_POINT ( 'NONE',  ( 5.000000000000000000, 25.00000000000000000, -15.00000000000000000 ) ) ;
#9837 = PLANE ( 'NONE',  #3261 ) ;
#9838 = DIRECTION ( 'NONE',  ( -0.000000000000000000, -0.000000000000000000, 1.000000000000000000 ) ) ;
#9839 = EDGE_LOOP ( 'NONE', ( #32782, #16693 ) ) ;
#9840 = AXIS2_PLACEMENT_3D ( 'NONE', #2291, #32713, #4239 ) ;
#9841 = CARTESIAN_POINT ( 'NONE',  ( -5.000000000000000000, 2.419979747126332903, -5.688163366729713566 ) ) ;
#9842 = CARTESIAN_POINT ( 'NONE',  ( -80.00000337463094979, 34.64101615137757051, -9.999999999999998224 ) ) ;
#9843 = ORIENTED_EDGE ( 'NONE', *, *, #4365, .F. ) ;
#9844 = CARTESIAN_POINT ( 'NONE',  ( 34.99999662536855283, -77.94228634059960825, 12.50000000000000000 ) ) ;
#9845 = ORIENTED_EDGE ( 'NONE', *, *, #36005, .F. ) ;
#9846 = CARTESIAN_POINT ( 'NONE',  ( -18.00000337463123046, 86.60254037844397601, 12.50000000000000000 ) ) ;
#9847 = CIRCLE ( 'NONE', #34406, 2.000000000000001776 ) ;
#9848 = AXIS2_PLACEMENT_3D ( 'NONE', #9150, #26414, #8440 ) ;
#9849 = ADVANCED_FACE ( 'NONE', ( #31333, #2102, #24809, #36241, #10550, #13540, #22184 ), #25002, .F. ) ;
#9850 = DIRECTION ( 'NONE',  ( 0.000000000000000000, -0.000000000000000000, -1.000000000000000000 ) ) ;
#9851 = CARTESIAN_POINT ( 'NONE',  ( -15.97563234535668109, 90.60231327712331506, -4.999999999999997335 ) ) ;
#9852 = CIRCLE ( 'NONE', #11052, 2.000000000000001776 ) ;
#9853 = DIRECTION ( 'NONE',  ( -0.000000000000000000, -0.000000000000000000, -1.000000000000000000 ) ) ;
#9854 = EDGE_CURVE ( 'NONE', #17617, #20586, #14776, .T. ) ;
#9855 = VERTEX_POINT ( 'NONE', #3053 ) ;
#9856 = DIRECTION ( 'NONE',  ( -1.000000000000000000, 0.000000000000000000, 0.000000000000000000 ) ) ;
#9857 = CONTEXT_DEPENDENT_SHAPE_REPRESENTATION ( #13756, #4109 ) ;
#9858 = EDGE_CURVE ( 'NONE', #17340, #30760, #35085, .T. ) ;
#9859 = DIRECTION ( 'NONE',  ( 0.000000000000000000, 0.000000000000000000, 1.000000000000000000 ) ) ;
#9860 = VECTOR ( 'NONE', #26193, 1000.000000000000000 ) ;
#9861 = FACE_BOUND ( 'NONE', #631, .T. ) ;
#9862 = DIRECTION ( 'NONE',  ( -1.000000000000000000, 0.000000000000000000, 0.000000000000000000 ) ) ;
#9863 = ORIENTED_EDGE ( 'NONE', *, *, #26805, .F. ) ;
#9864 = DIRECTION ( 'NONE',  ( -0.000000000000000000, -0.000000000000000000, -1.000000000000000000 ) ) ;
#9865 = AXIS2_PLACEMENT_3D ( 'NONE', #3736, #6918, #20990 ) ;
#9866 = EDGE_CURVE ( 'NONE', #17624, #8845, #10611, .T. ) ;
#9867 = DIRECTION ( 'NONE',  ( 1.000000000000000000, 0.000000000000000000, 0.000000000000000000 ) ) ;
#9868 = DIRECTION ( 'NONE',  ( 0.000000000000000000, 0.000000000000000000, -1.000000000000000000 ) ) ;
#9869 = EDGE_CURVE ( 'NONE', #22214, #13783, #9392, .T. ) ;
#9870 = VERTEX_POINT ( 'NONE', #32053 ) ;
#9871 = AXIS2_PLACEMENT_3D ( 'NONE', #8637, #2851, #14458 ) ;
#9872 = ORIENTED_EDGE ( 'NONE', *, *, #9627, .F. ) ;
#9873 = EDGE_LOOP ( 'NONE', ( #17831, #15098 ) ) ;
#9874 = CARTESIAN_POINT ( 'NONE',  ( 13.89091430021463935, 62.33939050065170306, 12.49999999999999822 ) ) ;
#9875 = DIRECTION ( 'NONE',  ( 1.000000000000000000, 0.000000000000000000, 0.000000000000000000 ) ) ;
#9876 = ADVANCED_FACE ( 'NONE', ( #28722 ), #6591, .F. ) ;
#9877 = CIRCLE ( 'NONE', #5094, 2.000000000000000000 ) ;
#9878 = EDGE_CURVE ( 'NONE', #12035, #21455, #31551, .T. ) ;
#9879 = DIRECTION ( 'NONE',  ( 0.000000000000000000, 0.000000000000000000, -1.000000000000000000 ) ) ;
#9880 = ORIENTED_EDGE ( 'NONE', *, *, #23634, .T. ) ;
#9881 = EDGE_CURVE ( 'NONE', #10138, #23997, #11765, .T. ) ;
#9882 = EDGE_CURVE ( 'NONE', #35412, #15350, #36370, .T. ) ;
#9883 = CARTESIAN_POINT ( 'NONE',  ( 74.99999662536836809, 43.30127018922198801, -9.999999999999998224 ) ) ;
#9884 = DIRECTION ( 'NONE',  ( -1.000000000000000000, 0.000000000000000000, 0.000000000000000000 ) ) ;
#9885 = ADVANCED_FACE ( 'NONE', ( #6393 ), #30938, .F. ) ;
#9886 = CARTESIAN_POINT ( 'NONE',  ( -96.90577897536184082, 67.77529820641851188, 32.50000000000000711 ) ) ;
#9887 = ORIENTED_EDGE ( 'NONE', *, *, #34978, .T. ) ;
#9888 = EDGE_LOOP ( 'NONE', ( #34938, #4416, #29477, #26353 ) ) ;
#9889 = FACE_OUTER_BOUND ( 'NONE', #3716, .T. ) ;
#9890 = FACE_OUTER_BOUND ( 'NONE', #3015, .T. ) ;
#9891 = VERTEX_POINT ( 'NONE', #25904 ) ;
#9892 = AXIS2_PLACEMENT_3D ( 'NONE', #467, #32337, #26904 ) ;
#9893 = DIRECTION ( 'NONE',  ( 0.000000000000000000, 0.000000000000000000, -1.000000000000000000 ) ) ;
#9894 = EDGE_LOOP ( 'NONE', ( #27358, #29494, #11686 ) ) ;
#9895 = LINE ( 'NONE', #24342, #33311 ) ;
#9896 = AXIS2_PLACEMENT_3D ( 'NONE', #26223, #9710, #29561 ) ;
#9897 = FACE_BOUND ( 'NONE', #14378, .T. ) ;
#9898 = EDGE_LOOP ( 'NONE', ( #8733, #12983, #19747, #10145 ) ) ;
#9899 = ORIENTED_EDGE ( 'NONE', *, *, #33865, .F. ) ;
#9900 = DIRECTION ( 'NONE',  ( 1.000000000000000000, 0.000000000000000000, 0.000000000000000000 ) ) ;
#9901 = EDGE_LOOP ( 'NONE', ( #17087, #4078, #7981, #23834 ) ) ;
#9902 = AXIS2_PLACEMENT_3D ( 'NONE', #17928, #15102, #23542 ) ;
#9903 = AXIS2_PLACEMENT_3D ( 'NONE', #27837, #16965, #22404 ) ;
#9904 = AXIS2_PLACEMENT_3D ( 'NONE', #13419, #19085, #16084 ) ;
#9905 = DIRECTION ( 'NONE',  ( 0.7071067811865489050, 0.7071067811865461294, 0.000000000000000000 ) ) ;
#9906 = DIRECTION ( 'NONE',  ( 1.000000000000000000, 0.000000000000000000, 0.000000000000000000 ) ) ;
#9907 = CARTESIAN_POINT ( 'NONE',  ( 45.00000000000000711, 5.510910596163091133E-15, 5.000000000000000000 ) ) ;
#9908 = VERTEX_POINT ( 'NONE', #23644 ) ;
#9909 = DIRECTION ( 'NONE',  ( 1.000000000000000000, 0.000000000000000000, 0.000000000000000000 ) ) ;
#9910 = ORIENTED_EDGE ( 'NONE', *, *, #9656, .F. ) ;
#9911 = ORIENTED_EDGE ( 'NONE', *, *, #26763, .F. ) ;
#9912 = ORIENTED_EDGE ( 'NONE', *, *, #27420, .F. ) ;
#9914 = DIRECTION ( 'NONE',  ( 0.000000000000000000, 0.000000000000000000, 1.000000000000000000 ) ) ;
#9913 = CIRCLE ( 'NONE', #2156, 2.000000000000001776 ) ;
#9915 = CARTESIAN_POINT ( 'NONE',  ( 76.99999662536836809, 43.30127018922198801, -9.999999999999998224 ) ) ;
#9916 = ORIENTED_EDGE ( 'NONE', *, *, #32297, .F. ) ;
#9917 = AXIS2_PLACEMENT_3D ( 'NONE', #2886, #14316, #28743 ) ;
#9918 = CARTESIAN_POINT ( 'NONE',  ( -5.000000000000000000, -0.6964580643377609181, -0.6026403643956899092 ) ) ;
#9919 = CIRCLE ( 'NONE', #23713, 2.000000000000000000 ) ;
#9920 = FACE_OUTER_BOUND ( 'NONE', #3993, .T. ) ;
#9921 = AXIS2_PLACEMENT_3D ( 'NONE', #27977, #19547, #2485 ) ;
#9922 = ORIENTED_EDGE ( 'NONE', *, *, #28649, .T. ) ;
#9923 = AXIS2_PLACEMENT_3D ( 'NONE', #12471, #32527, #15848 ) ;
#9924 = CARTESIAN_POINT ( 'NONE',  ( 104.8061974404897683, -19.22934205795014151, 32.50000000000000000 ) ) ;
#9925 = VECTOR ( 'NONE', #33698, 1000.000000000000000 ) ;
#9926 = ADVANCED_FACE ( 'NONE', ( #589 ), #25743, .F. ) ;
#9927 = CARTESIAN_POINT ( 'NONE',  ( 0.8082922630888169646, 5.306834936218043808, -0.2701150775513979641 ) ) ;
#9928 = EDGE_CURVE ( 'NONE', #22877, #12103, #20283, .T. ) ;
#9929 = CARTESIAN_POINT ( 'NONE',  ( -33.00000337463116296, 77.94228634059957983, -5.000000000000000000 ) ) ;
#9930 = DIRECTION ( 'NONE',  ( 0.000000000000000000, -0.000000000000000000, 1.000000000000000000 ) ) ;
#9931 = DIRECTION ( 'NONE',  ( 0.000000000000000000, 0.000000000000000000, 1.000000000000000000 ) ) ;
#9932 = DIRECTION ( 'NONE',  ( 0.000000000000000000, 0.000000000000000000, -1.000000000000000000 ) ) ;
#9933 = ORIENTED_EDGE ( 'NONE', *, *, #8613, .F. ) ;
#9934 = AXIS2_PLACEMENT_3D ( 'NONE', #18714, #27527, #16282 ) ;
#9935 = ORIENTED_EDGE ( 'NONE', *, *, #17611, .F. ) ;
#9936 = DIRECTION ( 'NONE',  ( 1.000000000000000000, 0.000000000000000000, 0.000000000000000000 ) ) ;
#9937 = DIRECTION ( 'NONE',  ( -1.000000000000000000, 0.000000000000000000, 0.000000000000000000 ) ) ;
#9938 = CARTESIAN_POINT ( 'NONE',  ( -37.00000337463116296, -60.62177826491080168, -5.000000000000000000 ) ) ;
#9939 = CARTESIAN_POINT ( 'NONE',  ( 145.0000000000000568, -5.056524707326808249E-13, 32.50000000000000000 ) ) ;
#9940 = ORIENTED_EDGE ( 'NONE', *, *, #19072, .T. ) ;
#9941 = UNCERTAINTY_MEASURE_WITH_UNIT (LENGTH_MEASURE( 1.000000000000000082E-05 ), #37074, 'distance_accuracy_value', 'NONE');
#9942 = AXIS2_PLACEMENT_3D ( 'NONE', #12060, #29141, #28945 ) ;
#9943 = DIRECTION ( 'NONE',  ( -1.000000000000000000, 0.000000000000000000, 0.000000000000000000 ) ) ;
#9944 = CARTESIAN_POINT ( 'NONE',  ( 65.00000000000000000, 7.960204194457797252E-15, -5.000000000000000000 ) ) ;
#9945 = VECTOR ( 'NONE', #30026, 1000.000000000000000 ) ;
#9946 = ORIENTED_EDGE ( 'NONE', *, *, #13106, .T. ) ;
#9947 = DIRECTION ( 'NONE',  ( -0.000000000000000000, -0.000000000000000000, 1.000000000000000000 ) ) ;
#9948 = ORIENTED_EDGE ( 'NONE', *, *, #28219, .T. ) ;
#9949 = AXIS2_PLACEMENT_3D ( 'NONE', #21939, #33581, #22138 ) ;
#9950 = AXIS2_PLACEMENT_3D ( 'NONE', #6389, #14634, #32046 ) ;
#9951 = EDGE_CURVE ( 'NONE', #15962, #29981, #16583, .T. ) ;
#9952 = DIRECTION ( 'NONE',  ( 0.000000000000000000, 0.000000000000000000, 1.000000000000000000 ) ) ;
#9953 = AXIS2_PLACEMENT_3D ( 'NONE', #22210, #19224, #25385 ) ;
#9954 = FACE_OUTER_BOUND ( 'NONE', #32291, .T. ) ;
#9955 = AXIS2_PLACEMENT_3D ( 'NONE', #8223, #4864, #5226 ) ;
#9956 = DIRECTION ( 'NONE',  ( 0.000000000000000000, 0.000000000000000000, 1.000000000000000000 ) ) ;
#9957 = ORIENTED_EDGE ( 'NONE', *, *, #4506, .T. ) ;
#9958 = ORIENTED_EDGE ( 'NONE', *, *, #21645, .F. ) ;
#9959 = EDGE_CURVE ( 'NONE', #25333, #33312, #3595, .T. ) ;
#9960 = ORIENTED_EDGE ( 'NONE', *, *, #34747, .T. ) ;
#9961 = DIRECTION ( 'NONE',  ( 0.000000000000000000, 0.000000000000000000, 1.000000000000000000 ) ) ;
#9962 = DIRECTION ( 'NONE',  ( 0.000000000000000000, 0.000000000000000000, 1.000000000000000000 ) ) ;
#9963 = DIRECTION ( 'NONE',  ( 1.000000000000000000, 0.000000000000000000, 0.000000000000000000 ) ) ;
#9964 = CARTESIAN_POINT ( 'NONE',  ( -19.53925848833874213, 89.94802294027088863, -23.27834620192013304 ) ) ;
#9965 = CARTESIAN_POINT ( 'NONE',  ( 0.3000000000000016542, 0.000000000000000000, 0.000000000000000000 ) ) ;
#9966 = EDGE_LOOP ( 'NONE', ( #25252, #32098, #34265, #32797 ) ) ;
#9967 = LINE ( 'NONE', #19174, #10451 ) ;
#9968 = AXIS2_PLACEMENT_3D ( 'NONE', #604, #28737, #23103 ) ;
#9969 = CARTESIAN_POINT ( 'NONE',  ( 4.220257619726806020, 79.78402657284750887, 12.50000000000000000 ) ) ;
#9970 = AXIS2_PLACEMENT_3D ( 'NONE', #3375, #14811, #26251 ) ;
#9971 = EDGE_CURVE ( 'NONE', #12428, #5388, #395, .T. ) ;
#9972 = VERTEX_POINT ( 'NONE', #20451 ) ;
#9973 = DIRECTION ( 'NONE',  ( -0.000000000000000000, -0.000000000000000000, 1.000000000000000000 ) ) ;
#9974 = AXIS2_PLACEMENT_3D ( 'NONE', #17206, #5574, #36889 ) ;
#9975 = CYLINDRICAL_SURFACE ( 'NONE', #20755, 27.00000000000001421 ) ;
#9976 = CIRCLE ( 'NONE', #14764, 2.000000000000001776 ) ;
#9977 = VECTOR ( 'NONE', #24696, 1000.000000000000000 ) ;
#9978 = ORIENTED_EDGE ( 'NONE', *, *, #5679, .T. ) ;
#9979 = CIRCLE ( 'NONE', #36334, 8.500000000000007105 ) ;
#9980 = ORIENTED_EDGE ( 'NONE', *, *, #36064, .T. ) ;
#9981 = AXIS2_PLACEMENT_3D ( 'NONE', #6694, #9308, #32945 ) ;
#9982 = LINE ( 'NONE', #28326, #12697 ) ;
#9983 = CYLINDRICAL_SURFACE ( 'NONE', #5587, 2.000000000000001776 ) ;
#9984 = CARTESIAN_POINT ( 'NONE',  ( 5.000000000000000000, 6.074766241781102566E-16, -0.5080592402122449114 ) ) ;
#9985 = ORIENTED_EDGE ( 'NONE', *, *, #7972, .F. ) ;
#9986 = VERTEX_POINT ( 'NONE', #15025 ) ;
#9987 = ORIENTED_EDGE ( 'NONE', *, *, #1203, .F. ) ;
#9988 = DIRECTION ( 'NONE',  ( -1.000000000000000000, 0.000000000000000000, 0.000000000000000000 ) ) ;
#9989 = ORIENTED_EDGE ( 'NONE', *, *, #19738, .F. ) ;
#9990 = EDGE_CURVE ( 'NONE', #30219, #8984, #26451, .T. ) ;
#9991 = VERTEX_POINT ( 'NONE', #11828 ) ;
#9992 = FACE_BOUND ( 'NONE', #22072, .T. ) ;
#9993 = VERTEX_POINT ( 'NONE', #760 ) ;
#9994 = EDGE_CURVE ( 'NONE', #34620, #8381, #4623, .T. ) ;
#9995 = AXIS2_PLACEMENT_3D ( 'NONE', #9604, #12951, #3968 ) ;
#9996 = ORIENTED_EDGE ( 'NONE', *, *, #10957, .F. ) ;
#9997 = FACE_OUTER_BOUND ( 'NONE', #3194, .T. ) ;
#9998 = CIRCLE ( 'NONE', #6408, 2.000000000000000000 ) ;
#9999 = CLOSED_SHELL ( 'NONE', ( #35667, #28786, #32791, #17591, #30964, #31218, #29280, #10725, #22495, #18607, #10225, #27325, #27485, #3148, #8996, #24589, #35538, #23841, #22946, #26638, #4191, #16734, #21097, #14097, #17544, #21055, #6169, #29486, #34571, #13784, #9277, #32424, #6388, #1603, #1763, #28680, #22595, #25690, #19671, #9319, #34371, #3050, #20215, #16436, #25737, #32140, #35534, #7151, #34609, #23797, #6379, #25913, #18431, #24293, #10322, #17034, #13775, #24694, #21351, #24401, #27177, #22422, #773, #30232, #9559, #27752, #4392, #22251, #25725, #24661, #36160, #10960, #28940, #5343, #5834, #2701, #24904, #12696, #34164, #23961, #31968, #8466, #21488, #17960, #13033, #25824, #32432, #13887, #14105, #9876, #5312, #13346, #23438, #22801, #32814, #5963, #12847, #8593, #3086, #13898, #8522, #2076, #2371, #29107, #6897, #15018, #17265, #29807, #8939, #7722, #22955, #5516, #33511, #25436, #13350, #36268, #29536, #11825, #14145, #25931, #33917, #34074, #14459, #13724, #29012, #17460, #25014, #34860, #12871, #30215, #1324, #12124, #34735, #14607, #390, #2984, #3848, #10613, #3463, #7753, #1064, #7969, #13943, #947, #14454, #16392, #12782, #3682, #33027, #12180, #28396, #29436, #28528, #9198, #25175, #6235, #14797, #23342, #27958, #12671, #33921, #4847, #33645, #31201, #11108, #10496, #16082, #36568, #1455, #15859, #2732, #36009, #10053, #15235, #3014, #9023, #14625, #26050, #1418, #5672, #10465, #13728, #8266, #1686, #12752, #20019, #32343, #24501, #23572, #16083, #25336, #31777, #20418, #27165, #35346, #29053, #27304, #24920, #27938, #28194, #19765, #22635, #3885, #8410, #33535, #25925, #32775, #7612, #5326, #10684, #20001, #11939, #23589, #26185, #20394, #7021, #9747, #4187, #15317, #26381, #22629, #26173, #16653, #33040, #12122, #26916, #21036, #159, #10413, #3594, #13113, #17571, #10325, #17712, #32681, #30828, #29569, #19665, #5535, #33373, #12335, #24941, #7495, #14975, #33531, #1160, #34421, #35541, #36020, #2777, #32031, #19436, #23605, #14708, #11893, #11019, #36724, #27296, #28669, #10950, #10201, #35888, #756, #3169, #21517, #11172, #30734, #33835, #20075, #29133, #4552, #15169, #14772, #26041, #21733, #1144, #4389, #13449, #12749, #27536, #16514, #4865, #34627, #26025, #2999, #2500, #27591, #21281, #23740, #37021, #3442, #15443, #28634, #5073, #30747, #4853, #5404, #33962, #14690, #7803, #4301, #32542, #34066, #30631, #17777, #33179, #33044, #11636, #25513, #24322, #15655, #8576, #4512, #9849, #9718, #11057, #13307, #23303, #10033, #20865, #9190, #22053, #2345, #17462, #18694, #1194, #1343, #5090, #842, #23853, #15808, #25676, #20555, #21683, #4048, #16895, #25093, #19374, #30652, #24680, #8292, #13502, #32248, #7536, #21256, #35743, #7136, #36943, #35123, #7332, #8450, #14701, #13983, #12411, #32503, #19356, #36416, #17373, #17783, #15337, #16701, #36948, #23260, #35652, #13370, #31460, #24710, #263, #7605, #35226, #9173, #1096, #9165, #29328, #14366, #12816, #4726, #36725, #4386, #2713, #6572, #6470, #33469, #36914, #30895, #25586, #24195, #29993, #31205, #6009, #33397, #30416, #10012, #25402, #26790, #34508, #5309, #10262, #8525, #25846, #1838, #27627, #22029, #15387, #26361, #18825, #21727, #21335, #6919, #25580, #35734, #20454, #34208, #11663, #14416, #25723, #10894, #30939, #29490, #26160, #28054, #25073, #10002, #14008, #15639, #26111, #35708, #30644, #2762, #7286, #12625, #26060, #6541, #10832, #478, #26933, #33244, #14325, #6286, #6771, #5775, #24103, #24602, #35855, #13412, #5693, #17194, #19220, #30134, #22215, #1958, #29717, #9548, #25406, #23190, #3116, #21892, #24670, #30280, #24541, #35327, #24096, #1351, #14000, #19531, #8272, #23186, #6806, #1687, #5224, #14822, #6630, #36060, #9345, #13565, #16925, #3710, #22226, #23323, #25245, #35569, #26035, #28853, #28721, #20983, #15398, #18281, #32357, #27548, #23356, #12506, #23847, #11015, #35600, #18134, #15507, #33272, #32559, #17419, #16470, #16608, #36024, #12927, #23064, #8899, #9590, #28007, #22897, #6114, #33465, #8061, #1501, #30511, #11608, #15034, #13348, #18329, #20899, #25046, #6804, #23225, #28132, #36675, #20946, #36037, #5995, #26575, #25807, #9401, #27897, #8051, #29740, #18870, #6646, #19163, #2775, #17449, #17083, #18934, #16039, #25240, #18625, #1895, #34997, #27805, #9818, #15194, #4452, #34862, #24638, #7079, #18286, #19257, #19913, #33483, #13108, #9660, #29707, #15752, #11139, #31780, #15989, #37070, #7153, #8895, #25053, #32764, #23729, #3621, #26866, #10242, #10144, #4163, #16621, #23110, #32270, #19398, #34326, #10698, #24842, #30944, #8294, #7716, #2549, #1417, #24327, #34783, #17524, #31544, #25615, #10587, #14931, #6766, #5317, #8942, #30411, #14500, #33659, #37099, #8979, #30595, #31823, #8008, #8435, #29206, #3512, #6163, #31678, #17406, #22293, #4588, #27220, #18130, #12541, #31636, #36580, #8341, #28752, #7258, #28009, #10552, #17661, #30485, #7253, #34563, #11928, #9180, #22681, #9304, #1286, #7134, #31284, #11924, #32446, #23026, #5412, #17822, #1161, #17938, #18538, #15611, #26591, #21327, #19279, #19749, #9482, #2554, #21625, #31622, #8479, #10992, #20876, #12632, #33185, #21664, #8961, #27779, #27523, #17291, #27449, #17659, #2486, #31211, #22620, #21214, #27007, #20285, #31158, #14699, #17916, #15951, #6447, #10111, #28220, #34670, #29472, #14486, #28999, #28817, #28353, #7051, #17595, #36250, #17311, #21239, #15677, #3642, #14439, #20263, #1756, #24773, #31184, #13936, #5872, #33298, #34837, #30689, #17432, #26722, #8474, #19546, #17267, #32788, #35358, #35289, #15656, #28324, #3379, #6905, #5630, #9789, #36661, #20663, #36478, #13970, #29767, #30533, #2066, #27398, #10457, #4382, #24275, #15651, #25993, #23868, #22334, #30662, #36496, #24992, #12043, #34267, #24736, #10134, #21820, #25465, #29949, #23101, #34555, #36177, #14067, #9415, #31608, #7703, #31299, #12017, #17892, #13894, #29819, #36492, #23339, #16005, #5037, #8710, #21815, #12873, #7995, #12437, #29061, #14590, #10788, #25306 ) ) ;
#10000 = CYLINDRICAL_SURFACE ( 'NONE', #14864, 2.000000000000001776 ) ;
#10001 = ORIENTED_EDGE ( 'NONE', *, *, #12609, .F. ) ;
#10002 = ADVANCED_FACE ( 'NONE', ( #34732 ), #34349, .F. ) ;
#10003 = ORIENTED_EDGE ( 'NONE', *, *, #10930, .F. ) ;
#10004 = AXIS2_PLACEMENT_3D ( 'NONE', #4246, #30277, #4611 ) ;
#10005 = DIRECTION ( 'NONE',  ( 0.000000000000000000, -1.000000000000000000, 1.034244904716769672E-15 ) ) ;
#10006 = DIRECTION ( 'NONE',  ( 0.000000000000000000, 0.000000000000000000, 1.000000000000000000 ) ) ;
#10007 = CIRCLE ( 'NONE', #13595, 1.999999999999998224 ) ;
#10008 = LINE ( 'NONE', #15456, #12661 ) ;
#10009 = DIRECTION ( 'NONE',  ( 0.000000000000000000, 0.000000000000000000, 1.000000000000000000 ) ) ;
#10010 = AXIS2_PLACEMENT_3D ( 'NONE', #2816, #17048, #16705 ) ;
#10011 = AXIS2_PLACEMENT_3D ( 'NONE', #6099, #31770, #25620 ) ;
#10012 = ADVANCED_FACE ( 'NONE', ( #10152 ), #21194, .F. ) ;
#10013 = EDGE_LOOP ( 'NONE', ( #30779, #7060 ) ) ;
#10014 = DIRECTION ( 'NONE',  ( 1.000000000000000000, 0.000000000000000000, 0.000000000000000000 ) ) ;
#10015 = ORIENTED_EDGE ( 'NONE', *, *, #14703, .T. ) ;
#10016 = DIRECTION ( 'NONE',  ( 1.000000000000000000, 0.000000000000000000, 0.000000000000000000 ) ) ;
#10017 = LINE ( 'NONE', #35369, #25618 ) ;
#10018 = CARTESIAN_POINT ( 'NONE',  ( -85.00000337463092137, 25.98076211353317433, -9.999999999999998224 ) ) ;
#10019 = CIRCLE ( 'NONE', #36422, 2.000000000000001776 ) ;
#10020 = DIRECTION ( 'NONE',  ( 0.000000000000000000, 0.000000000000000000, 1.000000000000000000 ) ) ;
#10021 = FACE_OUTER_BOUND ( 'NONE', #12677, .T. ) ;
#10022 = AXIS2_PLACEMENT_3D ( 'NONE', #27386, #1707, #10317 ) ;
#10023 = CARTESIAN_POINT ( 'NONE',  ( 3.000000000000000000, 0.000000000000000000, 0.000000000000000000 ) ) ;
#10024 = EDGE_CURVE ( 'NONE', #12218, #22555, #25577, .T. ) ;
#10025 = DIRECTION ( 'NONE',  ( 0.000000000000000000, 0.000000000000000000, -1.000000000000000000 ) ) ;
#10026 = ORIENTED_EDGE ( 'NONE', *, *, #33706, .F. ) ;
#10027 = DIRECTION ( 'NONE',  ( 0.000000000000000000, 0.000000000000000000, 1.000000000000000000 ) ) ;
#10028 = AXIS2_PLACEMENT_3D ( 'NONE', #13366, #5335, #31189 ) ;
#10029 = PLANE ( 'NONE',  #31481 ) ;
#10030 = FACE_OUTER_BOUND ( 'NONE', #30036, .T. ) ;
#10031 = AXIS2_PLACEMENT_3D ( 'NONE', #3061, #601, #23473 ) ;
#10032 = EDGE_LOOP ( 'NONE', ( #17468, #32434, #28410, #31277 ) ) ;
#10033 = ADVANCED_FACE ( 'NONE', ( #7154 ), #35472, .T. ) ;
#10034 = ORIENTED_EDGE ( 'NONE', *, *, #15128, .T. ) ;
#10035 = ORIENTED_EDGE ( 'NONE', *, *, #17199, .T. ) ;
#10036 = AXIS2_PLACEMENT_3D ( 'NONE', #30716, #25125, #4876 ) ;
#10037 = CARTESIAN_POINT ( 'NONE',  ( 5.999999999999998224, 0.000000000000000000, 0.000000000000000000 ) ) ;
#10038 = CYLINDRICAL_SURFACE ( 'NONE', #30181, 2.000000000000001776 ) ;
#10039 = CARTESIAN_POINT ( 'NONE',  ( -3.000003374631269981, -77.94228634059960825, 12.50000000000000000 ) ) ;
#10040 = ORIENTED_EDGE ( 'NONE', *, *, #33222, .T. ) ;
#10041 = MECHANICAL_DESIGN_GEOMETRIC_PRESENTATION_REPRESENTATION (  '', ( #29690 ), #21410 ) ;
#10042 = EDGE_CURVE ( 'NONE', #20202, #29611, #9759, .T. ) ;
#10043 = CIRCLE ( 'NONE', #19627, 0.2500000000000002220 ) ;
#10044 = AXIS2_PLACEMENT_3D ( 'NONE', #1927, #21995, #24812 ) ;
#10045 = DIRECTION ( 'NONE',  ( -0.000000000000000000, -0.000000000000000000, 1.000000000000000000 ) ) ;
#10046 = DIRECTION ( 'NONE',  ( 1.000000000000000000, 0.000000000000000000, 0.000000000000000000 ) ) ;
#10047 = VERTEX_POINT ( 'NONE', #15762 ) ;
#10048 = EDGE_CURVE ( 'NONE', #21760, #8155, #26635, .T. ) ;
#10049 = FACE_OUTER_BOUND ( 'NONE', #1920, .T. ) ;
#10050 = VERTEX_POINT ( 'NONE', #23843 ) ;
#10051 = FACE_BOUND ( 'NONE', #23451, .T. ) ;
#10052 = CIRCLE ( 'NONE', #14833, 3.000000000000002665 ) ;
#10053 = ADVANCED_FACE ( 'NONE', ( #3950 ), #18764, .F. ) ;
#10054 = LINE ( 'NONE', #18500, #36359 ) ;
#10055 = CARTESIAN_POINT ( 'NONE',  ( -50.00000337463109190, 51.96152422706637708, 17.49999999999999645 ) ) ;
#10056 = AXIS2_PLACEMENT_3D ( 'NONE', #18533, #29955, #18706 ) ;
#10057 = EDGE_CURVE ( 'NONE', #2026, #12842, #32625, .T. ) ;
#10058 = EDGE_LOOP ( 'NONE', ( #25206, #5998, #30213, #3648 ) ) ;
#10059 = DIRECTION ( 'NONE',  ( 0.000000000000000000, 0.000000000000000000, -1.000000000000000000 ) ) ;
#10060 = AXIS2_PLACEMENT_3D ( 'NONE', #36326, #5391, #27512 ) ;
#10061 = VECTOR ( 'NONE', #20645, 1000.000000000000000 ) ;
#10062 = ITEM_DEFINED_TRANSFORMATION ( 'NONE', 'NONE', #28516,  #21385 ) ;
#10063 = AXIS2_PLACEMENT_3D ( 'NONE', #28093, #25457, #36549 ) ;
#10064 = CARTESIAN_POINT ( 'NONE',  ( -18.00000337463123756, -86.60254037844400443, -5.000000000000000000 ) ) ;
#10065 = ADVANCED_FACE ( 'NONE', ( #24398 ), #33990, .T. ) ;
#10066 = VECTOR ( 'NONE', #10939, 1000.000000000000000 ) ;
#10067 = FACE_OUTER_BOUND ( 'NONE', #15193, .T. ) ;
#10068 = FACE_OUTER_BOUND ( 'NONE', #32880, .T. ) ;
#10069 = VERTEX_POINT ( 'NONE', #18399 ) ;
#10070 = FACE_OUTER_BOUND ( 'NONE', #6116, .T. ) ;
#10071 = DIRECTION ( 'NONE',  ( -1.000000000000000000, 0.000000000000000000, 0.000000000000000000 ) ) ;
#10072 = CARTESIAN_POINT ( 'NONE',  ( -60.00000337463108480, -51.96152422706641971, 12.50000000000000000 ) ) ;
#10073 = VECTOR ( 'NONE', #2042, 1000.000000000000000 ) ;
#10074 = ORIENTED_EDGE ( 'NONE', *, *, #33427, .T. ) ;
#10075 = ORIENTED_EDGE ( 'NONE', *, *, #13539, .T. ) ;
#10076 = CARTESIAN_POINT ( 'NONE',  ( -42.00000337463114164, 69.28203230275516944, 17.49999999999999645 ) ) ;
#10077 = AXIS2_PLACEMENT_3D ( 'NONE', #14007, #2969, #8221 ) ;
#10078 = DIRECTION ( 'NONE',  ( -0.000000000000000000, -0.000000000000000000, -1.000000000000000000 ) ) ;
#10079 = CARTESIAN_POINT ( 'NONE',  ( 66.99999662536839651, 60.62177826491078747, -9.999999999999998224 ) ) ;
#10080 = ADVANCED_FACE ( 'NONE', ( #13141 ), #26835, .T. ) ;
#10081 = EDGE_LOOP ( 'NONE', ( #10189, #7568, #2526, #34230, #24074 ) ) ;
#10082 = VECTOR ( 'NONE', #25009, 1000.000000000000000 ) ;
#10083 = CARTESIAN_POINT ( 'NONE',  ( 74.99999662536836809, 25.98076211353319565, -9.999999999999998224 ) ) ;
#10084 = DIRECTION ( 'NONE',  ( 0.000000000000000000, 0.000000000000000000, 1.000000000000000000 ) ) ;
#10085 = AXIS2_PLACEMENT_3D ( 'NONE', #22511, #33963, #31144 ) ;
#10086 = DIRECTION ( 'NONE',  ( 0.000000000000000000, 0.000000000000000000, 1.000000000000000000 ) ) ;
#10087 = FACE_OUTER_BOUND ( 'NONE', #11529, .T. ) ;
#10088 = ORIENTED_EDGE ( 'NONE', *, *, #30556, .F. ) ;
#10089 = AXIS2_PLACEMENT_3D ( 'NONE', #9086, #14531, #32334 ) ;
#10090 = EDGE_CURVE ( 'NONE', #25333, #520, #1644, .T. ) ;
#10091 = ORIENTED_EDGE ( 'NONE', *, *, #24087, .F. ) ;
#10092 = SURFACE_SIDE_STYLE ('',( #12689 ) ) ;
#10093 = AXIS2_PLACEMENT_3D ( 'NONE', #12768, #19345, #36222 ) ;
#10094 = DIRECTION ( 'NONE',  ( 1.000000000000000000, 0.000000000000000000, 0.000000000000000000 ) ) ;
#10095 = ORIENTED_EDGE ( 'NONE', *, *, #22834, .T. ) ;
#10096 = EDGE_CURVE ( 'NONE', #4290, #17808, #1148, .T. ) ;
#10097 = CARTESIAN_POINT ( 'NONE',  ( 84.99999662536832545, 25.98076211353319565, -5.000000000000000000 ) ) ;
#10098 = EDGE_CURVE ( 'NONE', #13035, #15480, #21396, .T. ) ;
#10099 = ORIENTED_EDGE ( 'NONE', *, *, #4077, .T. ) ;
#10100 = DIRECTION ( 'NONE',  ( 1.000000000000000000, 0.000000000000000000, 0.000000000000000000 ) ) ;
#10101 = CIRCLE ( 'NONE', #29327, 27.00000000000001776 ) ;
#10102 = CIRCLE ( 'NONE', #5901, 2.500000000000000444 ) ;
#10103 = DIRECTION ( 'NONE',  ( -0.8660254037844453689, -0.4999999999999882871, 0.000000000000000000 ) ) ;
#10104 = ORIENTED_EDGE ( 'NONE', *, *, #21748, .T. ) ;
#10105 = ORIENTED_EDGE ( 'NONE', *, *, #5059, .T. ) ;
#10106 = DIRECTION ( 'NONE',  ( 0.000000000000000000, 0.000000000000000000, 1.000000000000000000 ) ) ;
#10107 = ORIENTED_EDGE ( 'NONE', *, *, #14913, .T. ) ;
#10108 = AXIS2_PLACEMENT_3D ( 'NONE', #23760, #9513, #3317 ) ;
#10109 = PRESENTATION_STYLE_ASSIGNMENT (( #19285 ) ) ;
#10110 = CARTESIAN_POINT ( 'NONE',  ( -10.00000337463128197, 86.60254037844397601, 12.50000000000000000 ) ) ;
#10111 = ADVANCED_FACE ( 'NONE', ( #33011 ), #6758, .T. ) ;
#10112 = CIRCLE ( 'NONE', #6519, 2.000000000000001776 ) ;
#10113 = CYLINDRICAL_SURFACE ( 'NONE', #23304, 2.000000000000001776 ) ;
#10114 = LINE ( 'NONE', #21715, #21508 ) ;
#10115 = ORIENTED_EDGE ( 'NONE', *, *, #26643, .T. ) ;
#10116 = CARTESIAN_POINT ( 'NONE',  ( -20.00000337463123756, -69.28203230275522628, 17.49999999999999645 ) ) ;
#10117 = FACE_OUTER_BOUND ( 'NONE', #5709, .T. ) ;
#10118 = EDGE_LOOP ( 'NONE', ( #15682, #4100, #30956, #23538 ) ) ;
#10119 = ORIENTED_EDGE ( 'NONE', *, *, #15165, .F. ) ;
#10120 = ORIENTED_EDGE ( 'NONE', *, *, #32709, .T. ) ;
#10121 = DIRECTION ( 'NONE',  ( 0.000000000000000000, 0.000000000000000000, -1.000000000000000000 ) ) ;
#10122 = VECTOR ( 'NONE', #19232, 1000.000000000000000 ) ;
#10123 = DIRECTION ( 'NONE',  ( 0.000000000000000000, 0.000000000000000000, 1.000000000000000000 ) ) ;
#10124 = ORIENTED_EDGE ( 'NONE', *, *, #7829, .F. ) ;
#10125 = DIRECTION ( 'NONE',  ( 0.000000000000000000, 0.000000000000000000, 1.000000000000000000 ) ) ;
#10126 = FACE_OUTER_BOUND ( 'NONE', #35456, .T. ) ;
#10127 = CIRCLE ( 'NONE', #23286, 2.000000000000001776 ) ;
#10128 = VERTEX_POINT ( 'NONE', #24027 ) ;
#10129 = DIRECTION ( 'NONE',  ( 0.5000000000000014433, 0.8660254037844378194, -0.000000000000000000 ) ) ;
#10130 = CARTESIAN_POINT ( 'NONE',  ( 62.33939050065184517, -13.89091430021398565, 12.49999999999999822 ) ) ;
#10131 = EDGE_CURVE ( 'NONE', #2314, #9400, #7507, .T. ) ;
#10132 = CARTESIAN_POINT ( 'NONE',  ( -2.500000000000022204, 4.330127018922177662, 0.000000000000000000 ) ) ;
#10133 = CARTESIAN_POINT ( 'NONE',  ( 49.99999662536846756, 51.96152422706637708, -9.999999999999998224 ) ) ;
#10134 = ADVANCED_FACE ( 'NONE', ( #21392 ), #29444, .T. ) ;
#10135 = CARTESIAN_POINT ( 'NONE',  ( 69.99999662536839651, 17.32050807568879236, -9.999999999999998224 ) ) ;
#10136 = DIRECTION ( 'NONE',  ( -0.000000000000000000, -0.000000000000000000, 1.000000000000000000 ) ) ;
#10137 = ORIENTED_EDGE ( 'NONE', *, *, #10816, .T. ) ;
#10138 = VERTEX_POINT ( 'NONE', #21018 ) ;
#10139 = FILL_AREA_STYLE ('',( #30729 ) ) ;
#10140 = CIRCLE ( 'NONE', #22103, 2.000000000000001776 ) ;
#10141 = CARTESIAN_POINT ( 'NONE',  ( 79.99999662536832545, -34.64101615137759183, -9.999999999999998224 ) ) ;
#10142 = DIRECTION ( 'NONE',  ( 0.000000000000000000, 0.000000000000000000, 1.000000000000000000 ) ) ;
#10143 = CARTESIAN_POINT ( 'NONE',  ( 22.99999662536859901, -77.94228634059960825, -9.999999999999998224 ) ) ;
#10144 = ADVANCED_FACE ( 'NONE', ( #22142 ), #11244, .F. ) ;
#10145 = ORIENTED_EDGE ( 'NONE', *, *, #1047, .F. ) ;
#10146 = AXIS2_PLACEMENT_3D ( 'NONE', #32586, #15346, #1287 ) ;
#10147 = CARTESIAN_POINT ( 'NONE',  ( 3.000000000000000000, -2.935248768560059229, 3.469446951953614189E-15 ) ) ;
#10148 = DIRECTION ( 'NONE',  ( -1.000000000000000000, 0.000000000000000000, 0.000000000000000000 ) ) ;
#10149 = CARTESIAN_POINT ( 'NONE',  ( -10.49238116876062499, -117.7011972391635908, 32.50000000000000000 ) ) ;
#10150 = ORIENTED_EDGE ( 'NONE', *, *, #7960, .T. ) ;
#10151 = CIRCLE ( 'NONE', #6553, 2.000000000000000000 ) ;
#10152 = FACE_OUTER_BOUND ( 'NONE', #23566, .T. ) ;
#10153 = ORIENTED_EDGE ( 'NONE', *, *, #35245, .T. ) ;
#10154 = AXIS2_PLACEMENT_3D ( 'NONE', #19826, #22639, #22438 ) ;
#10155 = EDGE_CURVE ( 'NONE', #30219, #34090, #14041, .T. ) ;
#10156 = CARTESIAN_POINT ( 'NONE',  ( 69.99999662536839651, -3.469446951953614189E-15, -9.999999999999998224 ) ) ;
#10157 = EDGE_CURVE ( 'NONE', #18000, #34714, #25493, .T. ) ;
#10158 = DIRECTION ( 'NONE',  ( 1.000000000000000000, 0.000000000000000000, 0.000000000000000000 ) ) ;
#10159 = VECTOR ( 'NONE', #34994, 1000.000000000000000 ) ;
#10160 = EDGE_CURVE ( 'NONE', #17753, #4797, #10502, .T. ) ;
#10161 = CARTESIAN_POINT ( 'NONE',  ( 1.324703144935786447, 5.008684974571240289, -0.8655517945778323785 ) ) ;
#10162 = ADVANCED_FACE ( 'NONE', ( #19501 ), #18954, .F. ) ;
#10163 = VERTEX_POINT ( 'NONE', #25150 ) ;
#10164 = AXIS2_PLACEMENT_3D ( 'NONE', #24262, #24471, #33259 ) ;
#10165 = VERTEX_POINT ( 'NONE', #13868 ) ;
#10166 = ORIENTED_EDGE ( 'NONE', *, *, #7266, .T. ) ;
#10167 = CYLINDRICAL_SURFACE ( 'NONE', #8213, 2.000000000000000000 ) ;
#10168 = AXIS2_PLACEMENT_3D ( 'NONE', #20945, #17949, #12283 ) ;
#10169 = FACE_BOUND ( 'NONE', #967, .T. ) ;
#10170 = CIRCLE ( 'NONE', #25145, 2.000000000000000000 ) ;
#10171 = FACE_OUTER_BOUND ( 'NONE', #15164, .T. ) ;
#10172 = CARTESIAN_POINT ( 'NONE',  ( 0.000000000000000000, 89.94802294027088863, -19.99999999999999645 ) ) ;
#10173 = DIRECTION ( 'NONE',  ( -1.000000000000000000, -0.000000000000000000, -0.000000000000000000 ) ) ;
#10174 = ORIENTED_EDGE ( 'NONE', *, *, #2765, .T. ) ;
#10175 = DIRECTION ( 'NONE',  ( -1.000000000000000000, 0.000000000000000000, -0.000000000000000000 ) ) ;
#10176 = DIRECTION ( 'NONE',  ( 0.000000000000000000, 0.000000000000000000, 1.000000000000000000 ) ) ;
#10177 = DIRECTION ( 'NONE',  ( 1.000000000000000000, 0.000000000000000000, 0.000000000000000000 ) ) ;
#10178 = VERTEX_POINT ( 'NONE', #2259 ) ;
#10179 = CARTESIAN_POINT ( 'NONE',  ( -33.00000337463116296, -60.62177826491080168, 17.49999999999999645 ) ) ;
#10180 = DIRECTION ( 'NONE',  ( -0.000000000000000000, -0.000000000000000000, 1.000000000000000000 ) ) ;
#10181 = EDGE_CURVE ( 'NONE', #18894, #25339, #8235, .T. ) ;
#10182 = EDGE_LOOP ( 'NONE', ( #13300, #14436, #18773, #14727, #31929, #32613 ) ) ;
#10183 = VERTEX_POINT ( 'NONE', #28125 ) ;
#10184 = DIRECTION ( 'NONE',  ( 0.000000000000000000, 0.000000000000000000, 1.000000000000000000 ) ) ;
#10185 = CIRCLE ( 'NONE', #19185, 2.000000000000001776 ) ;
#10186 = CARTESIAN_POINT ( 'NONE',  ( 35.83991598322140248, 56.52018970185221036, 12.49999999999999645 ) ) ;
#10187 = DIRECTION ( 'NONE',  ( 0.000000000000000000, 0.000000000000000000, 1.000000000000000000 ) ) ;
#10188 = ORIENTED_EDGE ( 'NONE', *, *, #21206, .T. ) ;
#10189 = ORIENTED_EDGE ( 'NONE', *, *, #727, .T. ) ;
#10190 = ORIENTED_EDGE ( 'NONE', *, *, #15142, .T. ) ;
#10191 = CARTESIAN_POINT ( 'NONE',  ( -37.00000337463117717, -77.94228634059963667, -9.999999999999998224 ) ) ;
#10192 = VECTOR ( 'NONE', #12237, 1000.000000000000000 ) ;
#10193 = EDGE_LOOP ( 'NONE', ( #11352, #30043, #36019, #34318, #23338 ) ) ;
#10194 = EDGE_LOOP ( 'NONE', ( #28525, #32967, #26259, #7898 ) ) ;
#10195 = CIRCLE ( 'NONE', #9, 27.00000000000001421 ) ;
#10196 = CARTESIAN_POINT ( 'NONE',  ( 56.67878100130369035, -27.78182860042797131, -4.999999999999997335 ) ) ;
#10197 = ORIENTED_EDGE ( 'NONE', *, *, #20216, .T. ) ;
#10198 = ORIENTED_EDGE ( 'NONE', *, *, #28772, .F. ) ;
#10199 = CARTESIAN_POINT ( 'NONE',  ( -5.750000000000000000, 89.94802294027094547, 32.49999999999999289 ) ) ;
#10200 = DIRECTION ( 'NONE',  ( 1.000000000000000000, 0.000000000000000000, 0.000000000000000000 ) ) ;
#10201 = ADVANCED_FACE ( 'NONE', ( #36935 ), #19693, .F. ) ;
#10202 = EDGE_LOOP ( 'NONE', ( #11078, #12611 ) ) ;
#10203 = VECTOR ( 'NONE', #3624, 1000.000000000000000 ) ;
#10204 = EDGE_LOOP ( 'NONE', ( #23084, #11515, #5940, #9144 ) ) ;
#10205 = CARTESIAN_POINT ( 'NONE',  ( 19.99999662536858835, 69.28203230275516944, 17.49999999999999645 ) ) ;
#10206 = DIRECTION ( 'NONE',  ( 0.000000000000000000, 0.000000000000000000, 1.000000000000000000 ) ) ;
#10207 = CIRCLE ( 'NONE', #25180, 2.000000000000001776 ) ;
#10208 = DIRECTION ( 'NONE',  ( -1.000000000000000000, 0.000000000000000000, 0.000000000000000000 ) ) ;
#10209 = CARTESIAN_POINT ( 'NONE',  ( 11.99999662536862566, 86.60254037844397601, -5.000000000000000000 ) ) ;
#10210 = ORIENTED_EDGE ( 'NONE', *, *, #131, .T. ) ;
#10211 = DIRECTION ( 'NONE',  ( 0.000000000000000000, 0.000000000000000000, 1.000000000000000000 ) ) ;
#10212 = ORIENTED_EDGE ( 'NONE', *, *, #35368, .T. ) ;
#10213 = DIRECTION ( 'NONE',  ( 1.000000000000000000, 0.000000000000000000, 0.000000000000000000 ) ) ;
#10214 = CARTESIAN_POINT ( 'NONE',  ( 34.99999662536855283, -77.94228634059960825, -9.999999999999998224 ) ) ;
#10215 = AXIS2_PLACEMENT_3D ( 'NONE', #35620, #26803, #9560 ) ;
#10216 = FACE_BOUND ( 'NONE', #10740, .T. ) ;
#10217 = DIRECTION ( 'NONE',  ( 0.000000000000000000, 0.000000000000000000, 1.000000000000000000 ) ) ;
#10218 = CARTESIAN_POINT ( 'NONE',  ( -107.2742589609544410, 47.50000425637879431, 32.50001250000000397 ) ) ;
#10219 = CARTESIAN_POINT ( 'NONE',  ( 5.999999999999998224, 145.0000000000000568, 27.50000000000000000 ) ) ;
#10220 = DIRECTION ( 'NONE',  ( 0.000000000000000000, 0.000000000000000000, -1.000000000000000000 ) ) ;
#10221 = ORIENTED_EDGE ( 'NONE', *, *, #6007, .T. ) ;
#10222 = PLANE ( 'NONE',  #30953 ) ;
#10223 = FACE_OUTER_BOUND ( 'NONE', #4342, .T. ) ;
#10224 = CARTESIAN_POINT ( 'NONE',  ( -7.000003374631269537, -77.94228634059960825, -9.999999999999998224 ) ) ;
#10225 = ADVANCED_FACE ( 'NONE', ( #2449 ), #27742, .T. ) ;
#10226 = EDGE_CURVE ( 'NONE', #36602, #27228, #8257, .T. ) ;
#10227 = ORIENTED_EDGE ( 'NONE', *, *, #18809, .F. ) ;
#10228 = ORIENTED_EDGE ( 'NONE', *, *, #31974, .F. ) ;
#10229 = ORIENTED_EDGE ( 'NONE', *, *, #26970, .T. ) ;
#10230 = CARTESIAN_POINT ( 'NONE',  ( 0.000000000000000000, 0.000000000000000000, -5.974599999999999689 ) ) ;
#10231 = CYLINDRICAL_SURFACE ( 'NONE', #9472, 95.00000000000001421 ) ;
#10232 = ORIENTED_EDGE ( 'NONE', *, *, #13222, .F. ) ;
#10233 = CARTESIAN_POINT ( 'NONE',  ( 37.50000000000000000, 103.4105893997321743, 32.50000000000000000 ) ) ;
#10234 = EDGE_CURVE ( 'NONE', #9552, #32504, #26630, .T. ) ;
#10235 = DIRECTION ( 'NONE',  ( 0.000000000000000000, 0.000000000000000000, 1.000000000000000000 ) ) ;
#10236 = ORIENTED_EDGE ( 'NONE', *, *, #21954, .T. ) ;
#10237 = FACE_BOUND ( 'NONE', #3501, .T. ) ;
#10238 = ORIENTED_EDGE ( 'NONE', *, *, #16117, .F. ) ;
#10239 = CARTESIAN_POINT ( 'NONE',  ( -35.00000337463116296, 77.94228634059957983, -5.000000000000000000 ) ) ;
#10240 = DIRECTION ( 'NONE',  ( 0.000000000000000000, 0.000000000000000000, 1.000000000000000000 ) ) ;
#10241 = CARTESIAN_POINT ( 'NONE',  ( 36.97203788309026606, -58.48108235278833433, 12.49999999999999645 ) ) ;
#10242 = ADVANCED_FACE ( 'NONE', ( #1885 ), #24956, .F. ) ;
#10243 = VERTEX_POINT ( 'NONE', #22491 ) ;
#10244 = DIRECTION ( 'NONE',  ( -0.000000000000000000, -0.000000000000000000, 1.000000000000000000 ) ) ;
#10245 = CARTESIAN_POINT ( 'NONE',  ( 46.00000000000000000, 103.4105893997321743, -19.99999999999999645 ) ) ;
#10246 = DIRECTION ( 'NONE',  ( -0.000000000000000000, 1.000000000000000000, 0.000000000000000000 ) ) ;
#10247 = FACE_BOUND ( 'NONE', #36315, .T. ) ;
#10248 = CARTESIAN_POINT ( 'NONE',  ( 47.99999662536846756, 69.28203230275516944, -9.999999999999998224 ) ) ;
#10249 = EDGE_LOOP ( 'NONE', ( #17260, #29229, #31440, #1390 ) ) ;
#10250 = LINE ( 'NONE', #21680, #17795 ) ;
#10251 = LINE ( 'NONE', #29939, #24439 ) ;
#10252 = DIRECTION ( 'NONE',  ( -1.000000000000000000, 0.000000000000000000, -0.000000000000000000 ) ) ;
#10253 = EDGE_LOOP ( 'NONE', ( #9027, #24341, #22735, #31264 ) ) ;
#10254 = ADVANCED_FACE ( 'NONE', ( #16152 ), #28295, .T. ) ;
#10255 = VERTEX_POINT ( 'NONE', #21945 ) ;
#10256 = DIRECTION ( 'NONE',  ( -0.000000000000000000, -0.000000000000000000, 1.000000000000000000 ) ) ;
#10257 = LINE ( 'NONE', #21688, #21181 ) ;
#10258 = LINE ( 'NONE', #36321, #22487 ) ;
#10259 = ORIENTED_EDGE ( 'NONE', *, *, #15734, .F. ) ;
#10260 = DIRECTION ( 'NONE',  ( -0.000000000000000000, -0.000000000000000000, -1.000000000000000000 ) ) ;
#10261 = CYLINDRICAL_SURFACE ( 'NONE', #1540, 3.500000000000003109 ) ;
#10262 = ADVANCED_FACE ( 'NONE', ( #30739 ), #30577, .F. ) ;
#10263 = CARTESIAN_POINT ( 'NONE',  ( 17.99999662536858835, 69.28203230275516944, -9.999999999999998224 ) ) ;
#10264 = DIRECTION ( 'NONE',  ( 0.000000000000000000, 0.000000000000000000, 1.000000000000000000 ) ) ;
#10265 = VERTEX_POINT ( 'NONE', #13695 ) ;
#10266 = ORIENTED_EDGE ( 'NONE', *, *, #9001, .F. ) ;
#10267 = CARTESIAN_POINT ( 'NONE',  ( 11.99999662536865763, -69.28203230275519786, -9.999999999999998224 ) ) ;
#10268 = EDGE_CURVE ( 'NONE', #12416, #7360, #17628, .T. ) ;
#10269 = DIRECTION ( 'NONE',  ( -1.000000000000000000, 0.000000000000000000, -0.000000000000000000 ) ) ;
#10270 = VERTEX_POINT ( 'NONE', #10874 ) ;
#10271 = FACE_OUTER_BOUND ( 'NONE', #9894, .T. ) ;
#10272 = ORIENTED_EDGE ( 'NONE', *, *, #233, .F. ) ;
#10273 = AXIS2_PLACEMENT_3D ( 'NONE', #19316, #10309, #1877 ) ;
#10274 = CARTESIAN_POINT ( 'NONE',  ( -94.40806000769299544, 12.15049814296761888, 27.50000000000000000 ) ) ;
#10275 = CARTESIAN_POINT ( 'NONE',  ( -55.00000337463107059, 43.30127018922197379, 17.49999999999999645 ) ) ;
#10276 = ORIENTED_EDGE ( 'NONE', *, *, #23273, .F. ) ;
#10277 = DIRECTION ( 'NONE',  ( 0.000000000000000000, 0.000000000000000000, 1.000000000000000000 ) ) ;
#10278 = ORIENTED_EDGE ( 'NONE', *, *, #31637, .F. ) ;
#10279 = DIRECTION ( 'NONE',  ( 1.000000000000000000, 0.000000000000000000, 0.000000000000000000 ) ) ;
#10280 = DIRECTION ( 'NONE',  ( 0.000000000000000000, 0.000000000000000000, -1.000000000000000000 ) ) ;
#10281 = ADVANCED_FACE ( 'NONE', ( #32003 ), #14206, .F. ) ;
#10282 = LINE ( 'NONE', #33146, #29913 ) ;
#10283 = CARTESIAN_POINT ( 'NONE',  ( 76.99999662536836809, 8.660254037844394404, -9.999999999999998224 ) ) ;
#10284 = EDGE_LOOP ( 'NONE', ( #28419, #5820, #8804, #13198 ) ) ;
#10285 = DIRECTION ( 'NONE',  ( 1.000000000000000000, 0.000000000000000000, 0.000000000000000000 ) ) ;
#10286 = CARTESIAN_POINT ( 'NONE',  ( 59.99999662536842493, -51.96152422706639840, -9.999999999999998224 ) ) ;
#10287 = FACE_OUTER_BOUND ( 'NONE', #11127, .T. ) ;
#10288 = ORIENTED_EDGE ( 'NONE', *, *, #22430, .T. ) ;
#10289 = EDGE_CURVE ( 'NONE', #33284, #32298, #29587, .T. ) ;
#10290 = EDGE_LOOP ( 'NONE', ( #15965, #17816, #35140, #17300 ) ) ;
#10291 = ORIENTED_EDGE ( 'NONE', *, *, #18340, .F. ) ;
#10292 = VECTOR ( 'NONE', #25369, 1000.000000000000000 ) ;
#10293 = EDGE_CURVE ( 'NONE', #15817, #27467, #17050, .T. ) ;
#10294 = DIRECTION ( 'NONE',  ( 0.000000000000000000, 0.000000000000000000, -1.000000000000000000 ) ) ;
#10295 = ORIENTED_EDGE ( 'NONE', *, *, #2915, .T. ) ;
#10296 = LINE ( 'NONE', #2591, #33115 ) ;
#10297 = CARTESIAN_POINT ( 'NONE',  ( -60.93295298010992411, -19.13981058454771755, 12.49999999999999822 ) ) ;
#10298 = CARTESIAN_POINT ( 'NONE',  ( 27.99999662536855993, 69.28203230275518365, -9.999999999999998224 ) ) ;
#10299 = DIRECTION ( 'NONE',  ( 1.000000000000000000, 0.000000000000000000, 0.000000000000000000 ) ) ;
#10300 = DIRECTION ( 'NONE',  ( 1.000000000000000000, 0.000000000000000000, 0.000000000000000000 ) ) ;
#10301 = DIRECTION ( 'NONE',  ( -1.000000000000000000, 3.491481338843133750E-15, 0.000000000000000000 ) ) ;
#10302 = DIRECTION ( 'NONE',  ( 0.000000000000000000, 0.000000000000000000, 1.000000000000000000 ) ) ;
#10303 = DIRECTION ( 'NONE',  ( -1.000000000000000000, 0.000000000000000000, 0.000000000000000000 ) ) ;
#10304 = VERTEX_POINT ( 'NONE', #8987 ) ;
#10305 = ORIENTED_EDGE ( 'NONE', *, *, #30442, .T. ) ;
#10306 = DIRECTION ( 'NONE',  ( 0.000000000000000000, -0.000000000000000000, -1.000000000000000000 ) ) ;
#10307 = EDGE_CURVE ( 'NONE', #15870, #26836, #14047, .T. ) ;
#10308 = DIRECTION ( 'NONE',  ( -1.000000000000000000, -0.000000000000000000, -0.000000000000000000 ) ) ;
#10309 = DIRECTION ( 'NONE',  ( 0.000000000000000000, 0.000000000000000000, 1.000000000000000000 ) ) ;
#10310 = CYLINDRICAL_SURFACE ( 'NONE', #13705, 2.000000000000001776 ) ;
#10311 = ORIENTED_EDGE ( 'NONE', *, *, #9612, .T. ) ;
#10312 = DIRECTION ( 'NONE',  ( -0.000000000000000000, -0.000000000000000000, -1.000000000000000000 ) ) ;
#10313 = CARTESIAN_POINT ( 'NONE',  ( 74.99999662536836809, 25.98076211353319565, 12.50000000000000000 ) ) ;
#10314 = DIRECTION ( 'NONE',  ( 0.000000000000000000, 0.000000000000000000, 1.000000000000000000 ) ) ;
#10315 = ORIENTED_EDGE ( 'NONE', *, *, #24600, .T. ) ;
#10316 = CONICAL_SURFACE ( 'NONE', #25289, 20.00000000000001066, 0.1396263401595466691 ) ;
#10317 = DIRECTION ( 'NONE',  ( 1.000000000000000000, 0.000000000000000000, 0.000000000000000000 ) ) ;
#10318 = ORIENTED_EDGE ( 'NONE', *, *, #8383, .T. ) ;
#10319 =( NAMED_UNIT ( * ) SI_UNIT ( $, .STERADIAN. ) SOLID_ANGLE_UNIT ( ) );
#10320 = CARTESIAN_POINT ( 'NONE',  ( -111.8061974404896262, 19.22934205795090534, 32.50000000000000000 ) ) ;
#10321 = DIRECTION ( 'NONE',  ( 1.000000000000000000, 0.000000000000000000, 0.000000000000000000 ) ) ;
#10322 = ADVANCED_FACE ( 'NONE', ( #14985 ), #31665, .F. ) ;
#10323 = CARTESIAN_POINT ( 'NONE',  ( -65.00000337463106348, -60.62177826491083010, 12.50000000000000000 ) ) ;
#10324 = ORIENTED_EDGE ( 'NONE', *, *, #34444, .F. ) ;
#10325 = ADVANCED_FACE ( 'NONE', ( #12129 ), #11587, .F. ) ;
#10326 = ORIENTED_EDGE ( 'NONE', *, *, #32068, .F. ) ;
#10327 = FACE_OUTER_BOUND ( 'NONE', #36354, .T. ) ;
#10328 = EDGE_CURVE ( 'NONE', #31169, #40, #28995, .T. ) ;
#10329 = CIRCLE ( 'NONE', #18114, 2.000000000000001776 ) ;
#10330 = ORIENTED_EDGE ( 'NONE', *, *, #13858, .T. ) ;
#10331 = DIRECTION ( 'NONE',  ( 0.000000000000000000, 0.000000000000000000, 1.000000000000000000 ) ) ;
#10332 = CYLINDRICAL_SURFACE ( 'NONE', #30532, 2.000000000000001776 ) ;
#10333 = EDGE_CURVE ( 'NONE', #10511, #10440, #17041, .T. ) ;
#10334 = DIRECTION ( 'NONE',  ( -1.000000000000000000, 0.000000000000000000, 0.000000000000000000 ) ) ;
#10335 = DIRECTION ( 'NONE',  ( -0.5000000000000098810, -0.8660254037844328234, 0.000000000000000000 ) ) ;
#10336 = DIRECTION ( 'NONE',  ( 0.000000000000000000, 0.000000000000000000, 1.000000000000000000 ) ) ;
#10337 = EDGE_CURVE ( 'NONE', #5470, #20921, #23637, .T. ) ;
#10338 = VERTEX_POINT ( 'NONE', #20041 ) ;
#10339 = DIRECTION ( 'NONE',  ( -0.000000000000000000, -0.000000000000000000, 1.000000000000000000 ) ) ;
#10340 = DIRECTION ( 'NONE',  ( 0.000000000000000000, 0.000000000000000000, 1.000000000000000000 ) ) ;
#10341 = AXIS2_PLACEMENT_3D ( 'NONE', #36594, #19522, #11265 ) ;
#10342 = DIRECTION ( 'NONE',  ( 1.000000000000000000, 0.000000000000000000, 0.000000000000000000 ) ) ;
#10343 = ORIENTED_EDGE ( 'NONE', *, *, #20735, .T. ) ;
#10344 = CIRCLE ( 'NONE', #156, 150.0000000000000284 ) ;
#10345 = DIRECTION ( 'NONE',  ( 0.000000000000000000, 0.000000000000000000, 1.000000000000000000 ) ) ;
#10346 = FACE_OUTER_BOUND ( 'NONE', #9809, .T. ) ;
#10347 = EDGE_CURVE ( 'NONE', #10265, #15896, #26234, .T. ) ;
#10348 = ORIENTED_EDGE ( 'NONE', *, *, #16519, .T. ) ;
#10349 = EDGE_CURVE ( 'NONE', #10338, #27157, #19868, .T. ) ;
#10350 = VERTEX_POINT ( 'NONE', #25695 ) ;
#10351 = EDGE_CURVE ( 'NONE', #623, #4050, #31468, .T. ) ;
#10352 = EDGE_CURVE ( 'NONE', #2354, #10426, #3003, .T. ) ;
#10353 = CARTESIAN_POINT ( 'NONE',  ( -55.00000337463109901, -60.62177826491083010, -9.999999999999998224 ) ) ;
#10354 = DIRECTION ( 'NONE',  ( -0.000000000000000000, -0.000000000000000000, 1.000000000000000000 ) ) ;
#10355 = CARTESIAN_POINT ( 'NONE',  ( -5.854691731421723944E-14, -5.773502691896269745, -0.5999999999999998668 ) ) ;
#10356 = ORIENTED_EDGE ( 'NONE', *, *, #29143, .T. ) ;
#10357 = ORIENTED_EDGE ( 'NONE', *, *, #5444, .F. ) ;
#10358 = ORIENTED_EDGE ( 'NONE', *, *, #7003, .T. ) ;
#10359 = DIRECTION ( 'NONE',  ( 0.000000000000000000, 0.000000000000000000, 1.000000000000000000 ) ) ;
#10360 = CIRCLE ( 'NONE', #19331, 2.000000000000001776 ) ;
#10361 = ORIENTED_EDGE ( 'NONE', *, *, #31081, .F. ) ;
#10362 = CARTESIAN_POINT ( 'NONE',  ( -85.00000337463092137, -25.98076211353322051, 17.49999999999999645 ) ) ;
#10363 = EDGE_LOOP ( 'NONE', ( #34270, #9226, #62, #34153 ) ) ;
#10364 = ORIENTED_EDGE ( 'NONE', *, *, #4087, .T. ) ;
#10365 = DIRECTION ( 'NONE',  ( 0.000000000000000000, 0.000000000000000000, -1.000000000000000000 ) ) ;
#10366 = VECTOR ( 'NONE', #21263, 1000.000000000000000 ) ;
#10367 = CARTESIAN_POINT ( 'NONE',  ( -75.00000337463097821, 25.98076211353318854, -9.999999999999998224 ) ) ;
#10368 = ORIENTED_EDGE ( 'NONE', *, *, #6912, .T. ) ;
#10369 = VERTEX_POINT ( 'NONE', #341 ) ;
#10370 = DIRECTION ( 'NONE',  ( 0.000000000000000000, 0.000000000000000000, 1.000000000000000000 ) ) ;
#10371 = DIRECTION ( 'NONE',  ( 0.000000000000000000, 0.000000000000000000, -1.000000000000000000 ) ) ;
#10372 = DIRECTION ( 'NONE',  ( 1.000000000000000000, 0.000000000000000000, 0.000000000000000000 ) ) ;
#10373 = DIRECTION ( 'NONE',  ( 1.000000000000000000, 0.000000000000000000, 0.000000000000000000 ) ) ;
#10374 = ORIENTED_EDGE ( 'NONE', *, *, #1242, .F. ) ;
#10375 = DIRECTION ( 'NONE',  ( 1.000000000000000000, 0.000000000000000000, 0.000000000000000000 ) ) ;
#10376 = ORIENTED_EDGE ( 'NONE', *, *, #9680, .F. ) ;
#10377 = DIRECTION ( 'NONE',  ( -0.4999999999999977796, 0.8660254037844398178, 0.000000000000000000 ) ) ;
#10378 = LINE ( 'NONE', #1214, #29764 ) ;
#10379 = DIRECTION ( 'NONE',  ( 0.000000000000000000, 0.000000000000000000, -1.000000000000000000 ) ) ;
#10380 = CARTESIAN_POINT ( 'NONE',  ( 65.44550000000002399, 0.000000000000000000, 3.000000000000000444 ) ) ;
#10381 = CARTESIAN_POINT ( 'NONE',  ( 108.3061974404898820, 19.22934205794938478, 32.50000000000000000 ) ) ;
#10382 = AXIS2_PLACEMENT_3D ( 'NONE', #14977, #11416, #5800 ) ;
#10383 = DIRECTION ( 'NONE',  ( 0.000000000000000000, 0.000000000000000000, -1.000000000000000000 ) ) ;
#10384 = CARTESIAN_POINT ( 'NONE',  ( 0.3000000000000016542, 6.123233995736766282E-16, -5.000000000000000000 ) ) ;
#10385 = ORIENTED_EDGE ( 'NONE', *, *, #18561, .F. ) ;
#10386 = CARTESIAN_POINT ( 'NONE',  ( -42.00000337463114164, 69.28203230275516944, 12.50000000000000000 ) ) ;
#10387 = DIRECTION ( 'NONE',  ( 1.000000000000000000, 0.000000000000000000, 0.000000000000000000 ) ) ;
#10388 = DIRECTION ( 'NONE',  ( -1.000000000000000000, 0.000000000000000000, 0.000000000000000000 ) ) ;
#10389 = AXIS2_PLACEMENT_3D ( 'NONE', #17301, #11635, #30287 ) ;
#10390 = ORIENTED_EDGE ( 'NONE', *, *, #2368, .T. ) ;
#10391 = EDGE_LOOP ( 'NONE', ( #17413, #13662, #3326, #16586, #12076, #1322 ) ) ;
#10392 = EDGE_LOOP ( 'NONE', ( #30815, #15757, #22689, #15811, #9629 ) ) ;
#10393 = AXIS2_PLACEMENT_3D ( 'NONE', #22566, #34024, #8334 ) ;
#10394 = EDGE_CURVE ( 'NONE', #16962, #15109, #25864, .T. ) ;
#10395 = DIRECTION ( 'NONE',  ( 0.000000000000000000, 0.000000000000000000, 1.000000000000000000 ) ) ;
#10396 = DIRECTION ( 'NONE',  ( 1.000000000000000000, 0.000000000000000000, 0.000000000000000000 ) ) ;
#10397 = ORIENTED_EDGE ( 'NONE', *, *, #29339, .T. ) ;
#10398 = CIRCLE ( 'NONE', #13980, 2.000000000000000000 ) ;
#10399 = PRODUCT ( 'rotor hub', 'rotor hub', '', ( #12666 ) ) ;
#10400 = DIRECTION ( 'NONE',  ( 1.000000000000000000, 0.000000000000000000, 0.000000000000000000 ) ) ;
#10401 = DIRECTION ( 'NONE',  ( 1.000000000000000000, 0.000000000000000000, 0.000000000000000000 ) ) ;
#10402 = ORIENTED_EDGE ( 'NONE', *, *, #18406, .F. ) ;
#10403 = DIRECTION ( 'NONE',  ( 0.000000000000000000, 0.000000000000000000, -1.000000000000000000 ) ) ;
#10404 = ORIENTED_EDGE ( 'NONE', *, *, #28790, .T. ) ;
#10405 = FACE_BOUND ( 'NONE', #31060, .T. ) ;
#10406 = AXIS2_PLACEMENT_3D ( 'NONE', #16434, #30858, #22820 ) ;
#10407 = CARTESIAN_POINT ( 'NONE',  ( 0.000000000000000000, 0.000000000000000000, 0.000000000000000000 ) ) ;
#10408 = DIRECTION ( 'NONE',  ( 0.000000000000000000, 0.000000000000000000, 1.000000000000000000 ) ) ;
#10409 = DIRECTION ( 'NONE',  ( 0.000000000000000000, 0.000000000000000000, 1.000000000000000000 ) ) ;
#10410 = ORIENTED_EDGE ( 'NONE', *, *, #36470, .T. ) ;
#10411 = FACE_OUTER_BOUND ( 'NONE', #29858, .T. ) ;
#10412 = APPLICATION_PROTOCOL_DEFINITION ( 'draft international standard', 'automotive_design', 1998, #24048 ) ;
#10413 = ADVANCED_FACE ( 'NONE', ( #34488 ), #5999, .F. ) ;
#10414 = VECTOR ( 'NONE', #25411, 1000.000000000000000 ) ;
#10415 = CARTESIAN_POINT ( 'NONE',  ( 82.27241335952147949, -47.50000000000039790, 27.50000000000000000 ) ) ;
#10416 = CARTESIAN_POINT ( 'NONE',  ( 44.99999662536849598, -77.94228634059960825, 12.50000000000000000 ) ) ;
#10417 = VERTEX_POINT ( 'NONE', #3166 ) ;
#10418 = VECTOR ( 'NONE', #24423, 1000.000000000000114 ) ;
#10419 = CARTESIAN_POINT ( 'NONE',  ( 102.5304832720496080, 102.5304832720492527, 27.50000000000000000 ) ) ;
#10420 = DIRECTION ( 'NONE',  ( 0.000000000000000000, 0.000000000000000000, 1.000000000000000000 ) ) ;
#10421 = EDGE_LOOP ( 'NONE', ( #35731, #2288 ) ) ;
#10422 = DIRECTION ( 'NONE',  ( 1.000000000000000000, 0.000000000000000000, 0.000000000000000000 ) ) ;
#10423 = CYLINDRICAL_SURFACE ( 'NONE', #31618, 2.000000000000001776 ) ;
#10424 = DIRECTION ( 'NONE',  ( -1.000000000000000000, 0.000000000000000000, 0.000000000000000000 ) ) ;
#10425 = EDGE_CURVE ( 'NONE', #23671, #4724, #7475, .T. ) ;
#10426 = VERTEX_POINT ( 'NONE', #18721 ) ;
#10427 = ORIENTED_EDGE ( 'NONE', *, *, #36172, .T. ) ;
#10428 = B_SPLINE_CURVE_WITH_KNOTS ( 'NONE', 3,
 ( #10858, #31449, #5791, #36911, #22466, #17229 ),
 .UNSPECIFIED., .F., .F.,
 ( 4, 2, 4 ),
 ( 0.002950759650825688762, 0.004429055062152286240, 0.005907350473478884152 ),
 .UNSPECIFIED. ) ;
#10429 = DIRECTION ( 'NONE',  ( -0.000000000000000000, 0.000000000000000000, -1.000000000000000000 ) ) ;
#10430 = DIRECTION ( 'NONE',  ( 0.000000000000000000, 0.000000000000000000, -1.000000000000000000 ) ) ;
#10431 = PRESENTATION_LAYER_ASSIGNMENT (  '', '', ( #32584 ) ) ;
#10432 = CARTESIAN_POINT ( 'NONE',  ( 62.97617850287784336, 4.279621169095339184, 12.49999999999999822 ) ) ;
#10433 = ORIENTED_EDGE ( 'NONE', *, *, #33507, .T. ) ;
#10434 = EDGE_LOOP ( 'NONE', ( #11400, #28658 ) ) ;
#10435 = EDGE_CURVE ( 'NONE', #29294, #545, #4480, .T. ) ;
#10436 = CARTESIAN_POINT ( 'NONE',  ( -60.00000337463104216, 34.64101615137757051, 12.50000000000000000 ) ) ;
#10437 = CARTESIAN_POINT ( 'NONE',  ( -77.00000337463099243, -25.98076211353322051, -5.000000000000000000 ) ) ;
#10438 = CARTESIAN_POINT ( 'NONE',  ( -10.00000337463127842, -69.28203230275519786, -9.999999999999998224 ) ) ;
#10439 = CARTESIAN_POINT ( 'NONE',  ( -38.00000337463113453, 69.28203230275516944, -9.999999999999998224 ) ) ;
#10440 = VERTEX_POINT ( 'NONE', #26784 ) ;
#10441 = CONICAL_SURFACE ( 'NONE', #31385, 4.999999999999997335, 0.9110539511682894664 ) ;
#10442 = VERTEX_POINT ( 'NONE', #15904 ) ;
#10443 = DIRECTION ( 'NONE',  ( 0.000000000000000000, 0.000000000000000000, 1.000000000000000000 ) ) ;
#10444 = VECTOR ( 'NONE', #36179, 1000.000000000000000 ) ;
#10445 = CYLINDRICAL_SURFACE ( 'NONE', #17680, 2.000000000000001776 ) ;
#10446 = ORIENTED_EDGE ( 'NONE', *, *, #36465, .F. ) ;
#10447 = DIRECTION ( 'NONE',  ( 0.4999999999999919509, -0.8660254037844432595, 0.000000000000000000 ) ) ;
#10448 = EDGE_LOOP ( 'NONE', ( #31940, #20240, #30044, #17670 ) ) ;
#10449 = DIRECTION ( 'NONE',  ( 0.000000000000000000, 0.000000000000000000, 1.000000000000000000 ) ) ;
#10450 = DIRECTION ( 'NONE',  ( 1.000000000000000000, 0.000000000000000000, -0.000000000000000000 ) ) ;
#10451 = VECTOR ( 'NONE', #21966, 1000.000000000000000 ) ;
#10452 = VERTEX_POINT ( 'NONE', #901 ) ;
#10453 = EDGE_CURVE ( 'NONE', #4684, #35726, #6263, .T. ) ;
#10454 = AXIS2_PLACEMENT_3D ( 'NONE', #22811, #25971, #273 ) ;
#10455 = CARTESIAN_POINT ( 'NONE',  ( 3.417629563432034612, 3.800333343458349944, -3.719399823475519895 ) ) ;
#10456 = ORIENTED_EDGE ( 'NONE', *, *, #33227, .F. ) ;
#10457 = ADVANCED_FACE ( 'NONE', ( #23985 ), #15720, .T. ) ;
#10458 = PRESENTATION_STYLE_ASSIGNMENT (( #24721 ) ) ;
#10459 = AXIS2_PLACEMENT_3D ( 'NONE', #7494, #18752, #27372 ) ;
#10460 = CARTESIAN_POINT ( 'NONE',  ( -4.191707736911189031, 3.353419101626330612, -0.2701150775513885272 ) ) ;
#10461 = CYLINDRICAL_SURFACE ( 'NONE', #36515, 2.000000000000001776 ) ;
#10462 = DIRECTION ( 'NONE',  ( -1.000000000000000000, 0.000000000000000000, 0.000000000000000000 ) ) ;
#10463 = EDGE_LOOP ( 'NONE', ( #5030, #19390, #4833, #1705 ) ) ;
#10464 = CARTESIAN_POINT ( 'NONE',  ( -47.00000337463111322, -77.94228634059960825, -9.999999999999998224 ) ) ;
#10465 = ADVANCED_FACE ( 'NONE', ( #6548 ), #4289, .F. ) ;
#10466 = LINE ( 'NONE', #36897, #5861 ) ;
#10467 = DIRECTION ( 'NONE',  ( -0.7071067811865288100, 0.000000000000000000, 0.7071067811865663355 ) ) ;
#10468 = VERTEX_POINT ( 'NONE', #15154 ) ;
#10469 = AXIS2_PLACEMENT_3D ( 'NONE', #22275, #11391, #16840 ) ;
#10470 = VERTEX_POINT ( 'NONE', #15544 ) ;
#10471 = EDGE_CURVE ( 'NONE', #6640, #12600, #35036, .T. ) ;
#10472 = VERTEX_POINT ( 'NONE', #12527 ) ;
#10473 = AXIS2_PLACEMENT_3D ( 'NONE', #15866, #27291, #18866 ) ;
#10474 = CARTESIAN_POINT ( 'NONE',  ( 47.04203867989577503, -43.19957991610382919, 12.49999999999999822 ) ) ;
#10475 = VERTEX_POINT ( 'NONE', #13093 ) ;
#10476 = CARTESIAN_POINT ( 'NONE',  ( -5.000000000000000000, -1.096207231254244352, -0.7463930790433302986 ) ) ;
#10477 = DIRECTION ( 'NONE',  ( 0.000000000000000000, 0.000000000000000000, 1.000000000000000000 ) ) ;
#10478 = DIRECTION ( 'NONE',  ( 0.8660254037844344888, -0.5000000000000071054, 0.000000000000000000 ) ) ;
#10479 = VECTOR ( 'NONE', #15117, 1000.000000000000000 ) ;
#10480 = LINE ( 'NONE', #10680, #20021 ) ;
#10481 = LINE ( 'NONE', #29806, #2925 ) ;
#10482 = CARTESIAN_POINT ( 'NONE',  ( -85.17994309527703933, -72.40128952002849871, 32.50000000000000000 ) ) ;
#10483 = AXIS2_PLACEMENT_3D ( 'NONE', #27250, #33073, #15652 ) ;
#10484 = CARTESIAN_POINT ( 'NONE',  ( -10.00000337463125000, -86.60254037844400443, -9.999999999999998224 ) ) ;
#10485 = CARTESIAN_POINT ( 'NONE',  ( -2.775557561562891351E-14, 19.94802294027085310, 18.49999999999999645 ) ) ;
#10486 = ORIENTED_EDGE ( 'NONE', *, *, #25672, .F. ) ;
#10487 = CIRCLE ( 'NONE', #302, 2.000000000000001776 ) ;
#10488 = ORIENTED_EDGE ( 'NONE', *, *, #3481, .F. ) ;
#10489 = EDGE_CURVE ( 'NONE', #36483, #357, #13429, .T. ) ;
#10490 = DIRECTION ( 'NONE',  ( 0.000000000000000000, 0.000000000000000000, -1.000000000000000000 ) ) ;
#10491 = CARTESIAN_POINT ( 'NONE',  ( 44.99999662536849598, -77.94228634059960825, -9.999999999999998224 ) ) ;
#10492 = FACE_OUTER_BOUND ( 'NONE', #28592, .T. ) ;
#10493 = DIRECTION ( 'NONE',  ( 0.000000000000000000, 0.000000000000000000, 1.000000000000000000 ) ) ;
#10494 = ORIENTED_EDGE ( 'NONE', *, *, #31407, .F. ) ;
#10495 = AXIS2_PLACEMENT_3D ( 'NONE', #9508, #23393, #17746 ) ;
#10496 = ADVANCED_FACE ( 'NONE', ( #15341 ), #21152, .F. ) ;
#10497 = VECTOR ( 'NONE', #24637, 1000.000000000000000 ) ;
#10498 = DIRECTION ( 'NONE',  ( -1.000000000000000000, 6.167905692361977800E-15, 0.000000000000000000 ) ) ;
#10499 = DIRECTION ( 'NONE',  ( 0.000000000000000000, 0.000000000000000000, 1.000000000000000000 ) ) ;
#10500 = ORIENTED_EDGE ( 'NONE', *, *, #884, .F. ) ;
#10501 = EDGE_CURVE ( 'NONE', #16545, #716, #20779, .T. ) ;
#10502 = LINE ( 'NONE', #30926, #19607 ) ;
#10503 = ORIENTED_EDGE ( 'NONE', *, *, #20570, .F. ) ;
#10504 =( LENGTH_UNIT ( ) NAMED_UNIT ( * ) SI_UNIT ( .MILLI., .METRE. ) );
#10505 = CYLINDRICAL_SURFACE ( 'NONE', #34710, 2.000000000000001776 ) ;
#10506 = DIRECTION ( 'NONE',  ( -0.000000000000000000, -0.000000000000000000, -1.000000000000000000 ) ) ;
#10507 = CIRCLE ( 'NONE', #29031, 2.000000000000001776 ) ;
#10508 = FACE_OUTER_BOUND ( 'NONE', #11277, .T. ) ;
#10509 = EDGE_LOOP ( 'NONE', ( #29195, #35874, #10410, #5192 ) ) ;
#10510 = CIRCLE ( 'NONE', #917, 2.000000000000001776 ) ;
#10511 = VERTEX_POINT ( 'NONE', #6902 ) ;
#10512 = CIRCLE ( 'NONE', #18299, 2.000000000000001776 ) ;
#10513 = AXIS2_PLACEMENT_3D ( 'NONE', #36288, #33281, #28717 ) ;
#10514 = CIRCLE ( 'NONE', #12917, 2.000000000000000000 ) ;
#10515 = EDGE_CURVE ( 'NONE', #27674, #21403, #19442, .T. ) ;
#10516 = ORIENTED_EDGE ( 'NONE', *, *, #7266, .F. ) ;
#10517 = DIRECTION ( 'NONE',  ( 0.000000000000000000, 0.000000000000000000, 1.000000000000000000 ) ) ;
#10518 = FACE_OUTER_BOUND ( 'NONE', #13380, .T. ) ;
#10519 = DIRECTION ( 'NONE',  ( 0.000000000000000000, 0.000000000000000000, -1.000000000000000000 ) ) ;
#10520 = DIRECTION ( 'NONE',  ( -1.000000000000000000, -0.000000000000000000, -0.000000000000000000 ) ) ;
#10521 = CARTESIAN_POINT ( 'NONE',  ( -47.63139720814438505, -27.49999999999955591, -10.00000000000000000 ) ) ;
#10522 = VERTEX_POINT ( 'NONE', #18345 ) ;
#10523 = FACE_OUTER_BOUND ( 'NONE', #11982, .T. ) ;
#10524 = AXIS2_PLACEMENT_3D ( 'NONE', #7080, #27120, #1436 ) ;
#10525 = CYLINDRICAL_SURFACE ( 'NONE', #11973, 2.000000000000000000 ) ;
#10526 =( NAMED_UNIT ( * ) PLANE_ANGLE_UNIT ( ) SI_UNIT ( $, .RADIAN. ) );
#10527 = ORIENTED_EDGE ( 'NONE', *, *, #6352, .F. ) ;
#10528 = DIRECTION ( 'NONE',  ( 0.000000000000000000, 0.4999999999999953926, 0.8660254037844412611 ) ) ;
#10529 = CYLINDRICAL_SURFACE ( 'NONE', #986, 3.499999999999996003 ) ;
#10530 = EDGE_LOOP ( 'NONE', ( #8994, #6488, #25480, #4115, #27817 ) ) ;
#10531 = ORIENTED_EDGE ( 'NONE', *, *, #18213, .F. ) ;
#10532 = EDGE_CURVE ( 'NONE', #14697, #30372, #16441, .T. ) ;
#10533 = AXIS2_PLACEMENT_3D ( 'NONE', #2331, #20110, #31352 ) ;
#10534 = CARTESIAN_POINT ( 'NONE',  ( 86.99999662536831124, -25.98076211353319565, -9.999999999999998224 ) ) ;
#10535 = DIRECTION ( 'NONE',  ( 1.000000000000000000, 0.000000000000000000, 0.000000000000000000 ) ) ;
#10536 = EDGE_CURVE ( 'NONE', #28869, #16509, #30800, .T. ) ;
#10537 = VECTOR ( 'NONE', #14271, 1000.000000000000000 ) ;
#10538 = FACE_OUTER_BOUND ( 'NONE', #16439, .T. ) ;
#10539 = ORIENTED_EDGE ( 'NONE', *, *, #910, .F. ) ;
#10540 = ORIENTED_EDGE ( 'NONE', *, *, #3387, .F. ) ;
#10541 = ORIENTED_EDGE ( 'NONE', *, *, #23134, .T. ) ;
#10542 = AXIS2_PLACEMENT_3D ( 'NONE', #877, #10078, #24317 ) ;
#10543 = VECTOR ( 'NONE', #21838, 1000.000000000000000 ) ;
#10544 = EDGE_CURVE ( 'NONE', #25010, #25525, #23794, .T. ) ;
#10545 = VECTOR ( 'NONE', #6618, 1000.000000000000000 ) ;
#10546 = DIRECTION ( 'NONE',  ( 1.000000000000000000, 0.000000000000000000, 0.000000000000000000 ) ) ;
#10547 = CIRCLE ( 'NONE', #23720, 2.000000000000001776 ) ;
#10548 = VERTEX_POINT ( 'NONE', #20977 ) ;
#10549 = EDGE_CURVE ( 'NONE', #36402, #8583, #24223, .T. ) ;
#10550 = FACE_BOUND ( 'NONE', #5691, .T. ) ;
#10551 = ORIENTED_EDGE ( 'NONE', *, *, #9349, .T. ) ;
#10552 = ADVANCED_FACE ( 'NONE', ( #29574 ), #3899, .T. ) ;
#10553 = EDGE_LOOP ( 'NONE', ( #28351, #32027 ) ) ;
#10554 = CIRCLE ( 'NONE', #18937, 2.000000000000001776 ) ;
#10555 = DIRECTION ( 'NONE',  ( 1.000000000000000000, 0.000000000000000000, 0.000000000000000000 ) ) ;
#10556 = CARTESIAN_POINT ( 'NONE',  ( 17.14523346298344109, -93.36492675454773860, -49.86561046011506448 ) ) ;
#10557 = ORIENTED_EDGE ( 'NONE', *, *, #35957, .T. ) ;
#10558 = ORIENTED_EDGE ( 'NONE', *, *, #35657, .F. ) ;
#10559 = DIRECTION ( 'NONE',  ( 0.000000000000000000, 0.000000000000000000, 1.000000000000000000 ) ) ;
#10560 = CARTESIAN_POINT ( 'NONE',  ( 79.99999662536832545, -34.64101615137759183, -9.999999999999998224 ) ) ;
#10561 = EDGE_CURVE ( 'NONE', #31248, #10841, #11050, .T. ) ;
#10562 = CIRCLE ( 'NONE', #31499, 2.000000000000001776 ) ;
#10563 = DIRECTION ( 'NONE',  ( 0.000000000000000000, 0.000000000000000000, -1.000000000000000000 ) ) ;
#10564 = EDGE_CURVE ( 'NONE', #3670, #16140, #3295, .T. ) ;
#10565 = CARTESIAN_POINT ( 'NONE',  ( -10.00000337463127842, -69.28203230275519786, -9.999999999999998224 ) ) ;
#10566 = EDGE_CURVE ( 'NONE', #36232, #3839, #9877, .T. ) ;
#10567 = VECTOR ( 'NONE', #24417, 1000.000000000000000 ) ;
#10568 = ORIENTED_EDGE ( 'NONE', *, *, #28729, .F. ) ;
#10569 = DIRECTION ( 'NONE',  ( 1.000000000000000000, 0.000000000000000000, 0.000000000000000000 ) ) ;
#10570 = FACE_BOUND ( 'NONE', #4418, .T. ) ;
#10571 = CARTESIAN_POINT ( 'NONE',  ( 39.99999662536853151, -69.28203230275519786, -5.000000000000000000 ) ) ;
#10572 = DIRECTION ( 'NONE',  ( 1.000000000000000000, 0.000000000000000000, 0.000000000000000000 ) ) ;
#10573 = AXIS2_PLACEMENT_3D ( 'NONE', #19395, #16948, #22387 ) ;
#10574 = AXIS2_PLACEMENT_3D ( 'NONE', #27237, #35897, #29883 ) ;
#10575 = CARTESIAN_POINT ( 'NONE',  ( 44.13139720814401556, -27.50000000000022737, -10.00000000000000178 ) ) ;
#10576 = CARTESIAN_POINT ( 'NONE',  ( -3.500000000000000888, -55.00000000000000000, -15.00000000000000000 ) ) ;
#10577 = CIRCLE ( 'NONE', #14184, 2.000000000000001776 ) ;
#10578 = DIRECTION ( 'NONE',  ( 0.000000000000000000, 0.000000000000000000, 1.000000000000000000 ) ) ;
#10579 = DIRECTION ( 'NONE',  ( 0.000000000000000000, 0.000000000000000000, 1.000000000000000000 ) ) ;
#10580 = ORIENTED_EDGE ( 'NONE', *, *, #30354, .F. ) ;
#10581 = CARTESIAN_POINT ( 'NONE',  ( -5.000000000000000000, -0.9724665692850904541, -5.958069561147902427 ) ) ;
#10582 = CARTESIAN_POINT ( 'NONE',  ( -80.00000337463094979, 17.32050807568878525, -9.999999999999998224 ) ) ;
#10583 = CARTESIAN_POINT ( 'NONE',  ( -70.00000337463102085, -34.64101615137762025, -9.999999999999998224 ) ) ;
#10584 = ORIENTED_EDGE ( 'NONE', *, *, #29111, .T. ) ;
#10585 = AXIS2_PLACEMENT_3D ( 'NONE', #18810, #15445, #36065 ) ;
#10586 = EDGE_LOOP ( 'NONE', ( #12559, #28465 ) ) ;
#10587 = ADVANCED_FACE ( 'NONE', ( #27698 ), #27534, .F. ) ;
#10588 = ORIENTED_EDGE ( 'NONE', *, *, #26453, .F. ) ;
#10589 = CARTESIAN_POINT ( 'NONE',  ( 77.99999662536832545, -34.64101615137759183, -5.000000000000000000 ) ) ;
#10590 = CARTESIAN_POINT ( 'NONE',  ( -5.204170427930421283E-15, 5.773502691896269745, -0.5999999999999998668 ) ) ;
#10591 = EDGE_CURVE ( 'NONE', #19789, #22214, #30240, .T. ) ;
#10592 = VERTEX_POINT ( 'NONE', #7850 ) ;
#10593 = CIRCLE ( 'NONE', #26136, 2.000000000000001776 ) ;
#10594 = LINE ( 'NONE', #16951, #19699 ) ;
#10595 = AXIS2_PLACEMENT_3D ( 'NONE', #27717, #8234, #30900 ) ;
#10596 = CYLINDRICAL_SURFACE ( 'NONE', #36278, 95.00000000000001421 ) ;
#10597 = EDGE_LOOP ( 'NONE', ( #29312, #34213, #23452, #15789 ) ) ;
#10598 = CARTESIAN_POINT ( 'NONE',  ( -102.5304832720481869, 102.5304832720506596, 27.50000000000000000 ) ) ;
#10600 = EDGE_CURVE ( 'NONE', #35595, #14986, #31575, .T. ) ;
#10599 = ORIENTED_EDGE ( 'NONE', *, *, #1281, .F. ) ;
#10601 = DIRECTION ( 'NONE',  ( 0.000000000000000000, 0.000000000000000000, -1.000000000000000000 ) ) ;
#10602 = AXIS2_PLACEMENT_3D ( 'NONE', #4268, #18697, #1261 ) ;
#10603 = AXIS2_PLACEMENT_3D ( 'NONE', #24581, #23826, #26997 ) ;
#10604 = AXIS2_PLACEMENT_3D ( 'NONE', #9475, #32133, #35529 ) ;
#10605 = CARTESIAN_POINT ( 'NONE',  ( 1.301042606982605321E-15, 5.773502691896264416, -5.553418012614792509 ) ) ;
#10606 = CARTESIAN_POINT ( 'NONE',  ( 4.817220356105918810, -3.279784343982818040, -4.266919140436436386 ) ) ;
#10607 = DIRECTION ( 'NONE',  ( 0.000000000000000000, 0.000000000000000000, 1.000000000000000000 ) ) ;
#10608 = VERTEX_POINT ( 'NONE', #20145 ) ;
#10609 = DIRECTION ( 'NONE',  ( 0.000000000000000000, 0.000000000000000000, 1.000000000000000000 ) ) ;
#10610 = SHAPE_DEFINITION_REPRESENTATION ( #17857, #33474 ) ;
#10611 = CIRCLE ( 'NONE', #34576, 2.000000000000001776 ) ;
#10612 = DIRECTION ( 'NONE',  ( -1.000000000000000000, 0.000000000000000000, 0.000000000000000000 ) ) ;
#10613 = ADVANCED_FACE ( 'NONE', ( #4854 ), #13442, .F. ) ;
#10614 = DIRECTION ( 'NONE',  ( 0.000000000000000000, 0.000000000000000000, 1.000000000000000000 ) ) ;
#10615 = EDGE_CURVE ( 'NONE', #36125, #35067, #6291, .T. ) ;
#10616 = ORIENTED_EDGE ( 'NONE', *, *, #15856, .T. ) ;
#10617 = DIRECTION ( 'NONE',  ( -0.000000000000000000, -0.000000000000000000, 1.000000000000000000 ) ) ;
#10618 = DIRECTION ( 'NONE',  ( 1.000000000000000000, 0.000000000000000000, 0.000000000000000000 ) ) ;
#10619 = EDGE_CURVE ( 'NONE', #25427, #31944, #32622, .T. ) ;
#10620 = ORIENTED_EDGE ( 'NONE', *, *, #34389, .F. ) ;
#10621 = DIRECTION ( 'NONE',  ( 1.000000000000000000, 0.000000000000000000, 0.000000000000000000 ) ) ;
#10622 = AXIS2_PLACEMENT_3D ( 'NONE', #10214, #15466, #21642 ) ;
#10623 = CARTESIAN_POINT ( 'NONE',  ( 19.13981058454793072, -60.93295298010985306, 12.49999999999999822 ) ) ;
#10624 = LINE ( 'NONE', #13245, #11759 ) ;
#10625 = CIRCLE ( 'NONE', #34547, 25.00000000000000000 ) ;
#10626 = ORIENTED_EDGE ( 'NONE', *, *, #7074, .F. ) ;
#10627 = CIRCLE ( 'NONE', #31561, 2.000000000000000000 ) ;
#10628 = ORIENTED_EDGE ( 'NONE', *, *, #12627, .T. ) ;
#10629 = CARTESIAN_POINT ( 'NONE',  ( -7.000003374631307729, 77.94228634059957983, 12.50000000000000000 ) ) ;
#10630 = DIRECTION ( 'NONE',  ( 0.000000000000000000, 0.000000000000000000, 1.000000000000000000 ) ) ;
#10631 = AXIS2_PLACEMENT_3D ( 'NONE', #24843, #13219, #7040 ) ;
#10632 = CARTESIAN_POINT ( 'NONE',  ( -73.00000337463097821, 8.660254037844374864, 17.49999999999999645 ) ) ;
#10633 = CIRCLE ( 'NONE', #31571, 3.000000000000002665 ) ;
#10634 = VERTEX_POINT ( 'NONE', #8704 ) ;
#10635 = VERTEX_POINT ( 'NONE', #36347 ) ;
#10636 = CARTESIAN_POINT ( 'NONE',  ( 5.000000000000007994, -2.886751345948139758, -0.5999999999999998668 ) ) ;
#10637 = CARTESIAN_POINT ( 'NONE',  ( -4.088737910769898676, 3.412868758467427988, -1.160540885688320589 ) ) ;
#10638 =( REPRESENTATION_RELATIONSHIP ('NONE','NONE', #15268, #33015 ) REPRESENTATION_RELATIONSHIP_WITH_TRANSFORMATION ( #11152 )SHAPE_REPRESENTATION_RELATIONSHIP( ) );
#10639 = CARTESIAN_POINT ( 'NONE',  ( -73.90204618161054384, 6.988581222280664917, 12.50000000000000000 ) ) ;
#10640 = AXIS2_PLACEMENT_3D ( 'NONE', #26556, #20203, #5968 ) ;
#10641 = CARTESIAN_POINT ( 'NONE',  ( -81.11590899555835676, 72.50427799314736887, 32.49999999999999289 ) ) ;
#10642 = EDGE_CURVE ( 'NONE', #23924, #18775, #16467, .T. ) ;
#10643 = VERTEX_POINT ( 'NONE', #8014 ) ;
#10644 = ORIENTED_EDGE ( 'NONE', *, *, #11713, .F. ) ;
#10645 = CARTESIAN_POINT ( 'NONE',  ( 5.000000000000000000, 2.424500739214353384, -0.4207179063848189293 ) ) ;
#10646 = AXIS2_PLACEMENT_3D ( 'NONE', #15058, #32305, #18226 ) ;
#10647 = DIRECTION ( 'NONE',  ( 0.000000000000000000, 0.000000000000000000, 1.000000000000000000 ) ) ;
#10648 = VERTEX_POINT ( 'NONE', #1845 ) ;
#10649 = CARTESIAN_POINT ( 'NONE',  ( 64.99999662536839651, -43.30127018922199511, 12.50000000000000000 ) ) ;
#10650 = ORIENTED_EDGE ( 'NONE', *, *, #27726, .T. ) ;
#10651 = CIRCLE ( 'NONE', #16060, 1.999999999999998224 ) ;
#10652 = CIRCLE ( 'NONE', #31588, 95.00000000000000000 ) ;
#10653 = DIRECTION ( 'NONE',  ( 1.000000000000000000, 0.000000000000000000, 0.000000000000000000 ) ) ;
#10654 = CIRCLE ( 'NONE', #22027, 2.000000000000001776 ) ;
#10655 = AXIS2_PLACEMENT_3D ( 'NONE', #13166, #27209, #19179 ) ;
#10656 = FACE_OUTER_BOUND ( 'NONE', #13476, .T. ) ;
#10657 = CARTESIAN_POINT ( 'NONE',  ( -75.00000337463097821, -8.660254037844422825, 12.50000000000000000 ) ) ;
#10658 = ORIENTED_EDGE ( 'NONE', *, *, #2747, .F. ) ;
#10659 = DIRECTION ( 'NONE',  ( 0.000000000000000000, 0.000000000000000000, 1.000000000000000000 ) ) ;
#10660 = AXIS2_PLACEMENT_3D ( 'NONE', #30725, #7878, #18935 ) ;
#10661 = CARTESIAN_POINT ( 'NONE',  ( -62.00000337463104927, 34.64101615137757051, -9.999999999999998224 ) ) ;
#10662 = DIRECTION ( 'NONE',  ( 1.000000000000000000, 0.000000000000000000, 0.000000000000000000 ) ) ;
#10663 = ADVANCED_FACE ( 'NONE', ( #22098 ), #31051, .F. ) ;
#10664 = ORIENTED_EDGE ( 'NONE', *, *, #15903, .T. ) ;
#10665 = DIRECTION ( 'NONE',  ( 0.000000000000000000, 0.000000000000000000, -1.000000000000000000 ) ) ;
#10666 = CARTESIAN_POINT ( 'NONE',  ( 62.99999662536841072, -25.98076211353320275, -9.999999999999998224 ) ) ;
#10667 = CIRCLE ( 'NONE', #14246, 2.000000000000000000 ) ;
#10668 = DIRECTION ( 'NONE',  ( 1.000000000000000000, 0.000000000000000000, 0.000000000000000000 ) ) ;
#10669 = EDGE_LOOP ( 'NONE', ( #7173, #16253, #33902, #33467 ) ) ;
#10670 = EDGE_LOOP ( 'NONE', ( #13191, #35125 ) ) ;
#10671 = VERTEX_POINT ( 'NONE', #11514 ) ;
#10672 = AXIS2_PLACEMENT_3D ( 'NONE', #15961, #6958, #12945 ) ;
#10673 = CARTESIAN_POINT ( 'NONE',  ( 3.368272016354702636, 101.4480229402710592, 32.49999999999999289 ) ) ;
#10674 = EDGE_LOOP ( 'NONE', ( #19878, #31690 ) ) ;
#10675 = AXIS2_PLACEMENT_3D ( 'NONE', #16042, #7591, #19588 ) ;
#10676 = DIRECTION ( 'NONE',  ( -1.000000000000000000, 1.224646799147350989E-16, 0.000000000000000000 ) ) ;
#10677 = LINE ( 'NONE', #34114, #1594 ) ;
#10678 = FACE_OUTER_BOUND ( 'NONE', #36048, .T. ) ;
#10679 = CIRCLE ( 'NONE', #23849, 2.000000000000001776 ) ;
#10680 = CARTESIAN_POINT ( 'NONE',  ( 57.99999662536843914, -34.64101615137759893, -9.999999999999998224 ) ) ;
#10681 = CARTESIAN_POINT ( 'NONE',  ( 92.89190886694493088, -70.24536753140540668, 32.50000000000000000 ) ) ;
#10682 = FACE_OUTER_BOUND ( 'NONE', #32593, .T. ) ;
#10683 = CARTESIAN_POINT ( 'NONE',  ( 69.99999662536839651, 17.32050807568879236, 12.50000000000000000 ) ) ;
#10684 = ADVANCED_FACE ( 'NONE', ( #22961 ), #30333, .F. ) ;
#10685 = DIRECTION ( 'NONE',  ( 1.000000000000000000, 0.000000000000000000, 0.000000000000000000 ) ) ;
#10686 = ORIENTED_EDGE ( 'NONE', *, *, #2290, .T. ) ;
#10687 =( BOUNDED_CURVE ( )  B_SPLINE_CURVE ( 3, ( #20613, #3585, #576, #750 ),
 .UNSPECIFIED., .F., .T. ) 
 B_SPLINE_CURVE_WITH_KNOTS ( ( 4, 4 ),
 ( 4.712388980384679016, 6.283185307179586232 ),
 .UNSPECIFIED. ) 
 CURVE ( )  GEOMETRIC_REPRESENTATION_ITEM ( )  RATIONAL_B_SPLINE_CURVE ( ( 1.000000000000000000, 0.8047378541243626060, 0.8047378541243626060, 1.000000000000000000 ) ) 
 REPRESENTATION_ITEM ( '' )  );
#10688 = ORIENTED_EDGE ( 'NONE', *, *, #6728, .F. ) ;
#10689 = AXIS2_PLACEMENT_3D ( 'NONE', #30444, #4772, #27624 ) ;
#10690 = CARTESIAN_POINT ( 'NONE',  ( 44.99999662536851019, 77.94228634059959404, -9.999999999999998224 ) ) ;
#10691 = CARTESIAN_POINT ( 'NONE',  ( -56.67878100130369035, 27.78182860042797131, 12.49999999999999822 ) ) ;
#10692 = LINE ( 'NONE', #15942, #3688 ) ;
#10693 = DIRECTION ( 'NONE',  ( -1.000000000000000000, 0.000000000000000000, 0.000000000000000000 ) ) ;
#10694 = EDGE_LOOP ( 'NONE', ( #4792, #1269, #32589, #22688, #11786 ) ) ;
#10695 = UNCERTAINTY_MEASURE_WITH_UNIT (LENGTH_MEASURE( 1.000000000000000082E-05 ), #4291, 'distance_accuracy_value', 'NONE');
#10696 = CIRCLE ( 'NONE', #29844, 2.000000000000001776 ) ;
#10697 = CARTESIAN_POINT ( 'NONE',  ( 32.99999662536855283, -60.62177826491080168, 17.49999999999999645 ) ) ;
#10698 = ADVANCED_FACE ( 'NONE', ( #6807 ), #18242, .F. ) ;
#10699 = DIRECTION ( 'NONE',  ( -0.000000000000000000, -0.000000000000000000, 1.000000000000000000 ) ) ;
#10700 = CIRCLE ( 'NONE', #31641, 3.000000000000004885 ) ;
#10701 = EDGE_LOOP ( 'NONE', ( #29239, #28918, #18844, #2588 ) ) ;
#10702 = AXIS2_PLACEMENT_3D ( 'NONE', #8943, #14556, #20377 ) ;
#10703 = DIRECTION ( 'NONE',  ( 1.000000000000000000, 0.000000000000000000, 0.000000000000000000 ) ) ;
#10704 = VERTEX_POINT ( 'NONE', #1008 ) ;
#10705 = SURFACE_SIDE_STYLE ('',( #13492 ) ) ;
#10706 = DIRECTION ( 'NONE',  ( 0.000000000000000000, 0.000000000000000000, 1.000000000000000000 ) ) ;
#10707 = DIRECTION ( 'NONE',  ( 0.000000000000000000, 0.000000000000000000, 1.000000000000000000 ) ) ;
#10708 = CARTESIAN_POINT ( 'NONE',  ( -149.8799519615615736, 6.000000000001555200, 27.50000000000000000 ) ) ;
#10709 = EDGE_CURVE ( 'NONE', #1395, #21235, #289, .T. ) ;
#10710 = ORIENTED_EDGE ( 'NONE', *, *, #15734, .T. ) ;
#10711 = ORIENTED_EDGE ( 'NONE', *, *, #18929, .T. ) ;
#10712 = CIRCLE ( 'NONE', #28078, 2.000000000000001776 ) ;
#10713 = AXIS2_PLACEMENT_3D ( 'NONE', #5328, #10924, #50 ) ;
#10714 = ORIENTED_EDGE ( 'NONE', *, *, #1746, .T. ) ;
#10715 = CARTESIAN_POINT ( 'NONE',  ( 145.0000000000000853, 5.999999999999493738, 32.55002500000000509 ) ) ;
#10716 = DIRECTION ( 'NONE',  ( 1.000000000000000000, 0.000000000000000000, 0.000000000000000000 ) ) ;
#10717 = CARTESIAN_POINT ( 'NONE',  ( 36.99999662536853862, 77.94228634059959404, 17.49999999999999645 ) ) ;
#10718 = DIRECTION ( 'NONE',  ( 0.000000000000000000, 0.000000000000000000, 1.000000000000000000 ) ) ;
#10719 = FACE_OUTER_BOUND ( 'NONE', #24229, .T. ) ;
#10720 = EDGE_LOOP ( 'NONE', ( #15586, #21992 ) ) ;
#10721 = LINE ( 'NONE', #34162, #11727 ) ;
#10722 = EDGE_CURVE ( 'NONE', #34855, #20688, #3645, .T. ) ;
#10723 = CYLINDRICAL_SURFACE ( 'NONE', #28771, 2.000000000000001776 ) ;
#10724 = CIRCLE ( 'NONE', #8925, 2.000000000000001776 ) ;
#10725 = ADVANCED_FACE ( 'NONE', ( #6084 ), #31919, .T. ) ;
#10726 = DIRECTION ( 'NONE',  ( 0.000000000000000000, 0.000000000000000000, -1.000000000000000000 ) ) ;
#10727 = ORIENTED_EDGE ( 'NONE', *, *, #13, .F. ) ;
#10728 = DIRECTION ( 'NONE',  ( 0.000000000000000000, 0.000000000000000000, 1.000000000000000000 ) ) ;
#10729 = AXIS2_PLACEMENT_3D ( 'NONE', #23427, #18354, #9906 ) ;
#10730 = DIRECTION ( 'NONE',  ( -1.000000000000000000, -0.000000000000000000, -0.000000000000000000 ) ) ;
#10731 = ORIENTED_EDGE ( 'NONE', *, *, #22046, .T. ) ;
#10732 = EDGE_CURVE ( 'NONE', #29318, #22484, #30825, .T. ) ;
#10733 = VERTEX_POINT ( 'NONE', #23144 ) ;
#10734 = DIRECTION ( 'NONE',  ( 1.000000000000000000, 0.000000000000000000, 0.000000000000000000 ) ) ;
#10735 = CIRCLE ( 'NONE', #17318, 27.00000000000001421 ) ;
#10736 = LINE ( 'NONE', #19350, #34883 ) ;
#10737 = DIRECTION ( 'NONE',  ( 1.000000000000000000, 0.000000000000000000, 0.000000000000000000 ) ) ;
#10738 = CARTESIAN_POINT ( 'NONE',  ( -5.000000000000000000, -2.886751345948134428, -2.080000000000000071 ) ) ;
#10739 = EDGE_CURVE ( 'NONE', #19789, #28708, #21063, .T. ) ;
#10740 = EDGE_LOOP ( 'NONE', ( #30846, #10295 ) ) ;
#10741 = EDGE_LOOP ( 'NONE', ( #6185, #29782, #5796, #7671 ) ) ;
#10742 = CARTESIAN_POINT ( 'NONE',  ( -12.00000337463127842, -69.28203230275519786, -9.999999999999998224 ) ) ;
#10743 = VECTOR ( 'NONE', #2406, 1000.000000000000000 ) ;
#10744 = EDGE_CURVE ( 'NONE', #25550, #30229, #35641, .T. ) ;
#10745 = EDGE_LOOP ( 'NONE', ( #25544, #13582, #36950 ) ) ;
#10746 = AXIS2_PLACEMENT_3D ( 'NONE', #30550, #5233, #33159 ) ;
#10747 = CARTESIAN_POINT ( 'NONE',  ( -56.67878100130369035, 27.78182860042797131, -4.999999999999997335 ) ) ;
#10748 = VERTEX_POINT ( 'NONE', #815 ) ;
#10749 = ORIENTED_EDGE ( 'NONE', *, *, #3301, .F. ) ;
#10750 = CIRCLE ( 'NONE', #7754, 3.000000000000002665 ) ;
#10751 = DIRECTION ( 'NONE',  ( 0.000000000000000000, 0.000000000000000000, -1.000000000000000000 ) ) ;
#10752 = VECTOR ( 'NONE', #31967, 1000.000000000000000 ) ;
#10753 = PLANE ( 'NONE',  #19663 ) ;
#10754 = EDGE_LOOP ( 'NONE', ( #30911, #4849, #31524, #4252 ) ) ;
#10755 = VERTEX_POINT ( 'NONE', #12223 ) ;
#10756 = DIRECTION ( 'NONE',  ( 1.000000000000000000, 0.000000000000000000, 0.000000000000000000 ) ) ;
#10757 = CIRCLE ( 'NONE', #28705, 33.00000000000001421 ) ;
#10758 = CARTESIAN_POINT ( 'NONE',  ( 6.000000000000000000, -149.8799519615616305, 32.55002500000000509 ) ) ;
#10759 = DIRECTION ( 'NONE',  ( 0.000000000000000000, 0.000000000000000000, -1.000000000000000000 ) ) ;
#10760 = DIRECTION ( 'NONE',  ( 1.000000000000000000, 0.000000000000000000, 0.000000000000000000 ) ) ;
#10761 = ADVANCED_FACE ( 'NONE', ( #14895 ), #643, .T. ) ;
#10762 = EDGE_LOOP ( 'NONE', ( #22896, #16590 ) ) ;
#10763 = FACE_OUTER_BOUND ( 'NONE', #23840, .T. ) ;
#10764 = FACE_BOUND ( 'NONE', #4723, .T. ) ;
#10765 = CARTESIAN_POINT ( 'NONE',  ( -32.00000337463118427, 69.28203230275516944, -9.999999999999998224 ) ) ;
#10766 = FACE_BOUND ( 'NONE', #11368, .T. ) ;
#10767 = FACE_OUTER_BOUND ( 'NONE', #14917, .T. ) ;
#10768 = CARTESIAN_POINT ( 'NONE',  ( 5.236872748402765509, -0.5081686017868810579, -4.057689166958444282 ) ) ;
#10769 = ADVANCED_FACE ( 'NONE', ( #23697 ), #35149, .T. ) ;
#10770 = CIRCLE ( 'NONE', #35911, 2.000000000000001776 ) ;
#10771 = DIRECTION ( 'NONE',  ( -1.000000000000000000, 0.000000000000000000, 0.000000000000000000 ) ) ;
#10772 = EDGE_CURVE ( 'NONE', #2346, #35442, #35040, .T. ) ;
#10773 = DIRECTION ( 'NONE',  ( 1.000000000000000000, 0.000000000000000000, 0.000000000000000000 ) ) ;
#10774 = EDGE_LOOP ( 'NONE', ( #10315, #1035, #4636 ) ) ;
#10775 = CARTESIAN_POINT ( 'NONE',  ( -82.00000337463094979, 17.32050807568878525, 12.50000000000000000 ) ) ;
#10776 = CARTESIAN_POINT ( 'NONE',  ( -77.00000337463097821, 25.98076211353318854, -9.999999999999998224 ) ) ;
#10777 = AXIS2_PLACEMENT_3D ( 'NONE', #29841, #35483, #35310 ) ;
#10778 = DIRECTION ( 'NONE',  ( 1.000000000000000000, 0.000000000000000000, 0.000000000000000000 ) ) ;
#10779 = ORIENTED_EDGE ( 'NONE', *, *, #15148, .T. ) ;
#10780 = ORIENTED_EDGE ( 'NONE', *, *, #24704, .T. ) ;
#10781 = VERTEX_POINT ( 'NONE', #20889 ) ;
#10782 = AXIS2_PLACEMENT_3D ( 'NONE', #24869, #2542, #33676 ) ;
#10783 = CARTESIAN_POINT ( 'NONE',  ( 24.99999662536859546, -77.94228634059960825, -9.999999999999998224 ) ) ;
#10784 = DIRECTION ( 'NONE',  ( 1.000000000000000000, 0.000000000000000000, 0.000000000000000000 ) ) ;
#10785 = AXIS2_PLACEMENT_3D ( 'NONE', #30538, #18727, #22104 ) ;
#10786 = ORIENTED_EDGE ( 'NONE', *, *, #31871, .F. ) ;
#10787 = DIRECTION ( 'NONE',  ( -1.000000000000000000, 0.000000000000000000, 0.000000000000000000 ) ) ;
#10788 = ADVANCED_FACE ( 'NONE', ( #23513 ), #32116, .F. ) ;
#10789 = DIRECTION ( 'NONE',  ( 0.000000000000000000, 0.000000000000000000, 1.000000000000000000 ) ) ;
#10790 = ORIENTED_EDGE ( 'NONE', *, *, #31373, .T. ) ;
#10791 = DIRECTION ( 'NONE',  ( 1.000000000000000000, 0.000000000000000000, 0.000000000000000000 ) ) ;
#10792 = EDGE_LOOP ( 'NONE', ( #3731, #30810, #31638, #22259 ) ) ;
#10793 = CYLINDRICAL_SURFACE ( 'NONE', #19555, 45.00000000000000711 ) ;
#10794 = DIRECTION ( 'NONE',  ( 0.000000000000000000, 0.000000000000000000, 1.000000000000000000 ) ) ;
#10795 = CARTESIAN_POINT ( 'NONE',  ( -12.00000337463128197, 86.60254037844397601, -9.999999999999998224 ) ) ;
#10796 = CIRCLE ( 'NONE', #3593, 2.000000000000001776 ) ;
#10797 = ORIENTED_EDGE ( 'NONE', *, *, #28990, .T. ) ;
#10798 = DIRECTION ( 'NONE',  ( -1.000000000000000000, 0.000000000000000000, 0.000000000000000000 ) ) ;
#10799 = AXIS2_PLACEMENT_3D ( 'NONE', #31486, #14266, #34703 ) ;
#10800 = CARTESIAN_POINT ( 'NONE',  ( 111.8061974404897825, -19.22934205795014151, 32.50000000000000000 ) ) ;
#10801 = DIRECTION ( 'NONE',  ( 0.000000000000000000, 0.000000000000000000, 1.000000000000000000 ) ) ;
#10802 = EDGE_CURVE ( 'NONE', #8343, #36432, #22456, .T. ) ;
#10803 = CIRCLE ( 'NONE', #3017, 2.000000000000000000 ) ;
#10804 = EDGE_LOOP ( 'NONE', ( #5177, #87 ) ) ;
#10805 = CARTESIAN_POINT ( 'NONE',  ( 3.000000000000000000, 0.000000000000000000, 0.000000000000000000 ) ) ;
#10806 = DIRECTION ( 'NONE',  ( 1.000000000000000000, 0.000000000000000000, 0.000000000000000000 ) ) ;
#10807 = VERTEX_POINT ( 'NONE', #34598 ) ;
#10808 = EDGE_CURVE ( 'NONE', #6666, #22417, #32008, .T. ) ;
#10809 = FACE_OUTER_BOUND ( 'NONE', #11245, .T. ) ;
#10810 = FACE_OUTER_BOUND ( 'NONE', #3363, .T. ) ;
#10811 = DIRECTION ( 'NONE',  ( 0.000000000000000000, 0.000000000000000000, -1.000000000000000000 ) ) ;
#10812 = CARTESIAN_POINT ( 'NONE',  ( -5.999999999999985789, -149.8799519615616305, 27.50000000000000000 ) ) ;
#10813 = EDGE_CURVE ( 'NONE', #13352, #7527, #9249, .T. ) ;
#10814 = EDGE_LOOP ( 'NONE', ( #4525, #10875 ) ) ;
#10815 = EDGE_LOOP ( 'NONE', ( #1257, #7931 ) ) ;
#10816 = EDGE_CURVE ( 'NONE', #31233, #5893, #31757, .T. ) ;
#10817 = DIRECTION ( 'NONE',  ( -0.000000000000000000, 0.000000000000000000, -1.000000000000000000 ) ) ;
#10818 = DIRECTION ( 'NONE',  ( 0.000000000000000000, 0.000000000000000000, -1.000000000000000000 ) ) ;
#10819 = EDGE_CURVE ( 'NONE', #33663, #5095, #36256, .T. ) ;
#10820 = DIRECTION ( 'NONE',  ( 0.000000000000000000, 0.000000000000000000, 1.000000000000000000 ) ) ;
#10821 = EDGE_LOOP ( 'NONE', ( #36685, #16428, #11054, #21144 ) ) ;
#10822 = VERTEX_POINT ( 'NONE', #7757 ) ;
#10823 = CIRCLE ( 'NONE', #32361, 2.000000000000001776 ) ;
#10824 = CARTESIAN_POINT ( 'NONE',  ( 3.000000000000000000, 2.935248768560057453, -3.903127820947815962E-15 ) ) ;
#10825 = CARTESIAN_POINT ( 'NONE',  ( -5.000000000000000000, 2.886751345948126879, -2.079999999999992077 ) ) ;
#10826 = DIRECTION ( 'NONE',  ( 0.000000000000000000, 0.000000000000000000, -1.000000000000000000 ) ) ;
#10827 = EDGE_CURVE ( 'NONE', #2100, #33319, #24814, .T. ) ;
#10828 = VERTEX_POINT ( 'NONE', #1370 ) ;
#10830 = ORIENTED_EDGE ( 'NONE', *, *, #2572, .F. ) ;
#10829 = EDGE_CURVE ( 'NONE', #23537, #30130, #33443, .T. ) ;
#10831 = CARTESIAN_POINT ( 'NONE',  ( 56.67878100130369035, -27.78182860042797131, -4.999999999999997335 ) ) ;
#10832 = ADVANCED_FACE ( 'NONE', ( #36247 ), #35696, .F. ) ;
#10833 = DIRECTION ( 'NONE',  ( 0.000000000000000000, 0.000000000000000000, -1.000000000000000000 ) ) ;
#10835 = EDGE_CURVE ( 'NONE', #4001, #10128, #15809, .T. ) ;
#10834 = ORIENTED_EDGE ( 'NONE', *, *, #24175, .T. ) ;
#10836 = FACE_OUTER_BOUND ( 'NONE', #29415, .T. ) ;
#10837 = ORIENTED_EDGE ( 'NONE', *, *, #16106, .F. ) ;
#10838 = FACE_BOUND ( 'NONE', #11862, .T. ) ;
#10839 = DIRECTION ( 'NONE',  ( 1.000000000000000000, 0.000000000000000000, 0.000000000000000000 ) ) ;
#10840 = DIRECTION ( 'NONE',  ( 1.000000000000000000, 0.000000000000000000, 0.000000000000000000 ) ) ;
#10841 = VERTEX_POINT ( 'NONE', #4569 ) ;
#10842 = DIRECTION ( 'NONE',  ( 0.000000000000000000, 0.000000000000000000, 1.000000000000000000 ) ) ;
#10843 = DIRECTION ( 'NONE',  ( -0.000000000000000000, -0.000000000000000000, 1.000000000000000000 ) ) ;
#10844 = DIRECTION ( 'NONE',  ( -1.000000000000000000, 0.000000000000000000, 0.000000000000000000 ) ) ;
#10845 = LINE ( 'NONE', #5022, #27474 ) ;
#10846 = CIRCLE ( 'NONE', #34782, 2.000000000000001776 ) ;
#10847 = ORIENTED_EDGE ( 'NONE', *, *, #19162, .F. ) ;
#10848 = CARTESIAN_POINT ( 'NONE',  ( 81.99999662536833966, -3.469446951953614189E-15, 12.50000000000000000 ) ) ;
#10849 = DIRECTION ( 'NONE',  ( 1.000000000000000000, 0.000000000000000000, 0.000000000000000000 ) ) ;
#10850 = DIRECTION ( 'NONE',  ( 1.000000000000000000, 0.000000000000000000, 0.000000000000000000 ) ) ;
#10851 = VERTEX_POINT ( 'NONE', #21998 ) ;
#10852 = VERTEX_POINT ( 'NONE', #1928 ) ;
#10853 = DIRECTION ( 'NONE',  ( 0.000000000000000000, 0.000000000000000000, 1.000000000000000000 ) ) ;
#10854 = ORIENTED_EDGE ( 'NONE', *, *, #5041, .F. ) ;
#10855 = LINE ( 'NONE', #19667, #22333 ) ;
#10856 = DIRECTION ( 'NONE',  ( 0.000000000000000000, 0.000000000000000000, 1.000000000000000000 ) ) ;
#10857 = CARTESIAN_POINT ( 'NONE',  ( -70.00000337463100664, -17.32050807568882078, -5.000000000000000000 ) ) ;
#10858 = CARTESIAN_POINT ( 'NONE',  ( -2.500000000000006217, -4.330127018922186544, 0.000000000000000000 ) ) ;
#10859 = CARTESIAN_POINT ( 'NONE',  ( 106.8646913500057707, -42.81758297416944004, 32.50000000000000000 ) ) ;
#10860 = CARTESIAN_POINT ( 'NONE',  ( -78.38327399104142046, -72.20004170604832439, 32.50000000000000711 ) ) ;
#10861 = AXIS2_PLACEMENT_3D ( 'NONE', #8249, #13861, #32157 ) ;
#10862 = LINE ( 'NONE', #36733, #30993 ) ;
#10863 = DIRECTION ( 'NONE',  ( 0.000000000000000000, 0.000000000000000000, 1.000000000000000000 ) ) ;
#10864 = ORIENTED_EDGE ( 'NONE', *, *, #25000, .T. ) ;
#10865 = ORIENTED_EDGE ( 'NONE', *, *, #3894, .F. ) ;
#10866 = DIRECTION ( 'NONE',  ( -1.000000000000000000, 0.000000000000000000, 0.000000000000000000 ) ) ;
#10867 = EDGE_CURVE ( 'NONE', #4612, #11022, #21871, .T. ) ;
#10868 = CARTESIAN_POINT ( 'NONE',  ( 79.99999662536832545, -34.64101615137759183, -5.000000000000000000 ) ) ;
#10869 = LINE ( 'NONE', #21579, #9528 ) ;
#10870 = ORIENTED_EDGE ( 'NONE', *, *, #35582, .F. ) ;
#10871 = CARTESIAN_POINT ( 'NONE',  ( 3.000000000000000000, 1.467624384280024730, -2.542000000000001592 ) ) ;
#10872 = ORIENTED_EDGE ( 'NONE', *, *, #12902, .F. ) ;
#10873 = ORIENTED_EDGE ( 'NONE', *, *, #4436, .T. ) ;
#10874 = CARTESIAN_POINT ( 'NONE',  ( 56.29165124598892334, 32.49999999999928235, 12.49999999999999822 ) ) ;
#10875 = ORIENTED_EDGE ( 'NONE', *, *, #17637, .T. ) ;
#10876 = DIRECTION ( 'NONE',  ( 1.000000000000000000, 0.000000000000000000, 0.000000000000000000 ) ) ;
#10877 = CARTESIAN_POINT ( 'NONE',  ( 94.40806000769313755, 12.15049814296589226, 32.50000000000000000 ) ) ;
#10878 = LINE ( 'NONE', #11252, #9495 ) ;
#10879 = ORIENTED_EDGE ( 'NONE', *, *, #2027, .F. ) ;
#10880 = EDGE_LOOP ( 'NONE', ( #15177, #28707, #8877, #22152 ) ) ;
#10881 = AXIS2_PLACEMENT_3D ( 'NONE', #6194, #23455, #29614 ) ;
#10882 = EDGE_CURVE ( 'NONE', #35287, #11413, #4006, .T. ) ;
#10883 = ORIENTED_EDGE ( 'NONE', *, *, #27259, .F. ) ;
#10884 = EDGE_CURVE ( 'NONE', #13905, #32112, #15450, .T. ) ;
#10885 = EDGE_LOOP ( 'NONE', ( #28736, #4372, #6622, #11267 ) ) ;
#10886 = CARTESIAN_POINT ( 'NONE',  ( -80.00000337463096400, -34.64101615137762025, -9.999999999999998224 ) ) ;
#10887 = DIRECTION ( 'NONE',  ( 0.000000000000000000, 0.000000000000000000, 1.000000000000000000 ) ) ;
#10888 = CARTESIAN_POINT ( 'NONE',  ( -70.00000337463102085, -34.64101615137762025, -5.000000000000000000 ) ) ;
#10889 = DIRECTION ( 'NONE',  ( 0.000000000000000000, 0.000000000000000000, 1.000000000000000000 ) ) ;
#10890 = LINE ( 'NONE', #5828, #3357 ) ;
#10891 = ORIENTED_EDGE ( 'NONE', *, *, #34214, .T. ) ;
#10892 = CARTESIAN_POINT ( 'NONE',  ( -3.050000000000000711, 3.735172737399428132E-16, 2.266666666666999674 ) ) ;
#10893 = FACE_OUTER_BOUND ( 'NONE', #23231, .T. ) ;
#10894 = ADVANCED_FACE ( 'NONE', ( #21631 ), #27618, .F. ) ;
#10895 = CARTESIAN_POINT ( 'NONE',  ( 6.249999999999998224, 0.000000000000000000, 0.000000000000000000 ) ) ;
#10896 = ORIENTED_EDGE ( 'NONE', *, *, #2626, .F. ) ;
#10897 = CARTESIAN_POINT ( 'NONE',  ( 0.000000000000000000, 0.000000000000000000, -5.700000000000001066 ) ) ;
#10898 = CARTESIAN_POINT ( 'NONE',  ( 9.999996625368625658, 86.60254037844397601, 12.50000000000000000 ) ) ;
#10899 = ORIENTED_EDGE ( 'NONE', *, *, #11380, .T. ) ;
#10900 = ORIENTED_EDGE ( 'NONE', *, *, #21083, .F. ) ;
#10901 = DIRECTION ( 'NONE',  ( -0.000000000000000000, 0.000000000000000000, -1.000000000000000000 ) ) ;
#10902 = AXIS2_PLACEMENT_3D ( 'NONE', #9044, #3971, #9608 ) ;
#10903 = CARTESIAN_POINT ( 'NONE',  ( -4.400655246573244916, 3.515428273944189552, -4.176900509772079495 ) ) ;
#10904 = ADVANCED_FACE ( 'NONE', ( #4765 ), #12619, .F. ) ;
#10905 = CARTESIAN_POINT ( 'NONE',  ( 3.514986608498837484, -4.017641317389694322, -4.057689166958486915 ) ) ;
#10906 = CARTESIAN_POINT ( 'NONE',  ( -2.285412292771023424, -4.454019289455668940, -2.909304063934346637E-14 ) ) ;
#10907 = ORIENTED_EDGE ( 'NONE', *, *, #23248, .F. ) ;
#10908 = ORIENTED_EDGE ( 'NONE', *, *, #26107, .T. ) ;
#10909 = DIRECTION ( 'NONE',  ( 0.000000000000000000, 0.000000000000000000, 1.000000000000000000 ) ) ;
#10910 = ORIENTED_EDGE ( 'NONE', *, *, #5860, .T. ) ;
#10911 = DIRECTION ( 'NONE',  ( 1.000000000000000000, 0.000000000000000000, 0.000000000000000000 ) ) ;
#10912 = ORIENTED_EDGE ( 'NONE', *, *, #30515, .T. ) ;
#10913 = ORIENTED_EDGE ( 'NONE', *, *, #1881, .F. ) ;
#10914 = VECTOR ( 'NONE', #30012, 1000.000000000000000 ) ;
#10915 = AXIS2_PLACEMENT_3D ( 'NONE', #22528, #16904, #5644 ) ;
#10916 = CARTESIAN_POINT ( 'NONE',  ( 54.99999662536844625, 43.30127018922198801, -5.000000000000000000 ) ) ;
#10917 = EDGE_CURVE ( 'NONE', #28376, #29465, #24881, .T. ) ;
#10918 = DIRECTION ( 'NONE',  ( 0.000000000000000000, 0.000000000000000000, -1.000000000000000000 ) ) ;
#10919 = VERTEX_POINT ( 'NONE', #24072 ) ;
#10920 = VERTEX_POINT ( 'NONE', #35514 ) ;
#10921 = CARTESIAN_POINT ( 'NONE',  ( -37.00000337463116296, -60.62177826491080168, -9.999999999999998224 ) ) ;
#10922 = LINE ( 'NONE', #7762, #36905 ) ;
#10923 = CARTESIAN_POINT ( 'NONE',  ( -58.00000337463108480, -51.96152422706641971, -5.000000000000000000 ) ) ;
#10924 = DIRECTION ( 'NONE',  ( 0.000000000000000000, 0.000000000000000000, 1.000000000000000000 ) ) ;
#10925 = EDGE_LOOP ( 'NONE', ( #24624, #5894 ) ) ;
#10926 = DIRECTION ( 'NONE',  ( 0.000000000000000000, 0.000000000000000000, 1.000000000000000000 ) ) ;
#10927 = PRODUCT_DEFINITION ( 'UNKNOWN', '', #36327, #27575 ) ;
#10928 = AXIS2_PLACEMENT_3D ( 'NONE', #21963, #30590, #4908 ) ;
#10929 = FACE_BOUND ( 'NONE', #13281, .T. ) ;
#10930 = EDGE_CURVE ( 'NONE', #14423, #3735, #18250, .T. ) ;
#10931 = CARTESIAN_POINT ( 'NONE',  ( -31.46585318596190106, -86.45172111230344569, -4.999999999999997335 ) ) ;
#10932 = FACE_OUTER_BOUND ( 'NONE', #1272, .T. ) ;
#10933 = DIRECTION ( 'NONE',  ( -1.000000000000000000, 0.000000000000000000, 0.000000000000000000 ) ) ;
#10934 = DIRECTION ( 'NONE',  ( -1.000000000000000000, 0.000000000000000000, 0.000000000000000000 ) ) ;
#10935 = CARTESIAN_POINT ( 'NONE',  ( 79.99999662536833966, 34.64101615137759183, -9.999999999999998224 ) ) ;
#10936 = ADVANCED_FACE ( 'NONE', ( #18639 ), #9807, .T. ) ;
#10937 = CARTESIAN_POINT ( 'NONE',  ( -70.00000337463100664, -17.32050807568882078, 17.49999999999999645 ) ) ;
#10938 = VERTEX_POINT ( 'NONE', #4209 ) ;
#10939 = DIRECTION ( 'NONE',  ( 0.000000000000000000, 0.000000000000000000, 1.000000000000000000 ) ) ;
#10940 = DIRECTION ( 'NONE',  ( 0.000000000000000000, 0.000000000000000000, 1.000000000000000000 ) ) ;
#10941 = FACE_OUTER_BOUND ( 'NONE', #9699, .T. ) ;
#10942 = ORIENTED_EDGE ( 'NONE', *, *, #28199, .T. ) ;
#10943 = CIRCLE ( 'NONE', #12719, 33.00000000000002132 ) ;
#10944 = ORIENTED_EDGE ( 'NONE', *, *, #32012, .T. ) ;
#10945 = ORIENTED_EDGE ( 'NONE', *, *, #20381, .T. ) ;
#10946 = CARTESIAN_POINT ( 'NONE',  ( -70.00000337463099243, 34.64101615137758472, 12.50000000000000000 ) ) ;
#10947 = DIRECTION ( 'NONE',  ( 1.000000000000000000, 0.000000000000000000, 0.000000000000000000 ) ) ;
#10948 = VERTEX_POINT ( 'NONE', #15636 ) ;
#10949 = DIRECTION ( 'NONE',  ( 0.000000000000000000, 0.000000000000000000, -1.000000000000000000 ) ) ;
#10950 = ADVANCED_FACE ( 'NONE', ( #24451 ), #10000, .F. ) ;
#10951 = CARTESIAN_POINT ( 'NONE',  ( 47.63139720814418610, 27.49999999999988987, -5.000000000000000888 ) ) ;
#10952 = VERTEX_POINT ( 'NONE', #27233 ) ;
#10953 = CIRCLE ( 'NONE', #31887, 2.000000000000001776 ) ;
#10954 = CARTESIAN_POINT ( 'NONE',  ( -81.86307664143558327, 18.04780306571548820, 12.50000000000000000 ) ) ;
#10955 = ORIENTED_EDGE ( 'NONE', *, *, #21145, .T. ) ;
#10956 = DIRECTION ( 'NONE',  ( 0.000000000000000000, 0.000000000000000000, -1.000000000000000000 ) ) ;
#10957 = EDGE_CURVE ( 'NONE', #18409, #36079, #34049, .T. ) ;
#10958 = FACE_OUTER_BOUND ( 'NONE', #16418, .T. ) ;
#10959 = CARTESIAN_POINT ( 'NONE',  ( 52.39915983220795681, 35.19434990244919703, -4.999999999999997335 ) ) ;
#10960 = ADVANCED_FACE ( 'NONE', ( #33058 ), #19557, .F. ) ;
#10961 = ORIENTED_EDGE ( 'NONE', *, *, #32538, .F. ) ;
#10962 = FACE_OUTER_BOUND ( 'NONE', #24810, .T. ) ;
#10963 = AXIS2_PLACEMENT_3D ( 'NONE', #22217, #27470, #10396 ) ;
#10964 = ITEM_DEFINED_TRANSFORMATION ( 'NONE', 'NONE', #18358,  #21385 ) ;
#10965 = DIRECTION ( 'NONE',  ( -1.000000000000000000, 1.082992363797667670E-14, 0.000000000000000000 ) ) ;
#10966 = CARTESIAN_POINT ( 'NONE',  ( -73.00000337463099243, -25.98076211353322051, -9.999999999999998224 ) ) ;
#10967 = AXIS2_PLACEMENT_3D ( 'NONE', #8430, #16690, #19859 ) ;
#10968 = ORIENTED_EDGE ( 'NONE', *, *, #71, .T. ) ;
#10969 = DIRECTION ( 'NONE',  ( -1.000000000000000000, 0.000000000000000000, 0.000000000000000000 ) ) ;
#10970 = DIRECTION ( 'NONE',  ( -1.000000000000000000, 0.000000000000000000, 0.000000000000000000 ) ) ;
#10971 = VERTEX_POINT ( 'NONE', #2493 ) ;
#10972 = CARTESIAN_POINT ( 'NONE',  ( 91.99999662536828282, 0.000000000000000000, 17.49999999999999645 ) ) ;
#10973 = CARTESIAN_POINT ( 'NONE',  ( -45.00000337463112743, -60.62177826491080168, 17.49999999999999645 ) ) ;
#10974 = DIRECTION ( 'NONE',  ( 0.000000000000000000, 0.000000000000000000, 1.000000000000000000 ) ) ;
#10975 = CYLINDRICAL_SURFACE ( 'NONE', #15274, 2.000000000000001776 ) ;
#10976 = ORIENTED_EDGE ( 'NONE', *, *, #25814, .T. ) ;
#10977 = EDGE_CURVE ( 'NONE', #21860, #27057, #27987, .T. ) ;
#10978 = VECTOR ( 'NONE', #12766, 1000.000000000000000 ) ;
#10979 = ORIENTED_EDGE ( 'NONE', *, *, #27181, .F. ) ;
#10980 = CARTESIAN_POINT ( 'NONE',  ( 64.99999662536839651, 60.62177826491078747, -9.999999999999998224 ) ) ;
#10981 = CARTESIAN_POINT ( 'NONE',  ( -62.00000337463104927, 34.64101615137757051, 17.49999999999999645 ) ) ;
#10982 = VERTEX_POINT ( 'NONE', #25198 ) ;
#10983 = ORIENTED_EDGE ( 'NONE', *, *, #11948, .F. ) ;
#10984 = DIRECTION ( 'NONE',  ( 0.000000000000000000, 0.000000000000000000, 1.000000000000000000 ) ) ;
#10985 = CARTESIAN_POINT ( 'NONE',  ( -37.50000000000000000, 103.4105893997321886, 27.49999999999999645 ) ) ;
#10986 = DIRECTION ( 'NONE',  ( 0.000000000000000000, 0.000000000000000000, 1.000000000000000000 ) ) ;
#10987 = CIRCLE ( 'NONE', #31922, 2.541999999999999815 ) ;
#10988 = EDGE_LOOP ( 'NONE', ( #24205, #31700 ) ) ;
#10989 = EDGE_LOOP ( 'NONE', ( #24792, #8922, #8827, #29600, #5442, #10908, #3742, #19947, #16552, #5685, #17826, #13386, #22607, #23115, #23947, #2896, #7205, #6444, #23096, #34545, #6301, #21013, #1177, #24295 ) ) ;
#10990 = CIRCLE ( 'NONE', #34960, 27.00000000000001066 ) ;
#10991 = DIRECTION ( 'NONE',  ( -0.000000000000000000, -0.000000000000000000, -1.000000000000000000 ) ) ;
#10992 = ADVANCED_FACE ( 'NONE', ( #36624 ), #10753, .F. ) ;
#10993 = CYLINDRICAL_SURFACE ( 'NONE', #17096, 2.000000000000001776 ) ;
#10994 = ORIENTED_EDGE ( 'NONE', *, *, #27526, .T. ) ;
#10995 = EDGE_CURVE ( 'NONE', #11751, #27540, #31034, .T. ) ;
#10996 = CARTESIAN_POINT ( 'NONE',  ( -8.000003374631281972, 86.60254037844397601, 12.50000000000000000 ) ) ;
#10997 = VERTEX_POINT ( 'NONE', #34190 ) ;
#10998 = FACE_BOUND ( 'NONE', #20947, .T. ) ;
#10999 = VECTOR ( 'NONE', #14845, 1000.000000000000000 ) ;
#11000 = EDGE_CURVE ( 'NONE', #27568, #11237, #17860, .T. ) ;
#11001 = CARTESIAN_POINT ( 'NONE',  ( 84.99999662536831124, -25.98076211353319565, 12.50000000000000000 ) ) ;
#11002 = CIRCLE ( 'NONE', #207, 2.000000000000001776 ) ;
#11003 = EDGE_CURVE ( 'NONE', #4892, #8845, #33800, .T. ) ;
#11004 = ORIENTED_EDGE ( 'NONE', *, *, #14187, .F. ) ;
#11005 = EDGE_CURVE ( 'NONE', #26527, #23588, #5116, .T. ) ;
#11006 = DIRECTION ( 'NONE',  ( -0.5000000000000041078, -0.8660254037844364872, 0.000000000000000000 ) ) ;
#11007 = DIRECTION ( 'NONE',  ( 0.000000000000000000, 0.000000000000000000, 1.000000000000000000 ) ) ;
#11008 = DIRECTION ( 'NONE',  ( 0.000000000000000000, 0.000000000000000000, 1.000000000000000000 ) ) ;
#11009 = DIRECTION ( 'NONE',  ( 0.000000000000000000, 0.000000000000000000, 1.000000000000000000 ) ) ;
#11010 = ORIENTED_EDGE ( 'NONE', *, *, #1277, .F. ) ;
#11011 = DIRECTION ( 'NONE',  ( 0.000000000000000000, 0.000000000000000000, 1.000000000000000000 ) ) ;
#11012 = CYLINDRICAL_SURFACE ( 'NONE', #10063, 27.00000000000001066 ) ;
#11013 = DIRECTION ( 'NONE',  ( 0.000000000000000000, 0.000000000000000000, 1.000000000000000000 ) ) ;
#11014 = EDGE_CURVE ( 'NONE', #27066, #20492, #14253, .T. ) ;
#11015 = ADVANCED_FACE ( 'NONE', ( #28175 ), #13546, .F. ) ;
#11016 = ORIENTED_EDGE ( 'NONE', *, *, #35796, .T. ) ;
#11017 = CIRCLE ( 'NONE', #26009, 3.750000000000001776 ) ;
#11018 = VERTEX_POINT ( 'NONE', #25549 ) ;
#11019 = ADVANCED_FACE ( 'NONE', ( #2313 ), #36793, .F. ) ;
#11020 = EDGE_CURVE ( 'NONE', #2812, #23997, #11097, .T. ) ;
#11021 = DIRECTION ( 'NONE',  ( 0.000000000000000000, 0.000000000000000000, 1.000000000000000000 ) ) ;
#11023 = ADVANCED_FACE ( 'NONE', ( #27791 ), #31177, .F. ) ;
#11022 = VERTEX_POINT ( 'NONE', #7930 ) ;
#11024 = CARTESIAN_POINT ( 'NONE',  ( 4.279621169095998212, -62.97617850287780072, 12.49999999999999822 ) ) ;
#11025 = DIRECTION ( 'NONE',  ( 1.000000000000000000, 0.000000000000000000, 0.000000000000000000 ) ) ;
#11026 = CIRCLE ( 'NONE', #17599, 3.499999999999989342 ) ;
#11027 = CARTESIAN_POINT ( 'NONE',  ( 2.285412292771005660, 4.454019289455640518, -3.350862339338012141E-15 ) ) ;
#11028 = VECTOR ( 'NONE', #29428, 1000.000000000000000 ) ;
#11029 = DIRECTION ( 'NONE',  ( 0.000000000000000000, 0.000000000000000000, 1.000000000000000000 ) ) ;
#11030 = CARTESIAN_POINT ( 'NONE',  ( 106.2299462780987227, -40.32678999516329554, 32.50000000000000711 ) ) ;
#11031 = CARTESIAN_POINT ( 'NONE',  ( 77.99999662536833966, -3.224517592124143893E-15, -9.999999999999998224 ) ) ;
#11032 = CARTESIAN_POINT ( 'NONE',  ( 6.726859516510129922, 8.238026975208042369E-16, -4.599999999999999645 ) ) ;
#11033 = CARTESIAN_POINT ( 'NONE',  ( 81.99999662536832545, -34.64101615137759183, -9.999999999999998224 ) ) ;
#11034 = ORIENTED_EDGE ( 'NONE', *, *, #27473, .T. ) ;
#11035 = VERTEX_POINT ( 'NONE', #22545 ) ;
#11036 = LINE ( 'NONE', #22479, #17681 ) ;
#11037 = CARTESIAN_POINT ( 'NONE',  ( -51.13139720814380240, 27.50000000000055422, -10.00000000000000000 ) ) ;
#11038 = DIRECTION ( 'NONE',  ( 0.000000000000000000, 0.000000000000000000, 1.000000000000000000 ) ) ;
#11039 = AXIS2_PLACEMENT_3D ( 'NONE', #15556, #18565, #1118 ) ;
#11040 = DIRECTION ( 'NONE',  ( 1.000000000000000000, 0.000000000000000000, 0.000000000000000000 ) ) ;
#11041 = ORIENTED_EDGE ( 'NONE', *, *, #9266, .F. ) ;
#11042 = CIRCLE ( 'NONE', #15846, 2.000000000000001776 ) ;
#11043 = FACE_OUTER_BOUND ( 'NONE', #14030, .T. ) ;
#11044 = ORIENTED_EDGE ( 'NONE', *, *, #25361, .F. ) ;
#11045 = ORIENTED_EDGE ( 'NONE', *, *, #35695, .T. ) ;
#11046 = DIRECTION ( 'NONE',  ( 1.000000000000000000, 0.000000000000000000, 0.000000000000000000 ) ) ;
#11047 = ORIENTED_EDGE ( 'NONE', *, *, #34446, .T. ) ;
#11048 = LINE ( 'NONE', #5066, #13596 ) ;
#11049 = AXIS2_PLACEMENT_3D ( 'NONE', #32009, #31829, #17593 ) ;
#11050 = CIRCLE ( 'NONE', #31982, 2.000000000000001776 ) ;
#11051 = FACE_OUTER_BOUND ( 'NONE', #8089, .T. ) ;
#11052 = AXIS2_PLACEMENT_3D ( 'NONE', #2983, #5241, #16678 ) ;
#11053 = CARTESIAN_POINT ( 'NONE',  ( -73.00000337463097821, 43.30127018922197379, -9.999999999999998224 ) ) ;
#11054 = ORIENTED_EDGE ( 'NONE', *, *, #7335, .T. ) ;
#11055 = ORIENTED_EDGE ( 'NONE', *, *, #2306, .T. ) ;
#11056 = ORIENTED_EDGE ( 'NONE', *, *, #20907, .T. ) ;
#11057 = ADVANCED_FACE ( 'NONE', ( #14095, #36992, #2871, #5661, #30615, #4931, #16367 ), #13746, .F. ) ;
#11058 = EDGE_LOOP ( 'NONE', ( #27920, #16394, #27861, #37107 ) ) ;
#11059 = EDGE_LOOP ( 'NONE', ( #5184, #30125, #21252, #24634 ) ) ;
#11060 = EDGE_CURVE ( 'NONE', #13754, #17529, #13068, .T. ) ;
#11062 = CARTESIAN_POINT ( 'NONE',  ( 7.999996625368656744, -69.28203230275519786, -9.999999999999998224 ) ) ;
#11061 = AXIS2_PLACEMENT_3D ( 'NONE', #20540, #8946, #31963 ) ;
#11063 = EDGE_CURVE ( 'NONE', #11374, #26778, #3499, .T. ) ;
#11064 = DIRECTION ( 'NONE',  ( 0.000000000000000000, 0.000000000000000000, 1.000000000000000000 ) ) ;
#11065 = AXIS2_PLACEMENT_3D ( 'NONE', #5381, #17174, #22612 ) ;
#11066 = FACE_OUTER_BOUND ( 'NONE', #19392, .T. ) ;
#11067 = LINE ( 'NONE', #3022, #13925 ) ;
#11068 = CARTESIAN_POINT ( 'NONE',  ( 4.999999999999999112, 3.083561376477503835, -4.289114130331824981 ) ) ;
#11069 = ORIENTED_EDGE ( 'NONE', *, *, #19768, .F. ) ;
#11070 = CARTESIAN_POINT ( 'NONE',  ( 69.99999662536839651, -3.469446951953614189E-15, 17.49999999999999645 ) ) ;
#11071 = AXIS2_PLACEMENT_3D ( 'NONE', #35633, #13682, #19682 ) ;
#11072 = DIRECTION ( 'NONE',  ( 0.000000000000000000, 0.000000000000000000, 1.000000000000000000 ) ) ;
#11073 = DIRECTION ( 'NONE',  ( 1.000000000000000000, 0.000000000000000000, 0.000000000000000000 ) ) ;
#11074 = EDGE_LOOP ( 'NONE', ( #11303, #32331, #22218, #19318 ) ) ;
#11075 = DIRECTION ( 'NONE',  ( -0.000000000000000000, -0.000000000000000000, -1.000000000000000000 ) ) ;
#11076 = DIRECTION ( 'NONE',  ( 0.000000000000000000, 0.000000000000000000, 1.000000000000000000 ) ) ;
#11077 = AXIS2_PLACEMENT_3D ( 'NONE', #34649, #508, #11933 ) ;
#11078 = ORIENTED_EDGE ( 'NONE', *, *, #27206, .T. ) ;
#11079 = ORIENTED_EDGE ( 'NONE', *, *, #23159, .F. ) ;
#11080 = CARTESIAN_POINT ( 'NONE',  ( 5.000000000000000000, 0.000000000000000000, 2.266666666666666607 ) ) ;
#11081 = CARTESIAN_POINT ( 'NONE',  ( -20.00000337463124112, 69.28203230275516944, -9.999999999999998224 ) ) ;
#11082 = DIRECTION ( 'NONE',  ( -0.000000000000000000, -0.000000000000000000, 1.000000000000000000 ) ) ;
#11083 = DIRECTION ( 'NONE',  ( 0.000000000000000000, 0.000000000000000000, 1.000000000000000000 ) ) ;
#11084 = ORIENTED_EDGE ( 'NONE', *, *, #1998, .T. ) ;
#11085 = ORIENTED_EDGE ( 'NONE', *, *, #945, .T. ) ;
#11086 = EDGE_CURVE ( 'NONE', #11561, #10755, #208, .T. ) ;
#11087 = CARTESIAN_POINT ( 'NONE',  ( -75.00000337463097821, 43.30127018922197379, -9.999999999999998224 ) ) ;
#11088 = CIRCLE ( 'NONE', #35648, 27.00000000000001421 ) ;
#11089 = ORIENTED_EDGE ( 'NONE', *, *, #26872, .F. ) ;
#11090 = AXIS2_PLACEMENT_3D ( 'NONE', #17856, #34754, #31727 ) ;
#11091 = CARTESIAN_POINT ( 'NONE',  ( -83.00000337463092137, -25.98076211353322051, -9.999999999999998224 ) ) ;
#11092 = EDGE_LOOP ( 'NONE', ( #19579, #6386, #30856, #24424 ) ) ;
#11093 = VECTOR ( 'NONE', #34728, 1000.000000000000000 ) ;
#11094 = CARTESIAN_POINT ( 'NONE',  ( 0.000000000000000000, 89.94802294027088863, 30.49999999999999289 ) ) ;
#11095 = COLOUR_RGB ( '', 0.31764706, 0.68627451, 0.89019608) ;
#11096 = DIRECTION ( 'NONE',  ( -0.000000000000000000, -0.000000000000000000, 1.000000000000000000 ) ) ;
#11097 = LINE ( 'NONE', #28342, #31609 ) ;
#11098 = ORIENTED_EDGE ( 'NONE', *, *, #8945, .T. ) ;
#11099 = ORIENTED_EDGE ( 'NONE', *, *, #13246, .F. ) ;
#11100 = CARTESIAN_POINT ( 'NONE',  ( 102.5304832720488832, -102.5304832720499633, 32.55002500000000509 ) ) ;
#11101 = DIRECTION ( 'NONE',  ( -0.000000000000000000, -0.000000000000000000, -1.000000000000000000 ) ) ;
#11102 = AXIS2_PLACEMENT_3D ( 'NONE', #14524, #17164, #3267 ) ;
#11103 = LINE ( 'NONE', #2115, #23463 ) ;
#11104 = CIRCLE ( 'NONE', #14103, 2.000000000000000000 ) ;
#11105 = DIRECTION ( 'NONE',  ( 0.000000000000000000, 0.000000000000000000, 1.000000000000000000 ) ) ;
#11106 = ORIENTED_EDGE ( 'NONE', *, *, #35027, .T. ) ;
#11107 = DIRECTION ( 'NONE',  ( 1.000000000000000000, 0.000000000000000000, 0.000000000000000000 ) ) ;
#11108 = ADVANCED_FACE ( 'NONE', ( #32062 ), #23850, .F. ) ;
#11109 = FACE_BOUND ( 'NONE', #31736, .T. ) ;
#11110 = DIRECTION ( 'NONE',  ( 1.000000000000000000, 0.000000000000000000, 0.000000000000000000 ) ) ;
#11111 = DIRECTION ( 'NONE',  ( 1.000000000000000000, 0.000000000000000000, 0.000000000000000000 ) ) ;
#11112 = CYLINDRICAL_SURFACE ( 'NONE', #16504, 2.000000000000001776 ) ;
#11113 = DIRECTION ( 'NONE',  ( 0.000000000000000000, 0.000000000000000000, 1.000000000000000000 ) ) ;
#11114 = CARTESIAN_POINT ( 'NONE',  ( 43.19957991610432657, 47.04203867989531318, 12.49999999999999822 ) ) ;
#11115 = CIRCLE ( 'NONE', #23112, 3.499999999999996003 ) ;
#11116 = DIRECTION ( 'NONE',  ( 1.000000000000000000, 0.000000000000000000, 0.000000000000000000 ) ) ;
#11117 = ORIENTED_EDGE ( 'NONE', *, *, #10160, .F. ) ;
#11119 = AXIS2_PLACEMENT_3D ( 'NONE', #4177, #24784, #27202 ) ;
#11118 = DIRECTION ( 'NONE',  ( 0.000000000000000000, 0.000000000000000000, 1.000000000000000000 ) ) ;
#11120 = FACE_OUTER_BOUND ( 'NONE', #21957, .T. ) ;
#11121 = CARTESIAN_POINT ( 'NONE',  ( 45.00000000000000711, 0.000000000000000000, -10.00000000000000000 ) ) ;
#11122 = AXIS2_PLACEMENT_3D ( 'NONE', #3712, #6527, #11410 ) ;
#11123 = AXIS2_PLACEMENT_3D ( 'NONE', #20956, #30117, #9875 ) ;
#11124 = AXIS2_PLACEMENT_3D ( 'NONE', #27824, #16047, #28027 ) ;
#11125 = EDGE_LOOP ( 'NONE', ( #8258, #30095, #35405, #17176 ) ) ;
#11126 = CIRCLE ( 'NONE', #14718, 2.000000000000001776 ) ;
#11127 = EDGE_LOOP ( 'NONE', ( #15442, #21978, #4469, #8084 ) ) ;
#11128 = ORIENTED_EDGE ( 'NONE', *, *, #3705, .T. ) ;
#11129 = EDGE_CURVE ( 'NONE', #10522, #25534, #14645, .T. ) ;
#11130 = FACE_OUTER_BOUND ( 'NONE', #8796, .T. ) ;
#11131 = DIRECTION ( 'NONE',  ( -0.000000000000000000, -0.000000000000000000, 1.000000000000000000 ) ) ;
#11132 = EDGE_LOOP ( 'NONE', ( #18921, #15429 ) ) ;
#11133 = AXIS2_PLACEMENT_3D ( 'NONE', #2180, #33315, #30509 ) ;
#11134 = EDGE_CURVE ( 'NONE', #24333, #719, #22636, .T. ) ;
#11135 = AXIS2_PLACEMENT_3D ( 'NONE', #8154, #10956, #36833 ) ;
#11136 = LINE ( 'NONE', #36655, #19127 ) ;
#11137 = EDGE_LOOP ( 'NONE', ( #27876, #27777 ) ) ;
#11138 = LINE ( 'NONE', #14137, #23965 ) ;
#11139 = ADVANCED_FACE ( 'NONE', ( #31713 ), #9398, .F. ) ;
#11140 = ORIENTED_EDGE ( 'NONE', *, *, #11528, .F. ) ;
#11141 = DIRECTION ( 'NONE',  ( -0.000000000000000000, -0.000000000000000000, 1.000000000000000000 ) ) ;
#11142 = EDGE_LOOP ( 'NONE', ( #3726, #5525, #34998, #32602 ) ) ;
#11143 = EDGE_CURVE ( 'NONE', #17730, #35778, #12179, .T. ) ;
#11144 = CARTESIAN_POINT ( 'NONE',  ( -72.00000337463100664, 51.96152422706637708, -9.999999999999998224 ) ) ;
#11145 = CARTESIAN_POINT ( 'NONE',  ( 84.99999662536832545, 8.660254037844394404, 17.49999999999999645 ) ) ;
#11146 = AXIS2_PLACEMENT_3D ( 'NONE', #33204, #1518, #27595 ) ;
#11147 = ORIENTED_EDGE ( 'NONE', *, *, #8202, .T. ) ;
#11148 =( GEOMETRIC_REPRESENTATION_CONTEXT ( 3 ) GLOBAL_UNCERTAINTY_ASSIGNED_CONTEXT ( ( #32826 ) ) GLOBAL_UNIT_ASSIGNED_CONTEXT ( ( #26416, #32005, #24550 ) ) REPRESENTATION_CONTEXT ( 'NONE', 'WORKASPACE' ) );
#11149 = DIRECTION ( 'NONE',  ( 0.000000000000000000, 0.000000000000000000, -1.000000000000000000 ) ) ;
#11150 = VECTOR ( 'NONE', #11866, 1000.000000000000000 ) ;
#11151 = AXIS2_PLACEMENT_3D ( 'NONE', #22550, #28179, #5496 ) ;
#11152 = ITEM_DEFINED_TRANSFORMATION ( 'NONE', 'NONE', #17157,  #21385 ) ;
#11153 = CIRCLE ( 'NONE', #35124, 2.000000000000001776 ) ;
#11154 = DIRECTION ( 'NONE',  ( -0.000000000000000000, -0.000000000000000000, 1.000000000000000000 ) ) ;
#11155 = PLANE ( 'NONE',  #12235 ) ;
#11156 = AXIS2_PLACEMENT_3D ( 'NONE', #36164, #21909, #27708 ) ;
#11157 = EDGE_LOOP ( 'NONE', ( #20669, #1568 ) ) ;
#11158 = CARTESIAN_POINT ( 'NONE',  ( 56.67878100130369035, -27.78182860042797131, -4.999999999999997335 ) ) ;
#11159 = CARTESIAN_POINT ( 'NONE',  ( -60.00000337463104216, 34.64101615137757051, -9.999999999999998224 ) ) ;
#11160 = ORIENTED_EDGE ( 'NONE', *, *, #7129, .T. ) ;
#11161 = EDGE_CURVE ( 'NONE', #23429, #7967, #11851, .T. ) ;
#11162 = DIRECTION ( 'NONE',  ( -1.000000000000000000, 0.000000000000000000, 0.000000000000000000 ) ) ;
#11163 = LINE ( 'NONE', #25076, #7089 ) ;
#11164 = DIRECTION ( 'NONE',  ( 0.000000000000000000, 0.000000000000000000, 1.000000000000000000 ) ) ;
#11165 = DIRECTION ( 'NONE',  ( 1.000000000000000000, 0.000000000000000000, 0.000000000000000000 ) ) ;
#11166 = AXIS2_PLACEMENT_3D ( 'NONE', #23507, #34946, #8891 ) ;
#11167 = ORIENTED_EDGE ( 'NONE', *, *, #437, .F. ) ;
#11168 = ORIENTED_EDGE ( 'NONE', *, *, #25462, .F. ) ;
#11169 = DIRECTION ( 'NONE',  ( 1.000000000000000000, 0.000000000000000000, 0.000000000000000000 ) ) ;
#11170 = DIRECTION ( 'NONE',  ( 1.000000000000000000, 0.000000000000000000, 0.000000000000000000 ) ) ;
#11171 = AXIS2_PLACEMENT_3D ( 'NONE', #3064, #5874, #14655 ) ;
#11172 = ADVANCED_FACE ( 'NONE', ( #29448 ), #15205, .F. ) ;
#11173 = EDGE_LOOP ( 'NONE', ( #23237, #9717, #12773, #23059, #20293 ) ) ;
#11174 = VERTEX_POINT ( 'NONE', #31877 ) ;
#11175 = EDGE_CURVE ( 'NONE', #3360, #630, #24462, .T. ) ;
#11176 = DIRECTION ( 'NONE',  ( 0.000000000000000000, 0.000000000000000000, -1.000000000000000000 ) ) ;
#11177 = CARTESIAN_POINT ( 'NONE',  ( -2.744988726042923766, 4.188682711992889551, -0.5083873451168725577 ) ) ;
#11178 = DIRECTION ( 'NONE',  ( 0.000000000000000000, 0.000000000000000000, 1.000000000000000000 ) ) ;
#11179 = AXIS2_PLACEMENT_3D ( 'NONE', #14850, #20637, #34912 ) ;
#11180 = AXIS2_PLACEMENT_3D ( 'NONE', #19259, #26948, #17179 ) ;
#11181 = ORIENTED_EDGE ( 'NONE', *, *, #14853, .T. ) ;
#11182 = VECTOR ( 'NONE', #17488, 1000.000000000000000 ) ;
#11183 = ORIENTED_EDGE ( 'NONE', *, *, #531, .F. ) ;
#11184 = DIRECTION ( 'NONE',  ( 1.000000000000000000, 0.000000000000000000, 0.000000000000000000 ) ) ;
#11185 = AXIS2_PLACEMENT_3D ( 'NONE', #10072, #13059, #35008 ) ;
#11186 = CYLINDRICAL_SURFACE ( 'NONE', #14089, 3.000000000000006217 ) ;
#11187 = ORIENTED_EDGE ( 'NONE', *, *, #34431, .F. ) ;
#11188 = DIRECTION ( 'NONE',  ( 0.000000000000000000, 0.000000000000000000, 1.000000000000000000 ) ) ;
#11189 = EDGE_CURVE ( 'NONE', #20938, #19811, #3601, .T. ) ;
#11190 = ORIENTED_EDGE ( 'NONE', *, *, #2357, .F. ) ;
#11191 = FACE_BOUND ( 'NONE', #10674, .T. ) ;
#11192 = AXIS2_PLACEMENT_3D ( 'NONE', #17094, #25355, #14086 ) ;
#11193 = EDGE_CURVE ( 'NONE', #5840, #17343, #16055, .T. ) ;
#11194 = CARTESIAN_POINT ( 'NONE',  ( 9.999996625368618552, 69.28203230275516944, -9.999999999999998224 ) ) ;
#11195 = VERTEX_POINT ( 'NONE', #25910 ) ;
#11196 = AXIS2_PLACEMENT_3D ( 'NONE', #22822, #31241, #36871 ) ;
#11197 = DIRECTION ( 'NONE',  ( 1.000000000000000000, 0.000000000000000000, 0.000000000000000000 ) ) ;
#11198 = CONICAL_SURFACE ( 'NONE', #7001, 2.541999999999999815, 1.047197551196591858 ) ;
#11199 = CARTESIAN_POINT ( 'NONE',  ( 0.000000000000000000, 0.000000000000000000, -6.000000000000000000 ) ) ;
#11200 = AXIS2_PLACEMENT_3D ( 'NONE', #29344, #12071, #32344 ) ;
#11201 = DIRECTION ( 'NONE',  ( 1.224646799147353207E-16, 1.000000000000000000, -0.000000000000000000 ) ) ;
#11202 = DIRECTION ( 'NONE',  ( -1.000000000000000000, 0.000000000000000000, 0.000000000000000000 ) ) ;
#11203 = ORIENTED_EDGE ( 'NONE', *, *, #36146, .T. ) ;
#11204 = CARTESIAN_POINT ( 'NONE',  ( 79.99999662536832545, -17.32050807568879591, 17.49999999999999645 ) ) ;
#11205 = CARTESIAN_POINT ( 'NONE',  ( -79.83584802575171580, -32.64776428033012934, 12.50000000000000000 ) ) ;
#11206 = CARTESIAN_POINT ( 'NONE',  ( -4.180704885107413560, -3.359771601077115921, -5.801655677627839403 ) ) ;
#11207 = AXIS2_PLACEMENT_3D ( 'NONE', #31214, #13955, #36662 ) ;
#11208 = CIRCLE ( 'NONE', #36973, 3.499999999999996003 ) ;
#11209 = EDGE_LOOP ( 'NONE', ( #27750, #35234, #31095, #21229 ) ) ;
#11210 = CIRCLE ( 'NONE', #19601, 2.999999999999999556 ) ;
#11211 = EDGE_CURVE ( 'NONE', #27018, #1819, #11638, .T. ) ;
#11212 = ORIENTED_EDGE ( 'NONE', *, *, #29687, .T. ) ;
#11213 = VERTEX_POINT ( 'NONE', #23291 ) ;
#11214 = CARTESIAN_POINT ( 'NONE',  ( 67.99999662536838230, -3.224517592124143893E-15, 12.50000000000000000 ) ) ;
#11215 = AXIS2_PLACEMENT_3D ( 'NONE', #29735, #15871, #30109 ) ;
#11216 = CARTESIAN_POINT ( 'NONE',  ( -5.000003374631269537, -77.94228634059960825, -9.999999999999998224 ) ) ;
#11217 = VECTOR ( 'NONE', #12742, 1000.000000000000000 ) ;
#11218 = EDGE_CURVE ( 'NONE', #18582, #14464, #18464, .T. ) ;
#11219 = CARTESIAN_POINT ( 'NONE',  ( -78.00000337463094979, -17.32050807568882078, 17.49999999999999645 ) ) ;
#11220 = AXIS2_PLACEMENT_3D ( 'NONE', #16438, #22947, #34769 ) ;
#11221 = CARTESIAN_POINT ( 'NONE',  ( 42.99999662536848888, 60.62177826491077326, 17.49999999999999645 ) ) ;
#11222 = EDGE_CURVE ( 'NONE', #16746, #8683, #25641, .T. ) ;
#11223 = CARTESIAN_POINT ( 'NONE',  ( 0.000000000000000000, -1.467624384280027172, 2.542000000000001592 ) ) ;
#11224 = CARTESIAN_POINT ( 'NONE',  ( -106.4310728746527133, -54.27667806281213103, 32.50000000000000000 ) ) ;
#11225 = EDGE_CURVE ( 'NONE', #4653, #3063, #11833, .T. ) ;
#11226 = LINE ( 'NONE', #22471, #3429 ) ;
#11227 = AXIS2_PLACEMENT_3D ( 'NONE', #23914, #24649, #32506 ) ;
#11228 = FACE_OUTER_BOUND ( 'NONE', #34313, .T. ) ;
#11229 = EDGE_LOOP ( 'NONE', ( #13880, #1557, #18690, #20093 ) ) ;
#11230 = AXIS2_PLACEMENT_3D ( 'NONE', #25555, #5668, #28734 ) ;
#11231 = ORIENTED_EDGE ( 'NONE', *, *, #33143, .F. ) ;
#11232 = CARTESIAN_POINT ( 'NONE',  ( -2.775557561562891351E-14, 19.94802294027085310, 27.49999999999999645 ) ) ;
#11233 = AXIS2_PLACEMENT_3D ( 'NONE', #6976, #29096, #12198 ) ;
#11234 = DIRECTION ( 'NONE',  ( -1.000000000000000000, 0.000000000000000000, 0.000000000000000000 ) ) ;
#11235 = DIRECTION ( 'NONE',  ( 0.000000000000000000, 0.000000000000000000, 1.000000000000000000 ) ) ;
#11236 = DIRECTION ( 'NONE',  ( 0.000000000000000000, 0.000000000000000000, 1.000000000000000000 ) ) ;
#11237 = VERTEX_POINT ( 'NONE', #6210 ) ;
#11238 = AXIS2_PLACEMENT_3D ( 'NONE', #20564, #26019, #26216 ) ;
#11239 = CIRCLE ( 'NONE', #21441, 2.000000000000001776 ) ;
#11240 = EDGE_CURVE ( 'NONE', #6874, #374, #5300, .T. ) ;
#11241 = FACE_BOUND ( 'NONE', #4677, .T. ) ;
#11242 = ORIENTED_EDGE ( 'NONE', *, *, #415, .F. ) ;
#11243 = ORIENTED_EDGE ( 'NONE', *, *, #16368, .F. ) ;
#11244 = CYLINDRICAL_SURFACE ( 'NONE', #3438, 2.000000000000001776 ) ;
#11245 = EDGE_LOOP ( 'NONE', ( #15225, #27223, #5867, #30666 ) ) ;
#11246 = AXIS2_PLACEMENT_3D ( 'NONE', #18650, #32895, #23913 ) ;
#11247 =( NAMED_UNIT ( * ) SI_UNIT ( $, .STERADIAN. ) SOLID_ANGLE_UNIT ( ) );
#11248 = DIRECTION ( 'NONE',  ( -1.000000000000000000, 0.000000000000000000, 0.000000000000000000 ) ) ;
#11249 = PRODUCT ( 'socket head cap screw_iso_ISO 4762 M6 x 60 - 24N', 'socket head cap screw_iso_ISO 4762 M6 x 60 - 24N', '', ( #29372 ) ) ;
#11250 = CARTESIAN_POINT ( 'NONE',  ( -55.00000337463110611, -43.30127018922202353, 12.50000000000000000 ) ) ;
#11251 = VECTOR ( 'NONE', #31523, 1000.000000000000000 ) ;
#11252 = CARTESIAN_POINT ( 'NONE',  ( 3.000000000000000000, -2.935248768560059229, 3.469446951953614189E-15 ) ) ;
#11253 = EDGE_LOOP ( 'NONE', ( #24364, #12459, #4499, #3912 ) ) ;
#11254 = ORIENTED_EDGE ( 'NONE', *, *, #36027, .T. ) ;
#11255 = CIRCLE ( 'NONE', #8841, 2.000000000000001776 ) ;
#11256 = ORIENTED_EDGE ( 'NONE', *, *, #19467, .T. ) ;
#11257 = EDGE_LOOP ( 'NONE', ( #13857, #17632, #5275, #9946 ) ) ;
#11258 = EDGE_CURVE ( 'NONE', #11631, #18383, #26286, .T. ) ;
#11259 = AXIS2_PLACEMENT_3D ( 'NONE', #28154, #16529, #8289 ) ;
#11260 = ORIENTED_EDGE ( 'NONE', *, *, #16531, .T. ) ;
#11261 = DIRECTION ( 'NONE',  ( 1.000000000000000000, 0.000000000000000000, 0.000000000000000000 ) ) ;
#11262 = FACE_OUTER_BOUND ( 'NONE', #10194, .T. ) ;
#11263 = EDGE_CURVE ( 'NONE', #18862, #5705, #12443, .T. ) ;
#11264 = CARTESIAN_POINT ( 'NONE',  ( -70.00000337463099243, -2.428612866367529932E-14, -9.999999999999998224 ) ) ;
#11265 = DIRECTION ( 'NONE',  ( 1.000000000000000000, 0.000000000000000000, 0.000000000000000000 ) ) ;
#11266 = DIRECTION ( 'NONE',  ( 0.000000000000000000, 0.000000000000000000, 1.000000000000000000 ) ) ;
#11267 = ORIENTED_EDGE ( 'NONE', *, *, #22872, .T. ) ;
#11268 = DIRECTION ( 'NONE',  ( 0.000000000000000000, 0.000000000000000000, 1.000000000000000000 ) ) ;
#11269 = AXIS2_PLACEMENT_3D ( 'NONE', #16861, #22299, #28280 ) ;
#11270 = DIRECTION ( 'NONE',  ( 1.000000000000000000, 0.000000000000000000, 0.000000000000000000 ) ) ;
#11271 = CARTESIAN_POINT ( 'NONE',  ( 68.00000000000000000, 0.000000000000000000, 12.49999999999999822 ) ) ;
#11272 = VERTEX_POINT ( 'NONE', #12579 ) ;
#11273 = DIRECTION ( 'NONE',  ( 0.000000000000000000, 0.4999999999999953926, -0.8660254037844412611 ) ) ;
#11274 = EDGE_CURVE ( 'NONE', #31389, #3917, #15461, .T. ) ;
#11275 = DIRECTION ( 'NONE',  ( 1.000000000000000000, 0.000000000000000000, 0.000000000000000000 ) ) ;
#11276 = CIRCLE ( 'NONE', #34657, 2.000000000000001776 ) ;
#11277 = EDGE_LOOP ( 'NONE', ( #26562, #27918, #32448, #23382, #33652 ) ) ;
#11278 = ORIENTED_EDGE ( 'NONE', *, *, #13653, .F. ) ;
#11279 = CARTESIAN_POINT ( 'NONE',  ( 62.99999662536839651, -60.62177826491080168, -9.999999999999998224 ) ) ;
#11280 = AXIS2_PLACEMENT_3D ( 'NONE', #32631, #13147, #27016 ) ;
#11281 = FACE_OUTER_BOUND ( 'NONE', #12709, .T. ) ;
#11282 = LINE ( 'NONE', #20274, #25850 ) ;
#11283 = CARTESIAN_POINT ( 'NONE',  ( -5.122335214190873565, -2.957381614792632618, -4.281769937709105633 ) ) ;
#11284 = ORIENTED_EDGE ( 'NONE', *, *, #27545, .T. ) ;
#11285 = ORIENTED_EDGE ( 'NONE', *, *, #8533, .F. ) ;
#11286 = AXIS2_PLACEMENT_3D ( 'NONE', #34819, #14945, #682 ) ;
#11287 = EDGE_CURVE ( 'NONE', #18742, #18793, #26832, .T. ) ;
#11288 = AXIS2_PLACEMENT_3D ( 'NONE', #7432, #1619, #15873 ) ;
#11289 = EDGE_CURVE ( 'NONE', #4478, #25776, #27394, .T. ) ;
#11290 = CARTESIAN_POINT ( 'NONE',  ( 62.97617850287784336, 4.279621169095339184, -4.999999999999997335 ) ) ;
#11291 = EDGE_CURVE ( 'NONE', #9788, #23537, #25058, .T. ) ;
#11292 = ORIENTED_EDGE ( 'NONE', *, *, #13286, .T. ) ;
#11293 = EDGE_CURVE ( 'NONE', #28140, #1125, #1894, .T. ) ;
#11294 = CARTESIAN_POINT ( 'NONE',  ( 94.55012560584677317, -9.234378588654733377, 27.50000000000000000 ) ) ;
#11295 = ORIENTED_EDGE ( 'NONE', *, *, #34804, .T. ) ;
#11296 = AXIS2_PLACEMENT_3D ( 'NONE', #17455, #11622, #23076 ) ;
#11297 = ORIENTED_EDGE ( 'NONE', *, *, #14236, .T. ) ;
#11298 = CIRCLE ( 'NONE', #22679, 2.000000000000001776 ) ;
#11299 = DIRECTION ( 'NONE',  ( 0.000000000000000000, 0.000000000000000000, 1.000000000000000000 ) ) ;
#11300 = DIRECTION ( 'NONE',  ( 1.000000000000000000, 0.000000000000000000, 0.000000000000000000 ) ) ;
#11301 = CARTESIAN_POINT ( 'NONE',  ( -65.00000337463102085, 43.30127018922198801, -9.999999999999998224 ) ) ;
#11302 = ORIENTED_EDGE ( 'NONE', *, *, #20595, .T. ) ;
#11303 = ORIENTED_EDGE ( 'NONE', *, *, #16749, .F. ) ;
#11304 = CARTESIAN_POINT ( 'NONE',  ( -25.00000337463120914, 77.94228634059957983, 17.49999999999999645 ) ) ;
#11305 = CARTESIAN_POINT ( 'NONE',  ( -12.00000337463128908, 69.28203230275516944, 17.49999999999999645 ) ) ;
#11306 = DIRECTION ( 'NONE',  ( 0.000000000000000000, 0.000000000000000000, 1.000000000000000000 ) ) ;
#11307 = DIRECTION ( 'NONE',  ( 0.000000000000000000, 0.000000000000000000, 1.000000000000000000 ) ) ;
#11308 = ORIENTED_EDGE ( 'NONE', *, *, #6007, .F. ) ;
#11309 = DIRECTION ( 'NONE',  ( 0.000000000000000000, 0.000000000000000000, 1.000000000000000000 ) ) ;
#11310 = CIRCLE ( 'NONE', #23300, 3.000000000000002665 ) ;
#11311 = FACE_BOUND ( 'NONE', #9873, .T. ) ;
#11312 = VECTOR ( 'NONE', #23700, 1000.000000000000000 ) ;
#11313 = CARTESIAN_POINT ( 'NONE',  ( -67.00000337463106348, -60.62177826491083010, 12.50000000000000000 ) ) ;
#11314 = CARTESIAN_POINT ( 'NONE',  ( 0.000000000000000000, 89.94802294027088863, -19.99999999999999645 ) ) ;
#11315 = DIRECTION ( 'NONE',  ( 0.000000000000000000, 0.000000000000000000, -1.000000000000000000 ) ) ;
#11316 = EDGE_CURVE ( 'NONE', #10338, #4318, #34077, .T. ) ;
#11317 = PLANE ( 'NONE',  #23085 ) ;
#11318 = CARTESIAN_POINT ( 'NONE',  ( 9.944411252287574499, 118.0778277273563788, 27.49998800000000543 ) ) ;
#11319 = AXIS2_PLACEMENT_3D ( 'NONE', #12610, #21622, #24064 ) ;
#11320 = DIRECTION ( 'NONE',  ( -1.000000000000000000, 0.000000000000000000, 0.000000000000000000 ) ) ;
#11321 = VERTEX_POINT ( 'NONE', #6763 ) ;
#11322 = CARTESIAN_POINT ( 'NONE',  ( 17.55872235085559652, 89.94802294027088863, -24.99999999999999645 ) ) ;
#11323 = CARTESIAN_POINT ( 'NONE',  ( -4.999999999999997335, 0.000000000000000000, 0.000000000000000000 ) ) ;
#11324 = DIRECTION ( 'NONE',  ( 0.000000000000000000, 0.000000000000000000, -1.000000000000000000 ) ) ;
#11325 = ORIENTED_EDGE ( 'NONE', *, *, #11619, .T. ) ;
#11326 = ORIENTED_EDGE ( 'NONE', *, *, #17334, .T. ) ;
#11327 = CIRCLE ( 'NONE', #35882, 2.000000000000001776 ) ;
#11328 = EDGE_LOOP ( 'NONE', ( #728, #5886 ) ) ;
#11329 = DIRECTION ( 'NONE',  ( 0.000000000000000000, 0.000000000000000000, 1.000000000000000000 ) ) ;
#11330 = DIRECTION ( 'NONE',  ( 0.000000000000000000, 0.000000000000000000, 1.000000000000000000 ) ) ;
#11331 = PLANE ( 'NONE',  #35815 ) ;
#11332 = ORIENTED_EDGE ( 'NONE', *, *, #34984, .T. ) ;
#11333 = CARTESIAN_POINT ( 'NONE',  ( -45.00000000000000711, 5.510910596163090344E-15, -10.00000000000000000 ) ) ;
#11334 = CIRCLE ( 'NONE', #29877, 2.000000000000001776 ) ;
#11335 = ORIENTED_EDGE ( 'NONE', *, *, #10471, .F. ) ;
#11336 = EDGE_CURVE ( 'NONE', #20171, #12255, #7164, .T. ) ;
#11337 = FACE_OUTER_BOUND ( 'NONE', #11456, .T. ) ;
#11338 = ORIENTED_EDGE ( 'NONE', *, *, #31624, .F. ) ;
#11339 = DIRECTION ( 'NONE',  ( -1.000000000000000000, 0.000000000000000000, 0.000000000000000000 ) ) ;
#11340 = EDGE_LOOP ( 'NONE', ( #16202, #27600, #27231, #32825 ) ) ;
#11341 = VERTEX_POINT ( 'NONE', #4722 ) ;
#11342 = CARTESIAN_POINT ( 'NONE',  ( -80.00000337463094979, 34.64101615137757051, -5.000000000000000000 ) ) ;
#11343 = CARTESIAN_POINT ( 'NONE',  ( -84.88770934388888634, 10.65709906204123492, -5.000000000000000000 ) ) ;
#11344 = VERTEX_POINT ( 'NONE', #21596 ) ;
#11345 = DIRECTION ( 'NONE',  ( 1.000000000000000000, 0.000000000000000000, 0.000000000000000000 ) ) ;
#11346 = CARTESIAN_POINT ( 'NONE',  ( -65.00000000000000000, 0.000000000000000000, 17.49999999999999645 ) ) ;
#11347 = DIRECTION ( 'NONE',  ( -0.000000000000000000, 0.000000000000000000, -1.000000000000000000 ) ) ;
#11348 = AXIS2_PLACEMENT_3D ( 'NONE', #20536, #6681, #12660 ) ;
#11349 = EDGE_LOOP ( 'NONE', ( #29830, #28988, #33187, #1098 ) ) ;
#11350 = DIRECTION ( 'NONE',  ( 1.000000000000000000, 0.000000000000000000, 0.000000000000000000 ) ) ;
#11351 = DIRECTION ( 'NONE',  ( -1.000000000000000000, 0.000000000000000000, -0.000000000000000000 ) ) ;
#11352 = ORIENTED_EDGE ( 'NONE', *, *, #24031, .F. ) ;
#11353 = DIRECTION ( 'NONE',  ( 0.000000000000000000, 0.000000000000000000, 1.000000000000000000 ) ) ;
#11354 = CARTESIAN_POINT ( 'NONE',  ( -31.74999999999995737, 0.000000000000000000, 5.000000000000000000 ) ) ;
#11355 = AXIS2_PLACEMENT_3D ( 'NONE', #14058, #29033, #28854 ) ;
#11356 = CARTESIAN_POINT ( 'NONE',  ( 84.99999662536831124, -25.98076211353319565, -9.999999999999998224 ) ) ;
#11357 = EDGE_CURVE ( 'NONE', #2055, #35706, #35476, .T. ) ;
#11358 = EDGE_CURVE ( 'NONE', #4900, #35883, #17893, .T. ) ;
#11359 = CARTESIAN_POINT ( 'NONE',  ( -8.000003374631278419, -69.28203230275519786, -9.999999999999998224 ) ) ;
#11360 = ORIENTED_EDGE ( 'NONE', *, *, #29264, .T. ) ;
#11361 = AXIS2_PLACEMENT_3D ( 'NONE', #35755, #28045, #19612 ) ;
#11362 = ORIENTED_EDGE ( 'NONE', *, *, #24487, .F. ) ;
#11363 = EDGE_CURVE ( 'NONE', #14483, #34280, #7108, .T. ) ;
#11364 = CIRCLE ( 'NONE', #35926, 2.000000000000001776 ) ;
#11365 = CARTESIAN_POINT ( 'NONE',  ( 6.000000000000000000, -145.0000000000000568, 32.55002500000000509 ) ) ;
#11366 = DIRECTION ( 'NONE',  ( 1.000000000000000000, 0.000000000000000000, 0.000000000000000000 ) ) ;
#11368 = EDGE_LOOP ( 'NONE', ( #16712, #352 ) ) ;
#11367 = EDGE_CURVE ( 'NONE', #27049, #20566, #28062, .T. ) ;
#11369 = EDGE_LOOP ( 'NONE', ( #29425, #27256, #36711, #12000, #34283 ) ) ;
#11370 = DIRECTION ( 'NONE',  ( 0.000000000000000000, 0.000000000000000000, 1.000000000000000000 ) ) ;
#11371 = DIRECTION ( 'NONE',  ( 0.000000000000000000, 0.000000000000000000, -1.000000000000000000 ) ) ;
#11372 = CARTESIAN_POINT ( 'NONE',  ( -23.00000337463120559, 77.94228634059957983, 17.49999999999999645 ) ) ;
#11373 = AXIS2_PLACEMENT_3D ( 'NONE', #11919, #9106, #20532 ) ;
#11374 = VERTEX_POINT ( 'NONE', #4336 ) ;
#11375 = ORIENTED_EDGE ( 'NONE', *, *, #2801, .T. ) ;
#11376 = CARTESIAN_POINT ( 'NONE',  ( 108.3061974404897825, -19.22934205795014151, 32.50000000000000000 ) ) ;
#11377 = CARTESIAN_POINT ( 'NONE',  ( -12.00000337463127842, -69.28203230275519786, -9.999999999999998224 ) ) ;
#11378 = VERTEX_POINT ( 'NONE', #18771 ) ;
#11379 = AXIS2_PLACEMENT_3D ( 'NONE', #27808, #5507, #14317 ) ;
#11380 = EDGE_CURVE ( 'NONE', #30265, #3561, #16087, .T. ) ;
#11381 = CARTESIAN_POINT ( 'NONE',  ( -82.00000337463096400, -34.64101615137762025, 17.49999999999999645 ) ) ;
#11382 = EDGE_LOOP ( 'NONE', ( #16954, #28259, #25314, #19815, #26681, #24608, #22857, #11665, #11829, #24564, #20985, #33398, #33557 ) ) ;
#11384 = AXIS2_PLACEMENT_3D ( 'NONE', #19167, #11064, #5461 ) ;
#11383 = FACE_BOUND ( 'NONE', #7301, .T. ) ;
#11385 = DIRECTION ( 'NONE',  ( 0.000000000000000000, 0.000000000000000000, -1.000000000000000000 ) ) ;
#11386 = AXIS2_PLACEMENT_3D ( 'NONE', #29205, #6530, #23222 ) ;
#11387 = DIRECTION ( 'NONE',  ( 1.000000000000000000, 0.000000000000000000, 0.000000000000000000 ) ) ;
#11388 = CIRCLE ( 'NONE', #14981, 2.000000000000001776 ) ;
#11389 = VERTEX_POINT ( 'NONE', #24603 ) ;
#11390 = DIRECTION ( 'NONE',  ( 1.000000000000000000, 0.000000000000000000, 0.000000000000000000 ) ) ;
#11391 = DIRECTION ( 'NONE',  ( 0.000000000000000000, 0.000000000000000000, 1.000000000000000000 ) ) ;
#11392 = DIRECTION ( 'NONE',  ( -1.000000000000000000, 0.000000000000000000, 0.000000000000000000 ) ) ;
#11393 = CARTESIAN_POINT ( 'NONE',  ( 27.78182860042856461, 56.67878100130339902, 12.49999999999999822 ) ) ;
#11394 = ADVANCED_FACE ( 'NONE', ( #33760 ), #7709, .F. ) ;
#11395 = ORIENTED_EDGE ( 'NONE', *, *, #6674, .F. ) ;
#11396 = AXIS2_PLACEMENT_3D ( 'NONE', #32294, #1180, #21043 ) ;
#11397 = DIRECTION ( 'NONE',  ( 0.000000000000000000, 0.000000000000000000, 1.000000000000000000 ) ) ;
#11398 = DIRECTION ( 'NONE',  ( 0.5000000000000039968, 0.8660254037844363761, 0.000000000000000000 ) ) ;
#11399 = FACE_OUTER_BOUND ( 'NONE', #16823, .T. ) ;
#11400 = ORIENTED_EDGE ( 'NONE', *, *, #34548, .T. ) ;
#11401 = EDGE_LOOP ( 'NONE', ( #25189, #11910, #27171, #11770 ) ) ;
#11402 = AXIS2_PLACEMENT_3D ( 'NONE', #7906, #33970, #19527 ) ;
#11403 = ORIENTED_EDGE ( 'NONE', *, *, #28846, .F. ) ;
#11404 = EDGE_CURVE ( 'NONE', #33595, #35934, #14282, .T. ) ;
#11405 = COLOUR_RGB ( '', 0.66274510, 0.83137255, 0.94901961) ;
#11406 = FACE_OUTER_BOUND ( 'NONE', #14447, .T. ) ;
#11407 = EDGE_CURVE ( 'NONE', #22858, #30062, #10878, .T. ) ;
#11408 = DIRECTION ( 'NONE',  ( 1.000000000000000000, 0.000000000000000000, 0.000000000000000000 ) ) ;
#11409 = DIRECTION ( 'NONE',  ( 0.000000000000000000, -0.5000000000000011102, -0.8660254037844379305 ) ) ;
#11410 = DIRECTION ( 'NONE',  ( 1.000000000000000000, 0.000000000000000000, 0.000000000000000000 ) ) ;
#11411 = CARTESIAN_POINT ( 'NONE',  ( 5.999999999999947597, -2.132877728683645235E-15, 27.50000000000000000 ) ) ;
#11412 = DIRECTION ( 'NONE',  ( 0.000000000000000000, 0.000000000000000000, -1.000000000000000000 ) ) ;
#11413 = VERTEX_POINT ( 'NONE', #22498 ) ;
#11414 = ORIENTED_EDGE ( 'NONE', *, *, #4254, .T. ) ;
#11415 = DIRECTION ( 'NONE',  ( 1.000000000000000000, 0.000000000000000000, 0.000000000000000000 ) ) ;
#11416 = DIRECTION ( 'NONE',  ( 0.000000000000000000, 0.000000000000000000, 1.000000000000000000 ) ) ;
#11417 = LINE ( 'NONE', #26536, #13853 ) ;
#11418 = CARTESIAN_POINT ( 'NONE',  ( 3.000000000000000000, 2.935248768560057453, -3.903127820947815962E-15 ) ) ;
#11419 = ORIENTED_EDGE ( 'NONE', *, *, #6112, .F. ) ;
#11420 = EDGE_CURVE ( 'NONE', #36248, #30244, #11882, .T. ) ;
#11421 = DIRECTION ( 'NONE',  ( 0.000000000000000000, 0.000000000000000000, 1.000000000000000000 ) ) ;
#11422 = ORIENTED_EDGE ( 'NONE', *, *, #33414, .F. ) ;
#11423 = ORIENTED_EDGE ( 'NONE', *, *, #35981, .T. ) ;
#11424 = CARTESIAN_POINT ( 'NONE',  ( -15.00000337463125710, -77.94228634059960825, -5.000000000000000000 ) ) ;
#11425 = ORIENTED_EDGE ( 'NONE', *, *, #15211, .F. ) ;
#11426 = CARTESIAN_POINT ( 'NONE',  ( 86.99999662536831124, -8.660254037844397956, -9.999999999999998224 ) ) ;
#11427 = EDGE_CURVE ( 'NONE', #25842, #29105, #17284, .T. ) ;
#11428 = CARTESIAN_POINT ( 'NONE',  ( 51.99999662536847467, 51.96152422706637708, -5.000000000000000000 ) ) ;
#11429 = LINE ( 'NONE', #23046, #519 ) ;
#11430 = EDGE_CURVE ( 'NONE', #16632, #3771, #23869, .T. ) ;
#11431 = ORIENTED_EDGE ( 'NONE', *, *, #4806, .F. ) ;
#11432 = VERTEX_POINT ( 'NONE', #10708 ) ;
#11433 = EDGE_LOOP ( 'NONE', ( #9176, #9575 ) ) ;
#11434 = ORIENTED_EDGE ( 'NONE', *, *, #23617, .F. ) ;
#11435 = VERTEX_POINT ( 'NONE', #30583 ) ;
#11436 = PLANE ( 'NONE',  #29607 ) ;
#11437 = CARTESIAN_POINT ( 'NONE',  ( 0.000000000000000000, 0.000000000000000000, 5.000000000000000000 ) ) ;
#11438 = CIRCLE ( 'NONE', #18659, 2.000000000000000000 ) ;
#11439 = DIRECTION ( 'NONE',  ( 0.000000000000000000, 0.000000000000000000, 1.000000000000000000 ) ) ;
#11440 = LINE ( 'NONE', #30946, #11513 ) ;
#11441 = DIRECTION ( 'NONE',  ( 1.000000000000000000, 0.000000000000000000, 0.000000000000000000 ) ) ;
#11442 = ORIENTED_EDGE ( 'NONE', *, *, #12384, .F. ) ;
#11443 = DIRECTION ( 'NONE',  ( -0.000000000000000000, -0.000000000000000000, 1.000000000000000000 ) ) ;
#11444 = DIRECTION ( 'NONE',  ( 0.000000000000000000, 0.000000000000000000, -1.000000000000000000 ) ) ;
#11445 = EDGE_CURVE ( 'NONE', #30112, #29105, #12470, .T. ) ;
#11446 = CARTESIAN_POINT ( 'NONE',  ( -22.00000337463124112, -69.28203230275522628, 12.50000000000000000 ) ) ;
#11447 = ORIENTED_EDGE ( 'NONE', *, *, #25883, .T. ) ;
#11448 = CARTESIAN_POINT ( 'NONE',  ( 0.000000000000000000, 2.935248768560057453, -3.903127820947815962E-15 ) ) ;
#11449 = DIRECTION ( 'NONE',  ( 0.000000000000000000, 0.000000000000000000, 1.000000000000000000 ) ) ;
#11450 = VERTEX_POINT ( 'NONE', #25499 ) ;
#11451 = ORIENTED_EDGE ( 'NONE', *, *, #11951, .T. ) ;
#11452 = DIRECTION ( 'NONE',  ( 0.000000000000000000, 0.000000000000000000, 1.000000000000000000 ) ) ;
#11453 = CARTESIAN_POINT ( 'NONE',  ( -4.296971609540364945, 3.292644976426615688, -4.096693167835493199 ) ) ;
#11454 = DIRECTION ( 'NONE',  ( 0.000000000000000000, 0.000000000000000000, 1.000000000000000000 ) ) ;
#11455 = DIRECTION ( 'NONE',  ( 0.7071067811865389130, -0.7071067811865561215, 0.000000000000000000 ) ) ;
#11456 = EDGE_LOOP ( 'NONE', ( #23334, #18031, #9800, #33838 ) ) ;
#11457 = ORIENTED_EDGE ( 'NONE', *, *, #1156, .T. ) ;
#11458 = DIRECTION ( 'NONE',  ( 1.000000000000000000, 0.000000000000000000, 0.000000000000000000 ) ) ;
#11459 = DIRECTION ( 'NONE',  ( 1.000000000000000000, 0.000000000000000000, 0.000000000000000000 ) ) ;
#11460 = ADVANCED_FACE ( 'NONE', ( #17054 ), #1106, .T. ) ;
#11461 = ORIENTED_EDGE ( 'NONE', *, *, #29393, .T. ) ;
#11462 = AXIS2_PLACEMENT_3D ( 'NONE', #35898, #32686, #7014 ) ;
#11463 = EDGE_CURVE ( 'NONE', #4556, #8464, #33952, .T. ) ;
#11464 = AXIS2_PLACEMENT_3D ( 'NONE', #21577, #13685, #36571 ) ;
#11465 = DIRECTION ( 'NONE',  ( -1.000000000000000000, 0.000000000000000000, 0.000000000000000000 ) ) ;
#11466 = ORIENTED_EDGE ( 'NONE', *, *, #13781, .T. ) ;
#11467 = DIRECTION ( 'NONE',  ( 0.000000000000000000, 0.000000000000000000, 1.000000000000000000 ) ) ;
#11468 = EDGE_CURVE ( 'NONE', #18680, #22239, #13497, .T. ) ;
#11469 = DIRECTION ( 'NONE',  ( 0.000000000000000000, 0.000000000000000000, 1.000000000000000000 ) ) ;
#11470 = CARTESIAN_POINT ( 'NONE',  ( -28.99999999999999289, 103.4105893997321886, -19.99999999999999645 ) ) ;
#11471 = ORIENTED_EDGE ( 'NONE', *, *, #28621, .F. ) ;
#11472 = ORIENTED_EDGE ( 'NONE', *, *, #5789, .F. ) ;
#11473 = EDGE_CURVE ( 'NONE', #20787, #32385, #5272, .T. ) ;
#11474 = DIRECTION ( 'NONE',  ( 1.000000000000000000, 0.000000000000000000, 0.000000000000000000 ) ) ;
#11475 = EDGE_CURVE ( 'NONE', #21946, #4196, #37041, .T. ) ;
#11476 = CARTESIAN_POINT ( 'NONE',  ( 54.99999662536844625, -60.62177826491080168, -9.999999999999998224 ) ) ;
#11477 = CARTESIAN_POINT ( 'NONE',  ( -2.000003374631289521, -69.28203230275519786, 12.50000000000000000 ) ) ;
#11478 = ORIENTED_EDGE ( 'NONE', *, *, #21431, .T. ) ;
#11479 = DIRECTION ( 'NONE',  ( 0.000000000000000000, 0.000000000000000000, 1.000000000000000000 ) ) ;
#11480 = FACE_BOUND ( 'NONE', #28370, .T. ) ;
#11481 = DIRECTION ( 'NONE',  ( -0.000000000000000000, -0.000000000000000000, 1.000000000000000000 ) ) ;
#11482 = DIRECTION ( 'NONE',  ( 0.000000000000000000, 0.000000000000000000, 1.000000000000000000 ) ) ;
#11483 = CARTESIAN_POINT ( 'NONE',  ( 84.99999662536831124, -25.98076211353319565, -5.000000000000000000 ) ) ;
#11484 = EDGE_CURVE ( 'NONE', #17803, #5817, #7894, .T. ) ;
#11485 = DIRECTION ( 'NONE',  ( 0.000000000000000000, 0.000000000000000000, -1.000000000000000000 ) ) ;
#11486 = EDGE_CURVE ( 'NONE', #36783, #2687, #16698, .T. ) ;
#11487 = DIRECTION ( 'NONE',  ( 0.000000000000000000, 0.000000000000000000, 1.000000000000000000 ) ) ;
#11488 = EDGE_CURVE ( 'NONE', #21436, #5553, #22687, .T. ) ;
#11489 = VECTOR ( 'NONE', #1517, 1000.000000000000000 ) ;
#11490 = EDGE_CURVE ( 'NONE', #3670, #16108, #10700, .T. ) ;
#11491 = DIRECTION ( 'NONE',  ( 0.000000000000000000, 0.000000000000000000, 1.000000000000000000 ) ) ;
#11492 = EDGE_LOOP ( 'NONE', ( #9012, #9489 ) ) ;
#11493 = EDGE_CURVE ( 'NONE', #6819, #15973, #13701, .T. ) ;
#11494 = DIRECTION ( 'NONE',  ( 1.000000000000000000, 0.000000000000000000, 0.000000000000000000 ) ) ;
#11495 = CARTESIAN_POINT ( 'NONE',  ( -3.750000000000001776, 4.592425496802576930E-16, 3.400000000000000355 ) ) ;
#11496 = CARTESIAN_POINT ( 'NONE',  ( -68.00000337463102085, -51.96152422706641971, -9.999999999999998224 ) ) ;
#11497 = ORIENTED_EDGE ( 'NONE', *, *, #33699, .T. ) ;
#11498 = ORIENTED_EDGE ( 'NONE', *, *, #28790, .F. ) ;
#11499 = ORIENTED_EDGE ( 'NONE', *, *, #31222, .T. ) ;
#11500 = DIRECTION ( 'NONE',  ( 1.000000000000000000, -8.673617379884035472E-16, 0.000000000000000000 ) ) ;
#11501 = DIRECTION ( 'NONE',  ( 0.000000000000000000, 0.000000000000000000, 1.000000000000000000 ) ) ;
#11502 = DIRECTION ( 'NONE',  ( -1.000000000000000000, 0.000000000000000000, 0.000000000000000000 ) ) ;
#11503 = EDGE_LOOP ( 'NONE', ( #11045, #8504 ) ) ;
#11504 = CYLINDRICAL_SURFACE ( 'NONE', #21495, 2.000000000000001776 ) ;
#11505 = ORIENTED_EDGE ( 'NONE', *, *, #8019, .T. ) ;
#11506 = CARTESIAN_POINT ( 'NONE',  ( 69.99999662536838230, -34.64101615137759183, 17.49999999999999645 ) ) ;
#11507 = ORIENTED_EDGE ( 'NONE', *, *, #12224, .T. ) ;
#11508 = DIRECTION ( 'NONE',  ( -1.000000000000000000, 0.000000000000000000, 0.000000000000000000 ) ) ;
#11509 = ORIENTED_EDGE ( 'NONE', *, *, #32186, .T. ) ;
#11510 = ORIENTED_EDGE ( 'NONE', *, *, #36946, .F. ) ;
#11511 = DIRECTION ( 'NONE',  ( -0.000000000000000000, -0.000000000000000000, 1.000000000000000000 ) ) ;
#11512 = CARTESIAN_POINT ( 'NONE',  ( 54.99999662536846046, -43.30127018922200222, -5.000000000000000000 ) ) ;
#11513 = VECTOR ( 'NONE', #10889, 1000.000000000000000 ) ;
#11514 = CARTESIAN_POINT ( 'NONE',  ( -48.00000337463109190, 51.96152422706637708, 17.49999999999999645 ) ) ;
#11515 = ORIENTED_EDGE ( 'NONE', *, *, #36729, .F. ) ;
#11516 = DIRECTION ( 'NONE',  ( 0.000000000000000000, 0.000000000000000000, 1.000000000000000000 ) ) ;
#11517 = CARTESIAN_POINT ( 'NONE',  ( -124.4080600076932370, -12.15049814296501829, 32.50000000000000000 ) ) ;
#11518 = CARTESIAN_POINT ( 'NONE',  ( 3.035766082959412415E-15, 5.773502691896260863, -2.080000000000000071 ) ) ;
#11519 = EDGE_LOOP ( 'NONE', ( #21486, #32285 ) ) ;
#11520 = CARTESIAN_POINT ( 'NONE',  ( 74.99999662536836809, 25.98076211353319565, -5.000000000000000000 ) ) ;
#11521 = CYLINDRICAL_SURFACE ( 'NONE', #19780, 3.499999999999996003 ) ;
#11522 = EDGE_LOOP ( 'NONE', ( #21753, #13687, #6837 ) ) ;
#11523 = CARTESIAN_POINT ( 'NONE',  ( -34.00000000000027711, -58.88972745734168512, 12.49999999999999822 ) ) ;
#11524 = CARTESIAN_POINT ( 'NONE',  ( 79.99999662536833966, -3.469446951953614189E-15, -9.999999999999998224 ) ) ;
#11525 = DIRECTION ( 'NONE',  ( -0.000000000000000000, -0.000000000000000000, 1.000000000000000000 ) ) ;
#11526 = CARTESIAN_POINT ( 'NONE',  ( 58.88972745734179171, -34.00000000000007105, -4.999999999999997335 ) ) ;
#11527 = AXIS2_PLACEMENT_3D ( 'NONE', #27774, #4919, #36429 ) ;
#11528 = EDGE_CURVE ( 'NONE', #12630, #3592, #31298, .T. ) ;
#11529 = EDGE_LOOP ( 'NONE', ( #9621, #19724, #7759, #24870 ) ) ;
#11530 = DIRECTION ( 'NONE',  ( 1.000000000000000000, 0.000000000000000000, 0.000000000000000000 ) ) ;
#11531 = CARTESIAN_POINT ( 'NONE',  ( -3.374631327851540519E-06, 86.60254037844397601, -9.999999999999998224 ) ) ;
#11532 = EDGE_LOOP ( 'NONE', ( #11944, #3653, #28754, #11904, #13037, #3372 ) ) ;
#11533 = ORIENTED_EDGE ( 'NONE', *, *, #28190, .F. ) ;
#11534 = ORIENTED_EDGE ( 'NONE', *, *, #20142, .T. ) ;
#11535 = AXIS2_PLACEMENT_3D ( 'NONE', #33733, #13846, #25292 ) ;
#11536 = LINE ( 'NONE', #25819, #7651 ) ;
#11537 = AXIS2_PLACEMENT_3D ( 'NONE', #27463, #4598, #13773 ) ;
#11538 = CARTESIAN_POINT ( 'NONE',  ( -32.00000337463118427, 69.28203230275516944, -9.999999999999998224 ) ) ;
#11539 = VERTEX_POINT ( 'NONE', #36203 ) ;
#11540 = CARTESIAN_POINT ( 'NONE',  ( 6.999996625368676284, -77.94228634059960825, -5.000000000000000000 ) ) ;
#11541 = EDGE_LOOP ( 'NONE', ( #21019, #24890, #33226, #21610 ) ) ;
#11542 = APPLICATION_CONTEXT ( 'automotive_design' ) ;
#11543 = FACE_OUTER_BOUND ( 'NONE', #11841, .T. ) ;
#11544 = ORIENTED_EDGE ( 'NONE', *, *, #17408, .T. ) ;
#11545 = DIRECTION ( 'NONE',  ( 0.000000000000000000, 0.000000000000000000, 1.000000000000000000 ) ) ;
#11546 = ADVANCED_FACE ( 'NONE', ( #10508 ), #548, .F. ) ;
#11547 = VECTOR ( 'NONE', #30174, 1000.000000000000000 ) ;
#11548 = DIRECTION ( 'NONE',  ( -0.7071067811865487940, -0.7071067811865463515, 0.000000000000000000 ) ) ;
#11549 = FACE_BOUND ( 'NONE', #17559, .T. ) ;
#11550 = ORIENTED_EDGE ( 'NONE', *, *, #26528, .F. ) ;
#11551 = CARTESIAN_POINT ( 'NONE',  ( 0.000000000000000000, 0.000000000000000000, 0.000000000000000000 ) ) ;
#11552 = CARTESIAN_POINT ( 'NONE',  ( 54.99999662536844625, 43.30127018922198801, -9.999999999999998224 ) ) ;
#11553 = EDGE_CURVE ( 'NONE', #8910, #25432, #11429, .T. ) ;
#11554 = AXIS2_PLACEMENT_3D ( 'NONE', #25032, #10220, #8131 ) ;
#11555 = DIRECTION ( 'NONE',  ( -1.000000000000000000, 0.000000000000000000, 0.000000000000000000 ) ) ;
#11556 = CARTESIAN_POINT ( 'NONE',  ( 71.99999662536838230, -51.96152422706639840, 12.50000000000000000 ) ) ;
#11557 = ORIENTED_EDGE ( 'NONE', *, *, #10835, .F. ) ;
#11558 = CARTESIAN_POINT ( 'NONE',  ( -22.00000337463122690, 86.60254037844397601, 17.49999999999999645 ) ) ;
#11559 = DIRECTION ( 'NONE',  ( 0.000000000000000000, 0.000000000000000000, 1.000000000000000000 ) ) ;
#11560 = CARTESIAN_POINT ( 'NONE',  ( 49.99999662536846756, 69.28203230275516944, 12.50000000000000000 ) ) ;
#11561 = VERTEX_POINT ( 'NONE', #22875 ) ;
#11562 = ORIENTED_EDGE ( 'NONE', *, *, #33038, .F. ) ;
#11563 = ADVANCED_FACE ( 'NONE', ( #20786 ), #5331, .T. ) ;
#11564 = ORIENTED_EDGE ( 'NONE', *, *, #5568, .T. ) ;
#11565 = CIRCLE ( 'NONE', #10382, 2.000000000000001776 ) ;
#11566 = DIRECTION ( 'NONE',  ( -0.4415113423096792000, 0.000000000000000000, -0.8972556684757725387 ) ) ;
#11567 = FACE_OUTER_BOUND ( 'NONE', #13450, .T. ) ;
#11568 = CARTESIAN_POINT ( 'NONE',  ( -10.00000337463128197, 86.60254037844397601, 17.49999999999999645 ) ) ;
#11569 = CARTESIAN_POINT ( 'NONE',  ( -107.2751058113818203, -48.40472568396508279, 32.49999999999998579 ) ) ;
#11570 = FACE_OUTER_BOUND ( 'NONE', #33701, .T. ) ;
#11571 = CARTESIAN_POINT ( 'NONE',  ( -5.253679200383968073, 3.068495724078392328, -4.366070770724005179 ) ) ;
#11572 = VERTEX_POINT ( 'NONE', #34865 ) ;
#11573 = CIRCLE ( 'NONE', #28952, 2.000000000000001776 ) ;
#11574 = ORIENTED_EDGE ( 'NONE', *, *, #19844, .F. ) ;
#11575 = CARTESIAN_POINT ( 'NONE',  ( -7.000003374631307729, 77.94228634059957983, -9.999999999999998224 ) ) ;
#11576 = VECTOR ( 'NONE', #25382, 1000.000000000000000 ) ;
#11577 = EDGE_CURVE ( 'NONE', #28556, #14157, #8898, .T. ) ;
#11578 = CARTESIAN_POINT ( 'NONE',  ( 74.99999662536836809, 8.660254037844394404, -9.999999999999998224 ) ) ;
#11579 = DIRECTION ( 'NONE',  ( 1.000000000000000000, 0.000000000000000000, 0.000000000000000000 ) ) ;
#11580 = VERTEX_POINT ( 'NONE', #8612 ) ;
#11581 = EDGE_CURVE ( 'NONE', #4400, #24614, #6164, .T. ) ;
#11582 = AXIS2_PLACEMENT_3D ( 'NONE', #35176, #32908, #34977 ) ;
#11583 = DIRECTION ( 'NONE',  ( 1.000000000000000000, 0.000000000000000000, 0.000000000000000000 ) ) ;
#11584 = EDGE_LOOP ( 'NONE', ( #3640, #30506 ) ) ;
#11585 = VERTEX_POINT ( 'NONE', #9154 ) ;
#11586 = EDGE_CURVE ( 'NONE', #10997, #21808, #27446, .T. ) ;
#11587 = CYLINDRICAL_SURFACE ( 'NONE', #21845, 2.000000000000001776 ) ;
#11588 = EDGE_LOOP ( 'NONE', ( #14516, #14141 ) ) ;
#11589 =( NAMED_UNIT ( * ) SI_UNIT ( $, .STERADIAN. ) SOLID_ANGLE_UNIT ( ) );
#11590 = AXIS2_PLACEMENT_3D ( 'NONE', #23968, #30314, #15524 ) ;
#11591 = LINE ( 'NONE', #35251, #4479 ) ;
#11592 = EDGE_CURVE ( 'NONE', #27431, #31117, #10112, .T. ) ;
#11593 = FACE_OUTER_BOUND ( 'NONE', #5747, .T. ) ;
#11594 = ORIENTED_EDGE ( 'NONE', *, *, #30380, .T. ) ;
#11595 = ORIENTED_EDGE ( 'NONE', *, *, #26535, .T. ) ;
#11596 = ORIENTED_EDGE ( 'NONE', *, *, #1810, .F. ) ;
#11597 = AXIS2_PLACEMENT_3D ( 'NONE', #9764, #30386, #24963 ) ;
#11598 = ORIENTED_EDGE ( 'NONE', *, *, #489, .F. ) ;
#11599 = ORIENTED_EDGE ( 'NONE', *, *, #11222, .T. ) ;
#11600 = CARTESIAN_POINT ( 'NONE',  ( 34.99999662536853862, 77.94228634059959404, -9.999999999999998224 ) ) ;
#11601 = MECHANICAL_DESIGN_GEOMETRIC_PRESENTATION_REPRESENTATION (  '', ( #20571 ), #29563 ) ;
#11602 = SURFACE_STYLE_USAGE ( .BOTH. , #17063 ) ;
#11603 = CARTESIAN_POINT ( 'NONE',  ( 57.99999662536842493, 51.96152422706639129, -9.999999999999998224 ) ) ;
#11604 = CARTESIAN_POINT ( 'NONE',  ( -65.00000337463106348, -60.62177826491083010, -9.999999999999998224 ) ) ;
#11605 = CARTESIAN_POINT ( 'NONE',  ( -37.50000000000000000, 103.4105893997321743, 27.50000000000000000 ) ) ;
#11606 = ORIENTED_EDGE ( 'NONE', *, *, #21588, .T. ) ;
#11607 = FACE_OUTER_BOUND ( 'NONE', #15380, .T. ) ;
#11608 = ADVANCED_FACE ( 'NONE', ( #28681 ), #3171, .F. ) ;
#11609 = DIRECTION ( 'NONE',  ( -0.000000000000000000, -0.000000000000000000, -1.000000000000000000 ) ) ;
#11610 = FACE_OUTER_BOUND ( 'NONE', #19736, .T. ) ;
#11611 = VERTEX_POINT ( 'NONE', #6349 ) ;
#11612 = CARTESIAN_POINT ( 'NONE',  ( 29.99999662536857770, -69.28203230275519786, -5.000000000000000000 ) ) ;
#11613 = LINE ( 'NONE', #23068, #12999 ) ;
#11614 = ORIENTED_EDGE ( 'NONE', *, *, #11086, .F. ) ;
#11615 = EDGE_CURVE ( 'NONE', #16140, #11035, #31061, .T. ) ;
#11616 = AXIS2_PLACEMENT_3D ( 'NONE', #22080, #31239, #2187 ) ;
#11617 = EDGE_LOOP ( 'NONE', ( #25794, #23049, #24632, #26068 ) ) ;
#11618 = CARTESIAN_POINT ( 'NONE',  ( -5.000000000000000000, 30.00000000000000355, -15.00000000000000000 ) ) ;
#11619 = EDGE_CURVE ( 'NONE', #32887, #17624, #26238, .T. ) ;
#11620 = DIRECTION ( 'NONE',  ( 0.000000000000000000, 0.000000000000000000, 1.000000000000000000 ) ) ;
#11621 = CARTESIAN_POINT ( 'NONE',  ( 3.000000000000000000, 2.935248768560057453, -3.903127820947815962E-15 ) ) ;
#11622 = DIRECTION ( 'NONE',  ( 0.000000000000000000, 0.000000000000000000, -1.000000000000000000 ) ) ;
#11623 = ORIENTED_EDGE ( 'NONE', *, *, #13549, .F. ) ;
#11624 = VERTEX_POINT ( 'NONE', #25699 ) ;
#11625 = AXIS2_PLACEMENT_3D ( 'NONE', #7287, #24158, #30537 ) ;
#11626 = FACE_OUTER_BOUND ( 'NONE', #16115, .T. ) ;
#11627 = DIRECTION ( 'NONE',  ( 1.000000000000000000, 0.000000000000000000, 0.000000000000000000 ) ) ;
#11628 = AXIS2_PLACEMENT_3D ( 'NONE', #21340, #10106, #9341 ) ;
#11629 = CARTESIAN_POINT ( 'NONE',  ( 0.000000000000000000, 89.94802294027088863, -23.27834620192013304 ) ) ;
#11630 = AXIS2_PLACEMENT_3D ( 'NONE', #18004, #35455, #26994 ) ;
#11631 = VERTEX_POINT ( 'NONE', #3007 ) ;
#11632 = CARTESIAN_POINT ( 'NONE',  ( 145.0000000000000284, -6.000000000000504485, 32.55002500000000509 ) ) ;
#11633 = ORIENTED_EDGE ( 'NONE', *, *, #20060, .F. ) ;
#11634 = ORIENTED_EDGE ( 'NONE', *, *, #29123, .F. ) ;
#11635 = DIRECTION ( 'NONE',  ( -0.000000000000000000, -0.000000000000000000, 1.000000000000000000 ) ) ;
#11636 = ADVANCED_FACE ( 'NONE', ( #8991, #17792, #20419, #14430, #29227, #3557, #11593 ), #35044, .F. ) ;
#11637 = VECTOR ( 'NONE', #35452, 1000.000000000000000 ) ;
#11638 = LINE ( 'NONE', #397, #17254 ) ;
#11639 = VERTEX_POINT ( 'NONE', #6006 ) ;
#11640 = AXIS2_PLACEMENT_3D ( 'NONE', #1293, #15360, #15918 ) ;
#11641 = VERTEX_POINT ( 'NONE', #32223 ) ;
#11642 = LINE ( 'NONE', #2875, #31634 ) ;
#11643 = CARTESIAN_POINT ( 'NONE',  ( 64.99999662536841072, -25.98076211353320275, -9.999999999999998224 ) ) ;
#11644 = CARTESIAN_POINT ( 'NONE',  ( 68.17080445151383117, -51.15278694518232072, 12.50000000000000000 ) ) ;
#11645 = AXIS2_PLACEMENT_3D ( 'NONE', #29054, #11996, #6579 ) ;
#11646 = VERTEX_POINT ( 'NONE', #29410 ) ;
#11647 = CARTESIAN_POINT ( 'NONE',  ( -17.00000337463125533, -77.94228634059960825, -9.999999999999998224 ) ) ;
#11648 = FACE_BOUND ( 'NONE', #10762, .T. ) ;
#11649 = CYLINDRICAL_SURFACE ( 'NONE', #16061, 2.000000000000001776 ) ;
#11650 = CYLINDRICAL_SURFACE ( 'NONE', #36078, 25.00000000000000000 ) ;
#11651 = LINE ( 'NONE', #34560, #5136 ) ;
#11652 = CARTESIAN_POINT ( 'NONE',  ( 0.000000000000000000, 0.000000000000000000, -5.000000000000000000 ) ) ;
#11653 = CIRCLE ( 'NONE', #35039, 95.00000000000001421 ) ;
#11654 = EDGE_CURVE ( 'NONE', #4310, #6715, #3423, .T. ) ;
#11655 = SURFACE_STYLE_FILL_AREA ( #614 ) ;
#11656 = DIRECTION ( 'NONE',  ( 0.000000000000000000, 0.000000000000000000, 1.000000000000000000 ) ) ;
#11657 = EDGE_LOOP ( 'NONE', ( #18495, #16845 ) ) ;
#11658 = EDGE_CURVE ( 'NONE', #22247, #24345, #35863, .T. ) ;
#11659 = CARTESIAN_POINT ( 'NONE',  ( 0.000000000000000000, 89.94802294027088863, 27.49999999999999645 ) ) ;
#11660 = FACE_BOUND ( 'NONE', #22903, .T. ) ;
#11661 = DIRECTION ( 'NONE',  ( 0.000000000000000000, 0.000000000000000000, -1.000000000000000000 ) ) ;
#11662 = ORIENTED_EDGE ( 'NONE', *, *, #6901, .F. ) ;
#11663 = ADVANCED_FACE ( 'NONE', ( #23241 ), #31831, .F. ) ;
#11664 = ORIENTED_EDGE ( 'NONE', *, *, #24969, .F. ) ;
#11665 = ORIENTED_EDGE ( 'NONE', *, *, #932, .F. ) ;
#11666 = AXIS2_PLACEMENT_3D ( 'NONE', #4813, #30487, #13047 ) ;
#11667 = EDGE_CURVE ( 'NONE', #18343, #24428, #13690, .T. ) ;
#11668 = FACE_OUTER_BOUND ( 'NONE', #9901, .T. ) ;
#11669 = CARTESIAN_POINT ( 'NONE',  ( -90.00000337463090716, -1.040834085586084257E-14, -9.999999999999998224 ) ) ;
#11670 = AXIS2_PLACEMENT_3D ( 'NONE', #16817, #5548, #16977 ) ;
#11671 = EDGE_CURVE ( 'NONE', #31731, #7037, #15909, .T. ) ;
#11672 = CARTESIAN_POINT ( 'NONE',  ( 67.99999662536838230, 34.64101615137758472, -9.999999999999998224 ) ) ;
#11673 = ORIENTED_EDGE ( 'NONE', *, *, #31399, .F. ) ;
#11674 = EDGE_CURVE ( 'NONE', #27674, #14720, #10114, .T. ) ;
#11675 = AXIS2_PLACEMENT_3D ( 'NONE', #25642, #3296, #31247 ) ;
#11676 = CIRCLE ( 'NONE', #33237, 3.250000000000001332 ) ;
#11677 = CARTESIAN_POINT ( 'NONE',  ( 37.99999662536853151, 69.28203230275518365, -9.999999999999998224 ) ) ;
#11678 = ORIENTED_EDGE ( 'NONE', *, *, #19482, .F. ) ;
#11679 = CARTESIAN_POINT ( 'NONE',  ( 8.711340810219693864, -118.4423164015428256, 32.50000000000000711 ) ) ;
#11680 = ORIENTED_EDGE ( 'NONE', *, *, #27848, .T. ) ;
#11681 = DIRECTION ( 'NONE',  ( 1.000000000000000000, 0.000000000000000000, 0.000000000000000000 ) ) ;
#11682 = AXIS2_PLACEMENT_3D ( 'NONE', #9672, #12652, #9492 ) ;
#11683 = EDGE_LOOP ( 'NONE', ( #32747, #32569, #23400, #19443 ) ) ;
#11684 = EDGE_CURVE ( 'NONE', #17723, #22036, #25110, .T. ) ;
#11685 = CIRCLE ( 'NONE', #14101, 2.000000000000001776 ) ;
#11686 = ORIENTED_EDGE ( 'NONE', *, *, #36830, .T. ) ;
#11687 = CIRCLE ( 'NONE', #17690, 30.00000000000001421 ) ;
#11688 = EDGE_CURVE ( 'NONE', #22983, #16313, #18910, .T. ) ;
#11689 = FACE_OUTER_BOUND ( 'NONE', #12583, .T. ) ;
#11690 = EDGE_CURVE ( 'NONE', #7273, #10178, #10724, .T. ) ;
#11691 = DIRECTION ( 'NONE',  ( 1.000000000000000000, 0.000000000000000000, 0.000000000000000000 ) ) ;
#11692 = VERTEX_POINT ( 'NONE', #26976 ) ;
#11693 = CARTESIAN_POINT ( 'NONE',  ( -13.00000337463126066, 77.94228634059957983, -9.999999999999998224 ) ) ;
#11694 = FACE_OUTER_BOUND ( 'NONE', #28773, .T. ) ;
#11695 = CARTESIAN_POINT ( 'NONE',  ( 26.99999662536859546, -77.94228634059960825, 12.50000000000000000 ) ) ;
#11696 = CIRCLE ( 'NONE', #25498, 2.000000000000001776 ) ;
#11697 = ORIENTED_EDGE ( 'NONE', *, *, #5340, .F. ) ;
#11698 = DIRECTION ( 'NONE',  ( 0.4999999999999919509, -0.8660254037844433705, 0.000000000000000000 ) ) ;
#11699 = CARTESIAN_POINT ( 'NONE',  ( 4.999999999999999112, 2.886751345948125991, -5.700000000000000178 ) ) ;
#11700 = ORIENTED_EDGE ( 'NONE', *, *, #26945, .F. ) ;
#11701 = CARTESIAN_POINT ( 'NONE',  ( 3.108933952041194271, 78.59334852315024023, -5.000000000000000000 ) ) ;
#11702 = AXIS2_PLACEMENT_3D ( 'NONE', #5134, #28359, #5880 ) ;
#11703 = CARTESIAN_POINT ( 'NONE',  ( -60.00000337463104216, 51.96152422706639129, -9.999999999999998224 ) ) ;
#11704 = DIRECTION ( 'NONE',  ( -0.4999999999999968359, 0.8660254037844404840, 0.000000000000000000 ) ) ;
#11705 = CIRCLE ( 'NONE', #30291, 150.0000000000000284 ) ;
#11706 = VECTOR ( 'NONE', #36061, 1000.000000000000000 ) ;
#11707 = CIRCLE ( 'NONE', #4558, 2.000000000000000000 ) ;
#11708 = FACE_OUTER_BOUND ( 'NONE', #28053, .T. ) ;
#11709 = AXIS2_PLACEMENT_3D ( 'NONE', #6484, #20356, #3285 ) ;
#11710 = EDGE_CURVE ( 'NONE', #35393, #4661, #19115, .T. ) ;
#11711 = LINE ( 'NONE', #1027, #19136 ) ;
#11712 = ORIENTED_EDGE ( 'NONE', *, *, #1865, .F. ) ;
#11713 = EDGE_CURVE ( 'NONE', #36735, #22867, #25280, .T. ) ;
#11714 = CARTESIAN_POINT ( 'NONE',  ( 3.000000000000000000, 3.113052163432572109E-16, -2.541999999999999815 ) ) ;
#11715 = CARTESIAN_POINT ( 'NONE',  ( -83.45172111230354517, 31.46585318596159553, -49.86348611802629449 ) ) ;
#11716 = ORIENTED_EDGE ( 'NONE', *, *, #33042, .T. ) ;
#11717 = ORIENTED_EDGE ( 'NONE', *, *, #29987, .F. ) ;
#11718 = VERTEX_POINT ( 'NONE', #27342 ) ;
#11719 = DIRECTION ( 'NONE',  ( -1.000000000000000000, 0.000000000000000000, 0.000000000000000000 ) ) ;
#11720 = CARTESIAN_POINT ( 'NONE',  ( 2.500000000000000000, 0.000000000000000000, -0.3501037691048548561 ) ) ;
#11721 = EDGE_CURVE ( 'NONE', #12419, #13800, #35254, .T. ) ;
#11722 = CARTESIAN_POINT ( 'NONE',  ( 4.279621169095998212, -62.97617850287780072, -4.999999999999997335 ) ) ;
#11723 = VECTOR ( 'NONE', #16209, 1000.000000000000000 ) ;
#11724 = AXIS2_PLACEMENT_3D ( 'NONE', #18833, #10020, #7573 ) ;
#11725 = DIRECTION ( 'NONE',  ( 0.000000000000000000, 0.000000000000000000, 1.000000000000000000 ) ) ;
#11726 = ORIENTED_EDGE ( 'NONE', *, *, #21070, .F. ) ;
#11727 = VECTOR ( 'NONE', #22331, 1000.000000000000000 ) ;
#11728 = DIRECTION ( 'NONE',  ( 0.000000000000000000, 0.000000000000000000, 1.000000000000000000 ) ) ;
#11729 = ORIENTED_EDGE ( 'NONE', *, *, #32497, .T. ) ;
#11730 = FACE_BOUND ( 'NONE', #13483, .T. ) ;
#11731 = EDGE_CURVE ( 'NONE', #15417, #32452, #11310, .T. ) ;
#11732 = AXIS2_PLACEMENT_3D ( 'NONE', #35467, #32828, #4509 ) ;
#11733 = AXIS2_PLACEMENT_3D ( 'NONE', #26713, #12457, #23926 ) ;
#11734 = ADVANCED_FACE ( 'NONE', ( #12706 ), #29975, .T. ) ;
#11735 = FACE_OUTER_BOUND ( 'NONE', #17421, .T. ) ;
#11736 = EDGE_CURVE ( 'NONE', #8155, #23009, #27503, .T. ) ;
#11737 = EDGE_CURVE ( 'NONE', #8275, #16746, #6544, .T. ) ;
#11738 = LINE ( 'NONE', #25654, #5917 ) ;
#11739 = LINE ( 'NONE', #9507, #17061 ) ;
#11740 = DIRECTION ( 'NONE',  ( -0.6664934940021893794, 0.7455108466365553133, 0.000000000000000000 ) ) ;
#11741 = AXIS2_PLACEMENT_3D ( 'NONE', #247, #34591, #29121 ) ;
#11742 = CARTESIAN_POINT ( 'NONE',  ( -12.00000337463125000, -86.60254037844400443, 12.50000000000000000 ) ) ;
#11743 = FACE_OUTER_BOUND ( 'NONE', #18573, .T. ) ;
#11744 = CARTESIAN_POINT ( 'NONE',  ( -12.00000337463128197, 86.60254037844397601, -9.999999999999998224 ) ) ;
#11745 = EDGE_LOOP ( 'NONE', ( #15513, #5385, #5061 ) ) ;
#11746 = CARTESIAN_POINT ( 'NONE',  ( 27.99999662536857414, -69.28203230275519786, -9.999999999999998224 ) ) ;
#11747 = DIRECTION ( 'NONE',  ( 0.000000000000000000, 0.000000000000000000, 1.000000000000000000 ) ) ;
#11748 = CYLINDRICAL_SURFACE ( 'NONE', #26120, 2.000000000000001776 ) ;
#11749 = CIRCLE ( 'NONE', #2806, 27.00000000000001421 ) ;
#11750 = ORIENTED_EDGE ( 'NONE', *, *, #27556, .F. ) ;
#11751 = VERTEX_POINT ( 'NONE', #32587 ) ;
#11752 = ORIENTED_EDGE ( 'NONE', *, *, #2375, .T. ) ;
#11753 = AXIS2_PLACEMENT_3D ( 'NONE', #28808, #20007, #25656 ) ;
#11754 = CARTESIAN_POINT ( 'NONE',  ( -102.5304832720503185, -102.5304832720485280, 27.50000000000000000 ) ) ;
#11755 = AXIS2_PLACEMENT_3D ( 'NONE', #9682, #21107, #16053 ) ;
#11756 = EDGE_CURVE ( 'NONE', #24284, #698, #31660, .T. ) ;
#11757 = CIRCLE ( 'NONE', #31514, 2.000000000000001776 ) ;
#11758 = DIRECTION ( 'NONE',  ( 1.000000000000000000, 0.000000000000000000, 0.000000000000000000 ) ) ;
#11759 = VECTOR ( 'NONE', #24692, 1000.000000000000000 ) ;
#11760 = CARTESIAN_POINT ( 'NONE',  ( -43.00000337463111322, -77.94228634059960825, -5.000000000000000000 ) ) ;
#11761 = DIRECTION ( 'NONE',  ( 0.7071067811865414665, -0.7071067811865536790, -0.000000000000000000 ) ) ;
#11762 = DIRECTION ( 'NONE',  ( -0.000000000000000000, -0.000000000000000000, -1.000000000000000000 ) ) ;
#11763 = CARTESIAN_POINT ( 'NONE',  ( -37.50000000000000000, 103.4105893997321886, -19.99999999999999645 ) ) ;
#11764 = EDGE_LOOP ( 'NONE', ( #9499, #9712 ) ) ;
#11765 = CIRCLE ( 'NONE', #13604, 2.000000000000001776 ) ;
#11766 = ORIENTED_EDGE ( 'NONE', *, *, #7083, .T. ) ;
#11767 = LINE ( 'NONE', #14778, #26059 ) ;
#11768 = CARTESIAN_POINT ( 'NONE',  ( -55.00000337463107059, 60.62177826491078747, 17.49999999999999645 ) ) ;
#11769 = CARTESIAN_POINT ( 'NONE',  ( 56.99999662536844625, -60.62177826491080168, 17.49999999999999645 ) ) ;
#11770 = ORIENTED_EDGE ( 'NONE', *, *, #873, .T. ) ;
#11771 = AXIS2_PLACEMENT_3D ( 'NONE', #13289, #7125, #29797 ) ;
#11772 = FACE_BOUND ( 'NONE', #26523, .T. ) ;
#11773 = ORIENTED_EDGE ( 'NONE', *, *, #3439, .T. ) ;
#11774 = ORIENTED_EDGE ( 'NONE', *, *, #1532, .T. ) ;
#11775 = CLOSED_SHELL ( 'NONE', ( #33604, #34142, #3962, #15826, #19284, #33301, #7947, #2031, #36687, #2661, #10281, #32917, #7309, #35097, #15070, #4725, #30656, #23171, #19066, #14023, #16154, #18454, #36672, #29823, #33996, #6065, #10080, #36104, #15073, #13078, #26030, #2566, #19872, #14429, #14633, #6542, #5103, #6176, #17817, #654, #5106, #36704, #8282, #12953, #12007, #4272, #35436, #10761, #14375, #19961, #30173, #29363, #2219, #12487, #26316, #7116, #27552, #4331, #21100, #15115, #21843, #28450, #31480, #34181, #29356, #13920, #7530, #28891, #1972, #18720, #2271, #36617, #24782, #28348, #31788, #2783, #9926, #26505, #23687, #1636, #16196, #37090, #21934, #32552, #6992, #25018, #29594, #36608, #9622, #12297 ) ) ;
#11776 = EDGE_CURVE ( 'NONE', #32947, #14483, #33484, .T. ) ;
#11777 = DIRECTION ( 'NONE',  ( 1.000000000000000000, 0.000000000000000000, 0.000000000000000000 ) ) ;
#11778 = ORIENTED_EDGE ( 'NONE', *, *, #30057, .T. ) ;
#11780 = AXIS2_PLACEMENT_3D ( 'NONE', #26138, #34950, #9071 ) ;
#11779 =( LENGTH_UNIT ( ) NAMED_UNIT ( * ) SI_UNIT ( .MILLI., .METRE. ) );
#11781 = AXIS2_PLACEMENT_3D ( 'NONE', #9179, #29047, #14621 ) ;
#11782 = DIRECTION ( 'NONE',  ( 0.000000000000000000, 0.000000000000000000, 1.000000000000000000 ) ) ;
#11783 = CIRCLE ( 'NONE', #32758, 3.500000000000003109 ) ;
#11784 = DIRECTION ( 'NONE',  ( 1.000000000000000000, 0.000000000000000000, 0.000000000000000000 ) ) ;
#11785 = VERTEX_POINT ( 'NONE', #9907 ) ;
#11786 = ORIENTED_EDGE ( 'NONE', *, *, #6461, .T. ) ;
#11787 = CIRCLE ( 'NONE', #11215, 2.000000000000001776 ) ;
#11788 = ORIENTED_EDGE ( 'NONE', *, *, #27251, .F. ) ;
#11789 = AXIS2_PLACEMENT_3D ( 'NONE', #30780, #36619, #36438 ) ;
#11790 = ORIENTED_EDGE ( 'NONE', *, *, #23458, .F. ) ;
#11791 = ORIENTED_EDGE ( 'NONE', *, *, #11943, .F. ) ;
#11792 = FACE_OUTER_BOUND ( 'NONE', #2559, .T. ) ;
#11793 = CARTESIAN_POINT ( 'NONE',  ( 9.999996625368655856, -69.28203230275519786, 12.50000000000000000 ) ) ;
#11795 = AXIS2_PLACEMENT_3D ( 'NONE', #36636, #13928, #25375 ) ;
#11794 = PLANE ( 'NONE',  #28038 ) ;
#11796 = FACE_OUTER_BOUND ( 'NONE', #10284, .T. ) ;
#11797 = CYLINDRICAL_SURFACE ( 'NONE', #7005, 2.000000000000001776 ) ;
#11798 = EDGE_CURVE ( 'NONE', #2420, #32300, #11912, .T. ) ;
#11799 = ORIENTED_EDGE ( 'NONE', *, *, #12880, .F. ) ;
#11800 = DIRECTION ( 'NONE',  ( 0.000000000000000000, 0.4999999999999953926, 0.8660254037844412611 ) ) ;
#11801 = CIRCLE ( 'NONE', #33401, 2.000000000000001776 ) ;
#11802 = CARTESIAN_POINT ( 'NONE',  ( -1.738710530748195815, -5.045296470310012715, -4.085927688751848308 ) ) ;
#11803 = CIRCLE ( 'NONE', #35182, 2.000000000000001776 ) ;
#11804 = DIRECTION ( 'NONE',  ( 0.000000000000000000, 0.000000000000000000, -1.000000000000000000 ) ) ;
#11805 = ORIENTED_EDGE ( 'NONE', *, *, #8517, .F. ) ;
#11806 = DIRECTION ( 'NONE',  ( 0.000000000000000000, 0.000000000000000000, 1.000000000000000000 ) ) ;
#11807 = CYLINDRICAL_SURFACE ( 'NONE', #35767, 2.000000000000000000 ) ;
#11808 = EDGE_LOOP ( 'NONE', ( #30782, #6258, #24348, #15052, #1531, #15638, #4167, #24906, #35974, #10557, #30982, #20568 ) ) ;
#11809 = CIRCLE ( 'NONE', #31570, 1.999999999999998224 ) ;
#11810 = ORIENTED_EDGE ( 'NONE', *, *, #10057, .T. ) ;
#11811 = AXIS2_PLACEMENT_3D ( 'NONE', #7202, #33442, #27232 ) ;
#11812 = EDGE_CURVE ( 'NONE', #26888, #6282, #27146, .T. ) ;
#11813 = FACE_OUTER_BOUND ( 'NONE', #29658, .T. ) ;
#11814 = CYLINDRICAL_SURFACE ( 'NONE', #19940, 3.000000000000002665 ) ;
#11815 = FACE_BOUND ( 'NONE', #8658, .T. ) ;
#11816 = APPLICATION_CONTEXT ( 'automotive_design' ) ;
#11817 = CARTESIAN_POINT ( 'NONE',  ( 74.30619744048946984, -84.18124734178287838, 32.50000000000000000 ) ) ;
#11818 = ORIENTED_EDGE ( 'NONE', *, *, #32675, .F. ) ;
#11819 = CIRCLE ( 'NONE', #9462, 2.000000000000001776 ) ;
#11820 = DIRECTION ( 'NONE',  ( 0.000000000000000000, 0.000000000000000000, 1.000000000000000000 ) ) ;
#11821 = DIRECTION ( 'NONE',  ( 0.000000000000000000, 0.000000000000000000, 1.000000000000000000 ) ) ;
#11822 = DIRECTION ( 'NONE',  ( 0.000000000000000000, 0.000000000000000000, 1.000000000000000000 ) ) ;
#11823 = AXIS2_PLACEMENT_3D ( 'NONE', #19188, #27607, #7543 ) ;
#11824 = ORIENTED_EDGE ( 'NONE', *, *, #19470, .F. ) ;
#11825 = ADVANCED_FACE ( 'NONE', ( #32977 ), #7289, .F. ) ;
#11826 = CIRCLE ( 'NONE', #16645, 2.000000000000001776 ) ;
#11827 = CIRCLE ( 'NONE', #32803, 3.499999999999996003 ) ;
#11828 = CARTESIAN_POINT ( 'NONE',  ( 21.99999662536857770, 86.60254037844397601, -5.000000000000000000 ) ) ;
#11829 = ORIENTED_EDGE ( 'NONE', *, *, #2245, .F. ) ;
#11830 = DIRECTION ( 'NONE',  ( -0.8660254037844379305, 0.5000000000000011102, 0.000000000000000000 ) ) ;
#11831 = DIRECTION ( 'NONE',  ( 1.000000000000000000, 0.000000000000000000, 0.000000000000000000 ) ) ;
#11832 = VECTOR ( 'NONE', #785, 1000.000000000000000 ) ;
#11833 = LINE ( 'NONE', #34740, #21454 ) ;
#11834 = ORIENTED_EDGE ( 'NONE', *, *, #24207, .T. ) ;
#11835 = ORIENTED_EDGE ( 'NONE', *, *, #2880, .F. ) ;
#11836 = DIRECTION ( 'NONE',  ( 1.000000000000000000, 0.000000000000000000, 0.000000000000000000 ) ) ;
#11837 = EDGE_CURVE ( 'NONE', #3733, #29631, #32883, .T. ) ;
#11838 = CYLINDRICAL_SURFACE ( 'NONE', #9443, 2.000000000000001776 ) ;
#11839 = DIRECTION ( 'NONE',  ( 0.000000000000000000, 0.000000000000000000, 1.000000000000000000 ) ) ;
#11840 = CIRCLE ( 'NONE', #7073, 2.000000000000001776 ) ;
#11841 = EDGE_LOOP ( 'NONE', ( #33422, #24014 ) ) ;
#11842 = DIRECTION ( 'NONE',  ( -1.000000000000000000, 0.000000000000000000, 0.000000000000000000 ) ) ;
#11843 = EDGE_CURVE ( 'NONE', #10369, #17775, #25692, .T. ) ;
#11844 = FACE_BOUND ( 'NONE', #31953, .T. ) ;
#11845 = CARTESIAN_POINT ( 'NONE',  ( -85.00000337463092137, 25.98076211353317433, -9.999999999999998224 ) ) ;
#11846 = DIRECTION ( 'NONE',  ( 0.000000000000000000, 0.000000000000000000, -1.000000000000000000 ) ) ;
#11847 = CIRCLE ( 'NONE', #2287, 2.000000000000001776 ) ;
#11848 = CARTESIAN_POINT ( 'NONE',  ( 79.99999662536833966, -3.469446951953614189E-15, -9.999999999999998224 ) ) ;
#11849 = LINE ( 'NONE', #6776, #14711 ) ;
#11850 = CYLINDRICAL_SURFACE ( 'NONE', #26952, 2.000000000000001776 ) ;
#11851 = CIRCLE ( 'NONE', #490, 2.000000000000001776 ) ;
#11852 = DIRECTION ( 'NONE',  ( 1.000000000000000000, 0.000000000000000000, 0.000000000000000000 ) ) ;
#11853 = ORIENTED_EDGE ( 'NONE', *, *, #8723, .T. ) ;
#11854 = DIRECTION ( 'NONE',  ( 1.000000000000000000, 0.000000000000000000, 0.000000000000000000 ) ) ;
#11855 = EDGE_CURVE ( 'NONE', #7880, #14355, #32251, .T. ) ;
#11856 = CIRCLE ( 'NONE', #17258, 2.000000000000000000 ) ;
#11857 = AXIS2_PLACEMENT_3D ( 'NONE', #26249, #561, #20599 ) ;
#11858 = CARTESIAN_POINT ( 'NONE',  ( -50.00000337463110611, -69.28203230275519786, 17.49999999999999645 ) ) ;
#11859 = CARTESIAN_POINT ( 'NONE',  ( -93.55673653615988883, -16.49657687835776088, -5.000000000000000000 ) ) ;
#11860 = AXIS2_PLACEMENT_3D ( 'NONE', #16617, #31047, #35166 ) ;
#11861 = EDGE_LOOP ( 'NONE', ( #27965, #30912, #35650 ) ) ;
#11862 = EDGE_LOOP ( 'NONE', ( #29221, #22870 ) ) ;
#11863 = ORIENTED_EDGE ( 'NONE', *, *, #27065, .F. ) ;
#11864 = EDGE_CURVE ( 'NONE', #16326, #10952, #11334, .T. ) ;
#11865 = CIRCLE ( 'NONE', #32839, 2.000000000000001776 ) ;
#11866 = DIRECTION ( 'NONE',  ( -0.000000000000000000, -0.000000000000000000, 1.000000000000000000 ) ) ;
#11867 = CARTESIAN_POINT ( 'NONE',  ( 89.99999662536828282, 0.000000000000000000, -9.999999999999998224 ) ) ;
#11868 = CARTESIAN_POINT ( 'NONE',  ( 64.99999662536841072, 25.98076211353318854, -9.999999999999998224 ) ) ;
#11869 = VERTEX_POINT ( 'NONE', #16842 ) ;
#11870 = AXIS2_PLACEMENT_3D ( 'NONE', #32619, #6942, #4147 ) ;
#11871 = FACE_OUTER_BOUND ( 'NONE', #31738, .T. ) ;
#11872 = EDGE_LOOP ( 'NONE', ( #30373, #7204, #15152 ) ) ;
#11873 = CARTESIAN_POINT ( 'NONE',  ( -9.904827271909082853, -117.9629806292090279, 32.50000000000000711 ) ) ;
#11874 = ORIENTED_EDGE ( 'NONE', *, *, #24575, .F. ) ;
#11875 = CARTESIAN_POINT ( 'NONE',  ( -38.00000337463113453, 69.28203230275516944, 12.50000000000000000 ) ) ;
#11876 = AXIS2_PLACEMENT_3D ( 'NONE', #25284, #11011, #22452 ) ;
#11877 = ORIENTED_EDGE ( 'NONE', *, *, #25560, .F. ) ;
#11878 = ORIENTED_EDGE ( 'NONE', *, *, #6677, .T. ) ;
#11879 = EDGE_CURVE ( 'NONE', #35442, #2346, #9518, .T. ) ;
#11880 = DIRECTION ( 'NONE',  ( 1.000000000000000000, 0.000000000000000000, 0.000000000000000000 ) ) ;
#11881 = CARTESIAN_POINT ( 'NONE',  ( 2.260257450329328233, -4.468542444510769762, -0.5197061503823295903 ) ) ;
#11882 = CIRCLE ( 'NONE', #28644, 2.000000000000001776 ) ;
#11883 = DIRECTION ( 'NONE',  ( 0.000000000000000000, 0.000000000000000000, 1.000000000000000000 ) ) ;
#11884 = EDGE_LOOP ( 'NONE', ( #20139, #26600, #8010, #11909 ) ) ;
#11885 = DIRECTION ( 'NONE',  ( -0.000000000000000000, -0.000000000000000000, 1.000000000000000000 ) ) ;
#11886 = EDGE_CURVE ( 'NONE', #6247, #24313, #13131, .T. ) ;
#11887 = CARTESIAN_POINT ( 'NONE',  ( -102.5304832720481869, 102.5304832720506596, 32.55002500000000509 ) ) ;
#11888 = DIRECTION ( 'NONE',  ( -0.8660254037844379305, 0.5000000000000011102, 0.000000000000000000 ) ) ;
#11889 = ORIENTED_EDGE ( 'NONE', *, *, #18079, .T. ) ;
#11890 = CARTESIAN_POINT ( 'NONE',  ( 17.99999662536858835, 69.28203230275516944, -9.999999999999998224 ) ) ;
#11891 = DIRECTION ( 'NONE',  ( -1.000000000000000000, 0.000000000000000000, 0.000000000000000000 ) ) ;
#11892 = AXIS2_PLACEMENT_3D ( 'NONE', #7193, #18632, #23888 ) ;
#11894 = EDGE_LOOP ( 'NONE', ( #27035, #1366, #11606, #15672 ) ) ;
#11893 = ADVANCED_FACE ( 'NONE', ( #19837 ), #30885, .F. ) ;
#11895 = DIRECTION ( 'NONE',  ( 1.000000000000000000, 0.000000000000000000, 0.000000000000000000 ) ) ;
#11896 = DIRECTION ( 'NONE',  ( 1.000000000000000000, 0.000000000000000000, 0.000000000000000000 ) ) ;
#11897 = FACE_OUTER_BOUND ( 'NONE', #23466, .T. ) ;
#11898 = AXIS2_PLACEMENT_3D ( 'NONE', #14235, #17037, #2609 ) ;
#11899 = DIRECTION ( 'NONE',  ( -0.000000000000000000, -0.000000000000000000, 1.000000000000000000 ) ) ;
#11900 = CIRCLE ( 'NONE', #7130, 3.500000000000003109 ) ;
#11901 = CIRCLE ( 'NONE', #31676, 2.000000000000000000 ) ;
#11902 = CARTESIAN_POINT ( 'NONE',  ( -92.00000337463090716, -1.016341149603137227E-14, -9.999999999999998224 ) ) ;
#11903 = FACE_OUTER_BOUND ( 'NONE', #36632, .T. ) ;
#11904 = ORIENTED_EDGE ( 'NONE', *, *, #26839, .F. ) ;
#11905 = CARTESIAN_POINT ( 'NONE',  ( -52.00000337463109190, 69.28203230275518365, 12.50000000000000000 ) ) ;
#11906 = CARTESIAN_POINT ( 'NONE',  ( -101.4249800177810812, 31.43204461044035725, 27.50000000000000000 ) ) ;
#11907 = DIRECTION ( 'NONE',  ( 0.000000000000000000, 0.000000000000000000, -1.000000000000000000 ) ) ;
#11908 = ORIENTED_EDGE ( 'NONE', *, *, #6139, .T. ) ;
#11909 = ORIENTED_EDGE ( 'NONE', *, *, #20216, .F. ) ;
#11910 = ORIENTED_EDGE ( 'NONE', *, *, #35205, .F. ) ;
#11911 = EDGE_CURVE ( 'NONE', #3013, #10982, #540, .T. ) ;
#11912 = CIRCLE ( 'NONE', #37067, 2.500000000000000000 ) ;
#11913 = CARTESIAN_POINT ( 'NONE',  ( 4.390739357591695365E-15, -5.773502691896304384, -4.069522543421433269 ) ) ;
#11914 = CARTESIAN_POINT ( 'NONE',  ( -40.00000337463113453, 69.28203230275516944, -9.999999999999998224 ) ) ;
#11915 = DIRECTION ( 'NONE',  ( 0.000000000000000000, 0.000000000000000000, 1.000000000000000000 ) ) ;
#11916 = CARTESIAN_POINT ( 'NONE',  ( -58.88972745734203329, -33.99999999999965894, -4.999999999999997335 ) ) ;
#11917 = ORIENTED_EDGE ( 'NONE', *, *, #21914, .T. ) ;
#11918 = VECTOR ( 'NONE', #4414, 1000.000000000000000 ) ;
#11919 = CARTESIAN_POINT ( 'NONE',  ( -35.00000337463117717, -77.94228634059963667, -9.999999999999998224 ) ) ;
#11920 = ORIENTED_EDGE ( 'NONE', *, *, #29566, .F. ) ;
#11921 = FACE_BOUND ( 'NONE', #18344, .T. ) ;
#11922 = VECTOR ( 'NONE', #23546, 1000.000000000000000 ) ;
#11923 = VECTOR ( 'NONE', #3896, 1000.000000000000000 ) ;
#11924 = ADVANCED_FACE ( 'NONE', ( #36894 ), #16114, .T. ) ;
#11925 = DIRECTION ( 'NONE',  ( 1.000000000000000000, 0.000000000000000000, 0.000000000000000000 ) ) ;
#11926 = FACE_OUTER_BOUND ( 'NONE', #36614, .T. ) ;
#11927 = AXIS2_PLACEMENT_3D ( 'NONE', #15269, #17713, #12243 ) ;
#11928 = ADVANCED_FACE ( 'NONE', ( #30704 ), #22105, .T. ) ;
#11929 = ORIENTED_EDGE ( 'NONE', *, *, #20142, .F. ) ;
#11930 = DIRECTION ( 'NONE',  ( 0.000000000000000000, 0.000000000000000000, 1.000000000000000000 ) ) ;
#11931 = CARTESIAN_POINT ( 'NONE',  ( -47.63139720814399425, -27.50000000000022382, 10.70000000000000107 ) ) ;
#11932 = EDGE_CURVE ( 'NONE', #9158, #18582, #10845, .T. ) ;
#11933 = DIRECTION ( 'NONE',  ( 1.000000000000000000, 0.000000000000000000, 0.000000000000000000 ) ) ;
#11934 = AXIS2_PLACEMENT_3D ( 'NONE', #5375, #27667, #2374 ) ;
#11935 = DIRECTION ( 'NONE',  ( 0.000000000000000000, -1.000000000000000000, 1.625241993126352989E-15 ) ) ;
#11936 = CARTESIAN_POINT ( 'NONE',  ( -33.00000337463117006, -77.94228634059963667, 17.49999999999999645 ) ) ;
#11937 = EDGE_LOOP ( 'NONE', ( #15481, #31902, #19447, #28043 ) ) ;
#11938 = DIRECTION ( 'NONE',  ( 0.000000000000000000, 0.000000000000000000, 1.000000000000000000 ) ) ;
#11939 = ADVANCED_FACE ( 'NONE', ( #22277 ), #22653, .F. ) ;
#11940 = AXIS2_PLACEMENT_3D ( 'NONE', #14004, #5768, #14562 ) ;
#11941 = DIRECTION ( 'NONE',  ( 0.000000000000000000, 0.000000000000000000, -1.000000000000000000 ) ) ;
#11942 = CARTESIAN_POINT ( 'NONE',  ( -20.00000337463122690, 86.60254037844397601, 17.49999999999999645 ) ) ;
#11943 = EDGE_CURVE ( 'NONE', #182, #2651, #26295, .T. ) ;
#11944 = ORIENTED_EDGE ( 'NONE', *, *, #22881, .F. ) ;
#11945 = ORIENTED_EDGE ( 'NONE', *, *, #34418, .T. ) ;
#11946 = ORIENTED_EDGE ( 'NONE', *, *, #23576, .F. ) ;
#11947 = CARTESIAN_POINT ( 'NONE',  ( 3.000000000000000000, 0.000000000000000000, 0.000000000000000000 ) ) ;
#11948 = EDGE_CURVE ( 'NONE', #23292, #21544, #36710, .T. ) ;
#11949 = EDGE_CURVE ( 'NONE', #25264, #36242, #27703, .T. ) ;
#11950 = CARTESIAN_POINT ( 'NONE',  ( 61.06482292022111125, -72.77422209630303485, 12.49999999999999822 ) ) ;
#11951 = EDGE_CURVE ( 'NONE', #731, #1473, #10140, .T. ) ;
#11952 = EDGE_CURVE ( 'NONE', #27432, #29824, #22450, .T. ) ;
#11953 = CARTESIAN_POINT ( 'NONE',  ( 5.999999999999998224, 0.000000000000000000, 5.000000000000000000 ) ) ;
#11954 = CARTESIAN_POINT ( 'NONE',  ( -47.00000337463111322, 77.94228634059959404, 12.50000000000000000 ) ) ;
#11955 = CARTESIAN_POINT ( 'NONE',  ( 0.000000000000000000, 0.000000000000000000, 27.50000000000000000 ) ) ;
#11956 = CIRCLE ( 'NONE', #26932, 30.00000000000000000 ) ;
#11957 = DIRECTION ( 'NONE',  ( 1.000000000000000000, 0.000000000000000000, 0.000000000000000000 ) ) ;
#11958 = ORIENTED_EDGE ( 'NONE', *, *, #16444, .T. ) ;
#11959 = ORIENTED_EDGE ( 'NONE', *, *, #6342, .F. ) ;
#11960 = CARTESIAN_POINT ( 'NONE',  ( -25.00000337463121980, -77.94228634059963667, -9.999999999999998224 ) ) ;
#11961 = AXIS2_PLACEMENT_3D ( 'NONE', #1814, #13241, #36119 ) ;
#11962 = CYLINDRICAL_SURFACE ( 'NONE', #790, 1.999999999999998224 ) ;
#11963 = DIRECTION ( 'NONE',  ( -1.000000000000000000, 0.000000000000000000, 0.000000000000000000 ) ) ;
#11964 = VERTEX_POINT ( 'NONE', #19654 ) ;
#11965 = FACE_OUTER_BOUND ( 'NONE', #13897, .T. ) ;
#11966 = VERTEX_POINT ( 'NONE', #14005 ) ;
#11967 = VERTEX_POINT ( 'NONE', #14394 ) ;
#11968 = CARTESIAN_POINT ( 'NONE',  ( -20.00000337463122690, 86.60254037844397601, -9.999999999999998224 ) ) ;
#11969 = ORIENTED_EDGE ( 'NONE', *, *, #22037, .T. ) ;
#11970 = FACE_BOUND ( 'NONE', #4352, .T. ) ;
#11971 = DIRECTION ( 'NONE',  ( 0.000000000000000000, 0.000000000000000000, 1.000000000000000000 ) ) ;
#11972 = DIRECTION ( 'NONE',  ( -1.000000000000000000, -0.000000000000000000, -0.000000000000000000 ) ) ;
#11973 = AXIS2_PLACEMENT_3D ( 'NONE', #27957, #2282, #13717 ) ;
#11974 = ORIENTED_EDGE ( 'NONE', *, *, #9782, .T. ) ;
#11975 = EDGE_LOOP ( 'NONE', ( #30278, #30445, #637, #1852 ) ) ;
#11976 = AXIS2_PLACEMENT_3D ( 'NONE', #21915, #4686, #33362 ) ;
#11977 = ORIENTED_EDGE ( 'NONE', *, *, #28294, .F. ) ;
#11978 = ORIENTED_EDGE ( 'NONE', *, *, #8345, .T. ) ;
#11979 = ORIENTED_EDGE ( 'NONE', *, *, #22255, .F. ) ;
#11980 = DIRECTION ( 'NONE',  ( 1.000000000000000000, 0.000000000000000000, 0.000000000000000000 ) ) ;
#11981 = SURFACE_STYLE_FILL_AREA ( #26247 ) ;
#11982 = EDGE_LOOP ( 'NONE', ( #23986, #10385, #32227, #34775 ) ) ;
#11983 = DIRECTION ( 'NONE',  ( -1.000000000000000000, 0.000000000000000000, 0.000000000000000000 ) ) ;
#11984 = CARTESIAN_POINT ( 'NONE',  ( 107.1784174493373172, 49.76392998123883160, 32.50000000000000000 ) ) ;
#11985 = FACE_OUTER_BOUND ( 'NONE', #22575, .T. ) ;
#11986 = ORIENTED_EDGE ( 'NONE', *, *, #18735, .F. ) ;
#11987 = DIRECTION ( 'NONE',  ( 0.000000000000000000, 0.000000000000000000, -1.000000000000000000 ) ) ;
#11988 = DIRECTION ( 'NONE',  ( -1.000000000000000000, 0.000000000000000000, 0.000000000000000000 ) ) ;
#11989 = EDGE_CURVE ( 'NONE', #9816, #2403, #7727, .T. ) ;
#11990 = CARTESIAN_POINT ( 'NONE',  ( 29.99999662536857770, -69.28203230275519786, 17.49999999999999645 ) ) ;
#11991 = ORIENTED_EDGE ( 'NONE', *, *, #9396, .T. ) ;
#11992 = CYLINDRICAL_SURFACE ( 'NONE', #3483, 33.00000000000001421 ) ;
#11993 = LINE ( 'NONE', #23450, #20182 ) ;
#11994 = ORIENTED_EDGE ( 'NONE', *, *, #23714, .F. ) ;
#11995 = EDGE_LOOP ( 'NONE', ( #6765, #16265, #2087, #6650, #12994, #11774, #33230, #6684, #1699, #31557, #8619, #3995, #7644, #34834, #22086, #14413 ) ) ;
#11996 = DIRECTION ( 'NONE',  ( 0.000000000000000000, 0.000000000000000000, 1.000000000000000000 ) ) ;
#11997 = DIRECTION ( 'NONE',  ( 0.000000000000000000, 0.000000000000000000, 1.000000000000000000 ) ) ;
#11998 = CARTESIAN_POINT ( 'NONE',  ( -59.13646009116099833, 70.47608876694653190, 12.49999999999999822 ) ) ;
#11999 = CARTESIAN_POINT ( 'NONE',  ( 11.99999662536862566, 86.60254037844397601, -9.999999999999998224 ) ) ;
#12000 = ORIENTED_EDGE ( 'NONE', *, *, #28654, .F. ) ;
#12001 = CARTESIAN_POINT ( 'NONE',  ( -2.778182860042079927, 69.13212189986968781, 12.49999999999999645 ) ) ;
#12002 = CARTESIAN_POINT ( 'NONE',  ( 17.99999662536861678, -69.28203230275519786, 17.49999999999999645 ) ) ;
#12003 = CARTESIAN_POINT ( 'NONE',  ( 5.000000000000000000, -0.4878135028931873673, -6.000000000000001776 ) ) ;
#12004 = VERTEX_POINT ( 'NONE', #17011 ) ;
#12005 = DIRECTION ( 'NONE',  ( 0.000000000000000000, 0.000000000000000000, 1.000000000000000000 ) ) ;
#12006 = VERTEX_POINT ( 'NONE', #11556 ) ;
#12007 = ADVANCED_FACE ( 'NONE', ( #23007 ), #5578, .T. ) ;
#12008 = EDGE_CURVE ( 'NONE', #9986, #18803, #18519, .T. ) ;
#12009 = CARTESIAN_POINT ( 'NONE',  ( 93.36492675454790913, 17.14523346298246409, -49.86561046011506448 ) ) ;
#12010 = DIRECTION ( 'NONE',  ( 0.000000000000000000, 0.000000000000000000, 1.000000000000000000 ) ) ;
#12011 = CARTESIAN_POINT ( 'NONE',  ( -4.242640687119282106, 4.242640687119296317, 27.50000000000000000 ) ) ;
#12012 = EDGE_LOOP ( 'NONE', ( #2149, #26729 ) ) ;
#12013 = ORIENTED_EDGE ( 'NONE', *, *, #10564, .F. ) ;
#12014 = DIRECTION ( 'NONE',  ( 0.000000000000000000, 0.000000000000000000, 1.000000000000000000 ) ) ;
#12015 = CYLINDRICAL_SURFACE ( 'NONE', #26813, 2.000000000000001776 ) ;
#12016 = CYLINDRICAL_SURFACE ( 'NONE', #36471, 2.000000000000001776 ) ;
#12017 = ADVANCED_FACE ( 'NONE', ( #31257 ), #34274, .T. ) ;
#12018 = ORIENTED_EDGE ( 'NONE', *, *, #7145, .T. ) ;
#12019 = CARTESIAN_POINT ( 'NONE',  ( 6.999996625368645198, 77.94228634059957983, -9.999999999999998224 ) ) ;
#12020 = CIRCLE ( 'NONE', #13838, 27.00000000000001421 ) ;
#12021 = FACE_BOUND ( 'NONE', #9439, .T. ) ;
#12022 = DIRECTION ( 'NONE',  ( 1.000000000000000000, 0.000000000000000000, 0.000000000000000000 ) ) ;
#12023 = CARTESIAN_POINT ( 'NONE',  ( 42.97377950131529190, 96.90768712682505281, 18.49999999999999645 ) ) ;
#12024 = CARTESIAN_POINT ( 'NONE',  ( 24.99999662536857059, 77.94228634059957983, -5.000000000000000000 ) ) ;
#12025 = ORIENTED_EDGE ( 'NONE', *, *, #18820, .T. ) ;
#12026 = PLANE ( 'NONE',  #36274 ) ;
#12027 = EDGE_CURVE ( 'NONE', #16830, #10807, #14203, .T. ) ;
#12028 = CARTESIAN_POINT ( 'NONE',  ( 0.3000000000000016542, 0.000000000000000000, 0.000000000000000000 ) ) ;
#12029 = ORIENTED_EDGE ( 'NONE', *, *, #23290, .F. ) ;
#12030 = DIRECTION ( 'NONE',  ( 0.000000000000000000, 0.000000000000000000, 1.000000000000000000 ) ) ;
#12031 = DIRECTION ( 'NONE',  ( 1.000000000000000000, 0.000000000000000000, 0.000000000000000000 ) ) ;
#12032 = DIRECTION ( 'NONE',  ( 0.000000000000000000, 0.000000000000000000, 1.000000000000000000 ) ) ;
#12033 = VERTEX_POINT ( 'NONE', #3136 ) ;
#12034 = ORIENTED_EDGE ( 'NONE', *, *, #24255, .F. ) ;
#12035 = VERTEX_POINT ( 'NONE', #8951 ) ;
#12036 = LINE ( 'NONE', #20319, #13321 ) ;
#12037 = CARTESIAN_POINT ( 'NONE',  ( -63.00000337463104927, -43.30127018922202353, 12.50000000000000000 ) ) ;
#12038 = ORIENTED_EDGE ( 'NONE', *, *, #6612, .F. ) ;
#12039 = AXIS2_PLACEMENT_3D ( 'NONE', #6493, #11038, #17929 ) ;
#12040 = VERTEX_POINT ( 'NONE', #31798 ) ;
#12041 = CARTESIAN_POINT ( 'NONE',  ( 21.99999662536859191, 69.28203230275516944, 12.50000000000000000 ) ) ;
#12042 = ORIENTED_EDGE ( 'NONE', *, *, #13792, .T. ) ;
#12043 = ADVANCED_FACE ( 'NONE', ( #25660 ), #20201, .T. ) ;
#12044 = CARTESIAN_POINT ( 'NONE',  ( -60.00000337463108480, -51.96152422706641971, -9.999999999999998224 ) ) ;
#12045 = EDGE_LOOP ( 'NONE', ( #28100, #33624, #25149, #32296 ) ) ;
#12046 = DIRECTION ( 'NONE',  ( -1.000000000000000000, 0.000000000000000000, 0.000000000000000000 ) ) ;
#12047 = VERTEX_POINT ( 'NONE', #5966 ) ;
#12048 = EDGE_CURVE ( 'NONE', #24238, #7448, #4169, .T. ) ;
#12049 = ORIENTED_EDGE ( 'NONE', *, *, #1639, .T. ) ;
#12050 = DIRECTION ( 'NONE',  ( 0.000000000000000000, 0.000000000000000000, -1.000000000000000000 ) ) ;
#12051 = LINE ( 'NONE', #9639, #29778 ) ;
#12052 = DIRECTION ( 'NONE',  ( 0.000000000000000000, 0.000000000000000000, 1.000000000000000000 ) ) ;
#12053 = EDGE_CURVE ( 'NONE', #7932, #20086, #1785, .T. ) ;
#12054 = ORIENTED_EDGE ( 'NONE', *, *, #30685, .F. ) ;
#12055 = CARTESIAN_POINT ( 'NONE',  ( -108.3061974404896262, 19.22934205795090534, 27.50000000000000000 ) ) ;
#12056 = CARTESIAN_POINT ( 'NONE',  ( 46.99999662536851019, -60.62177826491080168, 17.49999999999999645 ) ) ;
#12057 = DIRECTION ( 'NONE',  ( 0.000000000000000000, 0.000000000000000000, 1.000000000000000000 ) ) ;
#12058 = EDGE_CURVE ( 'NONE', #7909, #8784, #14563, .T. ) ;
#12059 = EDGE_LOOP ( 'NONE', ( #19361, #12888, #15259 ) ) ;
#12060 = CARTESIAN_POINT ( 'NONE',  ( -10.00000337463125000, -86.60254037844400443, -5.000000000000000000 ) ) ;
#12061 = DIRECTION ( 'NONE',  ( -1.000000000000000000, 0.000000000000000000, -0.000000000000000000 ) ) ;
#12062 = VECTOR ( 'NONE', #17696, 1000.000000000000000 ) ;
#12063 = ORIENTED_EDGE ( 'NONE', *, *, #33017, .T. ) ;
#12064 = CARTESIAN_POINT ( 'NONE',  ( 98.28784258492957804, -106.7731239591692116, 32.55002500000000509 ) ) ;
#12065 = DIRECTION ( 'NONE',  ( 0.000000000000000000, 0.000000000000000000, 1.000000000000000000 ) ) ;
#12066 = DIRECTION ( 'NONE',  ( 1.000000000000000000, 0.000000000000000000, 0.000000000000000000 ) ) ;
#12067 = LINE ( 'NONE', #23528, #21862 ) ;
#12068 = DIRECTION ( 'NONE',  ( -0.000000000000000000, -0.000000000000000000, 1.000000000000000000 ) ) ;
#12069 = CARTESIAN_POINT ( 'NONE',  ( 15.97563234535730814, -90.60231327712320137, -4.999999999999997335 ) ) ;
#12070 = ORIENTED_EDGE ( 'NONE', *, *, #16308, .T. ) ;
#12071 = DIRECTION ( 'NONE',  ( 0.000000000000000000, -0.000000000000000000, -1.000000000000000000 ) ) ;
#12072 = DIRECTION ( 'NONE',  ( -0.000000000000000000, -0.000000000000000000, 1.000000000000000000 ) ) ;
#12073 = CARTESIAN_POINT ( 'NONE',  ( 4.279621169095998212, -62.97617850287780072, -49.86561046011506448 ) ) ;
#12074 = VERTEX_POINT ( 'NONE', #28982 ) ;
#12075 = EDGE_CURVE ( 'NONE', #4901, #33, #20010, .T. ) ;
#12076 = ORIENTED_EDGE ( 'NONE', *, *, #16488, .T. ) ;
#12077 = ORIENTED_EDGE ( 'NONE', *, *, #26802, .F. ) ;
#12078 = DIRECTION ( 'NONE',  ( 0.7071067811865389130, -0.7071067811865561215, 0.000000000000000000 ) ) ;
#12079 = CARTESIAN_POINT ( 'NONE',  ( 52.99999662536846046, -43.30127018922200222, 17.49999999999999645 ) ) ;
#12080 = CARTESIAN_POINT ( 'NONE',  ( 49.99999662536846756, 69.28203230275516944, -5.000000000000000000 ) ) ;
#12081 = EDGE_CURVE ( 'NONE', #29077, #12832, #20923, .T. ) ;
#12082 = LINE ( 'NONE', #23543, #6073 ) ;
#12083 = VECTOR ( 'NONE', #9214, 1000.000000000000000 ) ;
#12084 = CARTESIAN_POINT ( 'NONE',  ( 36.97203788309026606, -58.48108235278833433, -49.86561046011506448 ) ) ;
#12085 = EDGE_LOOP ( 'NONE', ( #15458, #34363 ) ) ;
#12086 = EDGE_CURVE ( 'NONE', #9029, #33241, #28636, .T. ) ;
#12087 = FACE_OUTER_BOUND ( 'NONE', #12499, .T. ) ;
#12088 = ORIENTED_EDGE ( 'NONE', *, *, #5610, .T. ) ;
#12089 = FACE_BOUND ( 'NONE', #30586, .T. ) ;
#12090 = DIRECTION ( 'NONE',  ( -0.000000000000000000, -0.000000000000000000, 1.000000000000000000 ) ) ;
#12091 = FACE_BOUND ( 'NONE', #32015, .T. ) ;
#12092 = ORIENTED_EDGE ( 'NONE', *, *, #23902, .F. ) ;
#12093 = CARTESIAN_POINT ( 'NONE',  ( 69.99999662536838230, -34.64101615137759183, 12.50000000000000000 ) ) ;
#12094 = APPLICATION_PROTOCOL_DEFINITION ( 'draft international standard', 'automotive_design', 1998, #13462 ) ;
#12095 = DIRECTION ( 'NONE',  ( 0.000000000000000000, 0.000000000000000000, 1.000000000000000000 ) ) ;
#12096 = EDGE_CURVE ( 'NONE', #19856, #31753, #20546, .T. ) ;
#12097 = DIRECTION ( 'NONE',  ( 1.000000000000000000, 0.000000000000000000, 0.000000000000000000 ) ) ;
#12098 = CARTESIAN_POINT ( 'NONE',  ( 51.99999662536847467, 69.28203230275516944, -9.999999999999998224 ) ) ;
#12099 = VERTEX_POINT ( 'NONE', #11936 ) ;
#12100 = DIRECTION ( 'NONE',  ( 1.000000000000000000, 0.000000000000000000, 0.000000000000000000 ) ) ;
#12101 = CARTESIAN_POINT ( 'NONE',  ( 86.99999662536832545, 8.660254037844394404, -9.999999999999998224 ) ) ;
#12102 = DIRECTION ( 'NONE',  ( 0.000000000000000000, 0.000000000000000000, -1.000000000000000000 ) ) ;
#12103 = VERTEX_POINT ( 'NONE', #23395 ) ;
#12104 = ORIENTED_EDGE ( 'NONE', *, *, #12463, .T. ) ;
#12105 = VECTOR ( 'NONE', #10520, 1000.000000000000000 ) ;
#12106 = ORIENTED_EDGE ( 'NONE', *, *, #19655, .T. ) ;
#12107 = DIRECTION ( 'NONE',  ( -1.000000000000000000, 0.000000000000000000, 0.000000000000000000 ) ) ;
#12108 = CARTESIAN_POINT ( 'NONE',  ( 60.93295298011005201, 19.13981058454729123, 12.49999999999999822 ) ) ;
#12109 = EDGE_CURVE ( 'NONE', #16919, #29590, #16754, .T. ) ;
#12110 = ORIENTED_EDGE ( 'NONE', *, *, #11615, .F. ) ;
#12111 = DIRECTION ( 'NONE',  ( 0.000000000000000000, 0.000000000000000000, 1.000000000000000000 ) ) ;
#12112 = CARTESIAN_POINT ( 'NONE',  ( 29.99999662536856349, 69.28203230275518365, -9.999999999999998224 ) ) ;
#12113 = EDGE_CURVE ( 'NONE', #22424, #9206, #6309, .T. ) ;
#12114 = DIRECTION ( 'NONE',  ( -1.000000000000000000, 0.000000000000000000, 0.000000000000000000 ) ) ;
#12115 = ORIENTED_EDGE ( 'NONE', *, *, #14435, .F. ) ;
#12116 = EDGE_CURVE ( 'NONE', #26437, #17529, #3520, .T. ) ;
#12117 = VERTEX_POINT ( 'NONE', #15121 ) ;
#12118 = VECTOR ( 'NONE', #23831, 1000.000000000000000 ) ;
#12119 = CARTESIAN_POINT ( 'NONE',  ( -2.500000000000000000, 3.061616997868383141E-16, -0.3501037691048548561 ) ) ;
#12120 = CYLINDRICAL_SURFACE ( 'NONE', #5590, 2.000000000000001776 ) ;
#12121 = CYLINDRICAL_SURFACE ( 'NONE', #22144, 2.000000000000001776 ) ;
#12122 = ADVANCED_FACE ( 'NONE', ( #29934 ), #18512, .F. ) ;
#12123 = ORIENTED_EDGE ( 'NONE', *, *, #18122, .T. ) ;
#12124 = ADVANCED_FACE ( 'NONE', ( #10068 ), #32741, .F. ) ;
#12125 = FACE_BOUND ( 'NONE', #30740, .T. ) ;
#12126 = ORIENTED_EDGE ( 'NONE', *, *, #12138, .F. ) ;
#12127 = CIRCLE ( 'NONE', #11535, 2.000000000000001776 ) ;
#12128 = EDGE_LOOP ( 'NONE', ( #7340, #36291 ) ) ;
#12129 = FACE_OUTER_BOUND ( 'NONE', #5818, .T. ) ;
#12130 = ORIENTED_EDGE ( 'NONE', *, *, #33840, .F. ) ;
#12131 = EDGE_CURVE ( 'NONE', #5193, #20137, #30505, .T. ) ;
#12132 = EDGE_CURVE ( 'NONE', #14960, #4180, #2965, .T. ) ;
#12133 = DIRECTION ( 'NONE',  ( 1.000000000000000000, 0.000000000000000000, 0.000000000000000000 ) ) ;
#12134 = EDGE_CURVE ( 'NONE', #25177, #5895, #24545, .T. ) ;
#12135 = CYLINDRICAL_SURFACE ( 'NONE', #10729, 2.000000000000001776 ) ;
#12136 = CARTESIAN_POINT ( 'NONE',  ( -50.00000337463112032, -51.96152422706641971, -9.999999999999998224 ) ) ;
#12137 = ORIENTED_EDGE ( 'NONE', *, *, #4776, .T. ) ;
#12138 = EDGE_CURVE ( 'NONE', #34610, #25842, #26748, .T. ) ;
#12139 = ORIENTED_EDGE ( 'NONE', *, *, #9990, .T. ) ;
#12140 = AXIS2_PLACEMENT_3D ( 'NONE', #17330, #5520, #19944 ) ;
#12141 = ORIENTED_EDGE ( 'NONE', *, *, #15567, .F. ) ;
#12142 = ORIENTED_EDGE ( 'NONE', *, *, #29965, .F. ) ;
#12143 = CIRCLE ( 'NONE', #33129, 150.0000000000000284 ) ;
#12144 = EDGE_LOOP ( 'NONE', ( #4021, #30065, #2578, #2862, #33670 ) ) ;
#12145 = CARTESIAN_POINT ( 'NONE',  ( -55.00000337463109901, -60.62177826491083010, 12.50000000000000000 ) ) ;
#12146 = CARTESIAN_POINT ( 'NONE',  ( 48.49678893472093932, 67.96280274017779277, -5.000000000000000000 ) ) ;
#12147 = VERTEX_POINT ( 'NONE', #4068 ) ;
#12148 = DIRECTION ( 'NONE',  ( 0.000000000000000000, 0.000000000000000000, 1.000000000000000000 ) ) ;
#12149 = CARTESIAN_POINT ( 'NONE',  ( 0.000000000000000000, 95.00000000000001421, 32.50000000000000000 ) ) ;
#12150 = CARTESIAN_POINT ( 'NONE',  ( -33.00000337463117006, -77.94228634059963667, -5.000000000000000000 ) ) ;
#12151 = ORIENTED_EDGE ( 'NONE', *, *, #28504, .T. ) ;
#12152 = DIRECTION ( 'NONE',  ( 0.000000000000000000, 0.000000000000000000, 1.000000000000000000 ) ) ;
#12153 = VECTOR ( 'NONE', #13404, 1000.000000000000000 ) ;
#12154 = LINE ( 'NONE', #23618, #21589 ) ;
#12155 = CIRCLE ( 'NONE', #21766, 27.00000000000001421 ) ;
#12156 = CARTESIAN_POINT ( 'NONE',  ( -47.04203867989546950, 43.19957991610416315, 12.49999999999999822 ) ) ;
#12157 = ORIENTED_EDGE ( 'NONE', *, *, #11949, .F. ) ;
#12158 = CARTESIAN_POINT ( 'NONE',  ( 51.99999662536848888, -51.96152422706640550, -9.999999999999998224 ) ) ;
#12159 = FACE_OUTER_BOUND ( 'NONE', #4821, .T. ) ;
#12160 = AXIS2_PLACEMENT_3D ( 'NONE', #19813, #28608, #17532 ) ;
#12161 = ORIENTED_EDGE ( 'NONE', *, *, #29511, .F. ) ;
#12162 = EDGE_LOOP ( 'NONE', ( #152, #27749, #30528, #6331 ) ) ;
#12163 = DIRECTION ( 'NONE',  ( 0.000000000000000000, 0.000000000000000000, 1.000000000000000000 ) ) ;
#12164 = DIRECTION ( 'NONE',  ( 0.000000000000000000, 0.000000000000000000, 1.000000000000000000 ) ) ;
#12165 = CARTESIAN_POINT ( 'NONE',  ( 14.99999662536859901, 77.94228634059957983, -9.999999999999998224 ) ) ;
#12166 = CARTESIAN_POINT ( 'NONE',  ( 79.99999662536832545, -17.32050807568879591, -9.999999999999998224 ) ) ;
#12167 = VERTEX_POINT ( 'NONE', #15305 ) ;
#12168 = AXIS2_PLACEMENT_3D ( 'NONE', #24626, #1738, #22344 ) ;
#12169 = DIRECTION ( 'NONE',  ( 0.000000000000000000, 0.000000000000000000, 1.000000000000000000 ) ) ;
#12170 = CARTESIAN_POINT ( 'NONE',  ( 4.279621169095998212, -62.97617850287780072, 12.49999999999999822 ) ) ;
#12171 = CIRCLE ( 'NONE', #33758, 3.866666666667000651 ) ;
#12172 = EDGE_LOOP ( 'NONE', ( #3493, #35782, #32609, #10945 ) ) ;
#12173 = CARTESIAN_POINT ( 'NONE',  ( -75.00000337463100664, -43.30127018922202353, -5.000000000000000000 ) ) ;
#12174 = ORIENTED_EDGE ( 'NONE', *, *, #8558, .F. ) ;
#12175 = DIRECTION ( 'NONE',  ( 1.000000000000000000, 0.000000000000000000, 0.000000000000000000 ) ) ;
#12176 = EDGE_CURVE ( 'NONE', #18535, #35393, #5964, .T. ) ;
#12177 = DIRECTION ( 'NONE',  ( 0.000000000000000000, 0.000000000000000000, 1.000000000000000000 ) ) ;
#12178 = EDGE_CURVE ( 'NONE', #11174, #21285, #20324, .T. ) ;
#12179 = LINE ( 'NONE', #23469, #6469 ) ;
#12180 = ADVANCED_FACE ( 'NONE', ( #4259 ), #30107, .F. ) ;
#12181 = ORIENTED_EDGE ( 'NONE', *, *, #23436, .T. ) ;
#12182 = ORIENTED_EDGE ( 'NONE', *, *, #31104, .F. ) ;
#12183 = CARTESIAN_POINT ( 'NONE',  ( 57.99999662536842493, -51.96152422706639840, -5.000000000000000000 ) ) ;
#12184 = CARTESIAN_POINT ( 'NONE',  ( -52.00000337463110611, -69.28203230275519786, -9.999999999999998224 ) ) ;
#12185 = CARTESIAN_POINT ( 'NONE',  ( 39.99999662536853151, 69.28203230275518365, 12.50000000000000000 ) ) ;
#12186 = ORIENTED_EDGE ( 'NONE', *, *, #5766, .T. ) ;
#12187 = DIRECTION ( 'NONE',  ( 1.000000000000000000, 0.000000000000000000, 0.000000000000000000 ) ) ;
#12188 = FACE_BOUND ( 'NONE', #8878, .T. ) ;
#12189 = CARTESIAN_POINT ( 'NONE',  ( 0.000000000000000000, 0.000000000000000000, 32.50000000000000000 ) ) ;
#12190 = DIRECTION ( 'NONE',  ( -1.000000000000000000, 0.000000000000000000, 0.000000000000000000 ) ) ;
#12191 = FACE_OUTER_BOUND ( 'NONE', #16652, .T. ) ;
#12192 = EDGE_LOOP ( 'NONE', ( #26699, #18227 ) ) ;
#12193 = FACE_OUTER_BOUND ( 'NONE', #7670, .T. ) ;
#12194 = VECTOR ( 'NONE', #35384, 1000.000000000000000 ) ;
#12195 = B_SPLINE_CURVE_WITH_KNOTS ( 'NONE', 3,
 ( #36411, #30399, #2276, #8081, #13510 ),
 .UNSPECIFIED., .F., .F.,
 ( 4, 1, 4 ),
 ( 5.023827903067772009E-20, 0.002886751345948134623, 0.005773502691896269245 ),
 .UNSPECIFIED. ) ;
#12196 = CYLINDRICAL_SURFACE ( 'NONE', #16419, 2.000000000000001776 ) ;
#12197 = ORIENTED_EDGE ( 'NONE', *, *, #25507, .T. ) ;
#12198 = DIRECTION ( 'NONE',  ( -1.000000000000000000, 0.000000000000000000, 0.000000000000000000 ) ) ;
#12199 = DIRECTION ( 'NONE',  ( 0.000000000000000000, 0.000000000000000000, -1.000000000000000000 ) ) ;
#12200 = DIRECTION ( 'NONE',  ( -0.000000000000000000, -0.000000000000000000, 1.000000000000000000 ) ) ;
#12201 = EDGE_CURVE ( 'NONE', #18462, #3561, #22132, .T. ) ;
#12202 = AXIS2_PLACEMENT_3D ( 'NONE', #33759, #31471, #16502 ) ;
#12203 = ORIENTED_EDGE ( 'NONE', *, *, #21038, .F. ) ;
#12204 = ORIENTED_EDGE ( 'NONE', *, *, #22353, .F. ) ;
#12205 = ORIENTED_EDGE ( 'NONE', *, *, #22229, .T. ) ;
#12206 = CIRCLE ( 'NONE', #12811, 2.000000000000001776 ) ;
#12207 = DIRECTION ( 'NONE',  ( 1.000000000000000000, 0.000000000000000000, 0.000000000000000000 ) ) ;
#12208 = DIRECTION ( 'NONE',  ( -0.000000000000000000, -0.000000000000000000, 1.000000000000000000 ) ) ;
#12209 = DIRECTION ( 'NONE',  ( 1.000000000000000000, 0.000000000000000000, 0.000000000000000000 ) ) ;
#12210 = ORIENTED_EDGE ( 'NONE', *, *, #4799, .T. ) ;
#12211 = ORIENTED_EDGE ( 'NONE', *, *, #3160, .T. ) ;
#12212 = EDGE_LOOP ( 'NONE', ( #33674, #26585, #7879, #3058 ) ) ;
#12213 = CYLINDRICAL_SURFACE ( 'NONE', #23089, 27.00000000000001421 ) ;
#12214 = ORIENTED_EDGE ( 'NONE', *, *, #1396, .F. ) ;
#12215 = CARTESIAN_POINT ( 'NONE',  ( -30.00000337463119848, -69.28203230275522628, 17.49999999999999645 ) ) ;
#12216 = ORIENTED_EDGE ( 'NONE', *, *, #2525, .F. ) ;
#12217 = DIRECTION ( 'NONE',  ( 1.000000000000000000, 0.000000000000000000, 0.000000000000000000 ) ) ;
#12218 = VERTEX_POINT ( 'NONE', #27108 ) ;
#12219 = EDGE_LOOP ( 'NONE', ( #3465, #17884, #2501, #36816, #27778, #204 ) ) ;
#12220 = CIRCLE ( 'NONE', #33836, 33.00000000000001421 ) ;
#12221 = DIRECTION ( 'NONE',  ( -1.000000000000000000, 0.000000000000000000, 0.000000000000000000 ) ) ;
#12222 = CARTESIAN_POINT ( 'NONE',  ( 42.99999662536850309, 77.94228634059959404, 12.50000000000000000 ) ) ;
#12223 = CARTESIAN_POINT ( 'NONE',  ( -53.00000337463106348, 60.62177826491078747, 17.49999999999999645 ) ) ;
#12224 = EDGE_CURVE ( 'NONE', #18123, #10426, #8949, .T. ) ;
#12225 = VERTEX_POINT ( 'NONE', #6690 ) ;
#12226 = VERTEX_POINT ( 'NONE', #35951 ) ;
#12227 = CARTESIAN_POINT ( 'NONE',  ( -35.00000337463117717, -77.94228634059963667, -9.999999999999998224 ) ) ;
#12228 = CARTESIAN_POINT ( 'NONE',  ( -5.000000000000000000, 25.00000000000000000, -15.00000000000000000 ) ) ;
#12229 = CIRCLE ( 'NONE', #27807, 2.000000000000001776 ) ;
#12230 = CYLINDRICAL_SURFACE ( 'NONE', #36053, 2.000000000000001776 ) ;
#12231 = AXIS2_PLACEMENT_3D ( 'NONE', #27141, #26587, #29772 ) ;
#12232 = DIRECTION ( 'NONE',  ( 0.000000000000000000, 0.000000000000000000, -1.000000000000000000 ) ) ;
#12233 = AXIS2_PLACEMENT_3D ( 'NONE', #11722, #5746, #110 ) ;
#12234 = ORIENTED_EDGE ( 'NONE', *, *, #34988, .F. ) ;
#12235 = AXIS2_PLACEMENT_3D ( 'NONE', #2717, #23152, #28942 ) ;
#12236 = CARTESIAN_POINT ( 'NONE',  ( 9.999996625368655856, -86.60254037844400443, -9.999999999999998224 ) ) ;
#12237 = DIRECTION ( 'NONE',  ( -0.000000000000000000, -0.000000000000000000, -1.000000000000000000 ) ) ;
#12238 = EDGE_LOOP ( 'NONE', ( #32588, #30639, #32742, #23995 ) ) ;
#12239 = DIRECTION ( 'NONE',  ( 1.000000000000000000, 0.000000000000000000, 0.000000000000000000 ) ) ;
#12240 = CARTESIAN_POINT ( 'NONE',  ( -18.00000337463124467, 69.28203230275516944, -9.999999999999998224 ) ) ;
#12241 = FACE_OUTER_BOUND ( 'NONE', #28200, .T. ) ;
#12242 = DIRECTION ( 'NONE',  ( 0.000000000000000000, 0.000000000000000000, 1.000000000000000000 ) ) ;
#12243 = DIRECTION ( 'NONE',  ( -1.000000000000000000, 0.000000000000000000, 0.000000000000000000 ) ) ;
#12244 = AXIS2_PLACEMENT_3D ( 'NONE', #18001, #23445, #28698 ) ;
#12245 = EDGE_CURVE ( 'NONE', #11213, #8789, #14951, .T. ) ;
#12246 = CARTESIAN_POINT ( 'NONE',  ( 79.99999662536833966, 17.32050807568879236, -9.999999999999998224 ) ) ;
#12247 = ORIENTED_EDGE ( 'NONE', *, *, #4357, .F. ) ;
#12249 = CIRCLE ( 'NONE', #19481, 3.050000000000000711 ) ;
#12248 = DIRECTION ( 'NONE',  ( 0.000000000000000000, 0.000000000000000000, 1.000000000000000000 ) ) ;
#12250 = CARTESIAN_POINT ( 'NONE',  ( 0.000000000000000000, 0.000000000000000000, 0.000000000000000000 ) ) ;
#12251 = CYLINDRICAL_SURFACE ( 'NONE', #6802, 2.000000000000001776 ) ;
#12252 = EDGE_CURVE ( 'NONE', #10165, #7561, #16165, .T. ) ;
#12253 = VERTEX_POINT ( 'NONE', #12850 ) ;
#12254 = ORIENTED_EDGE ( 'NONE', *, *, #13188, .F. ) ;
#12255 = VERTEX_POINT ( 'NONE', #6864 ) ;
#12256 = DIRECTION ( 'NONE',  ( 0.000000000000000000, 0.000000000000000000, 1.000000000000000000 ) ) ;
#12257 = DIRECTION ( 'NONE',  ( 1.000000000000000000, 0.000000000000000000, 0.000000000000000000 ) ) ;
#12258 = EDGE_CURVE ( 'NONE', #17955, #10852, #18306, .T. ) ;
#12259 = CARTESIAN_POINT ( 'NONE',  ( 12.99999662536859901, 77.94228634059957983, -9.999999999999998224 ) ) ;
#12260 = AXIS2_PLACEMENT_3D ( 'NONE', #5767, #6508, #17208 ) ;
#12261 = AXIS2_PLACEMENT_3D ( 'NONE', #4669, #19111, #35350 ) ;
#12262 = DIRECTION ( 'NONE',  ( 0.000000000000000000, 0.000000000000000000, -1.000000000000000000 ) ) ;
#12263 = EDGE_CURVE ( 'NONE', #22983, #21984, #6571, .T. ) ;
#12264 = LINE ( 'NONE', #3846, #3337 ) ;
#12265 = VERTEX_POINT ( 'NONE', #12670 ) ;
#12266 = LINE ( 'NONE', #9677, #4184 ) ;
#12267 = ORIENTED_EDGE ( 'NONE', *, *, #9579, .F. ) ;
#12268 = FACE_BOUND ( 'NONE', #14098, .T. ) ;
#12269 = DIRECTION ( 'NONE',  ( 0.000000000000000000, 0.000000000000000000, 1.000000000000000000 ) ) ;
#12270 = AXIS2_PLACEMENT_3D ( 'NONE', #14349, #88, #17158 ) ;
#12271 = CARTESIAN_POINT ( 'NONE',  ( -3.000003374631308173, 77.94228634059957983, -9.999999999999998224 ) ) ;
#12272 = EDGE_CURVE ( 'NONE', #36161, #27930, #35309, .T. ) ;
#12273 = CIRCLE ( 'NONE', #29067, 5.000000000000000888 ) ;
#12274 = ORIENTED_EDGE ( 'NONE', *, *, #26122, .T. ) ;
#12275 = CARTESIAN_POINT ( 'NONE',  ( -50.00000337463110611, -69.28203230275519786, 12.50000000000000000 ) ) ;
#12276 = AXIS2_PLACEMENT_3D ( 'NONE', #22537, #27612, #13347 ) ;
#12277 = APPLICATION_PROTOCOL_DEFINITION ( 'draft international standard', 'automotive_design', 1998, #3678 ) ;
#12278 = CIRCLE ( 'NONE', #3310, 1.999999999999998224 ) ;
#12279 = VECTOR ( 'NONE', #17367, 1000.000000000000114 ) ;
#12280 = CARTESIAN_POINT ( 'NONE',  ( 64.99999662536842493, 43.30127018922200222, -5.000000000000000000 ) ) ;
#12281 = AXIS2_PLACEMENT_3D ( 'NONE', #26637, #34903, #9762 ) ;
#12282 = CARTESIAN_POINT ( 'NONE',  ( 11.99999662536861855, 69.28203230275516944, 17.49999999999999645 ) ) ;
#12283 = DIRECTION ( 'NONE',  ( 1.000000000000000000, 0.000000000000000000, 0.000000000000000000 ) ) ;
#12284 = ORIENTED_EDGE ( 'NONE', *, *, #1833, .F. ) ;
#12285 = DIRECTION ( 'NONE',  ( 1.000000000000000000, 0.000000000000000000, 0.000000000000000000 ) ) ;
#12286 = CARTESIAN_POINT ( 'NONE',  ( 69.99999662536838230, -51.96152422706639840, -5.000000000000000000 ) ) ;
#12287 = DIRECTION ( 'NONE',  ( 0.000000000000000000, 0.000000000000000000, 1.000000000000000000 ) ) ;
#12288 = CIRCLE ( 'NONE', #19495, 2.000000000000001776 ) ;
#12289 = EDGE_CURVE ( 'NONE', #12365, #24912, #33514, .T. ) ;
#12290 = CIRCLE ( 'NONE', #20682, 95.00000000000001421 ) ;
#12291 = ORIENTED_EDGE ( 'NONE', *, *, #26211, .F. ) ;
#12292 = ORIENTED_EDGE ( 'NONE', *, *, #7798, .F. ) ;
#12293 = EDGE_CURVE ( 'NONE', #22692, #460, #18547, .T. ) ;
#12294 = EDGE_LOOP ( 'NONE', ( #11302, #34900 ) ) ;
#12295 = CARTESIAN_POINT ( 'NONE',  ( -60.00000337463104216, 51.96152422706639129, 12.50000000000000000 ) ) ;
#12296 = DIRECTION ( 'NONE',  ( 1.000000000000000000, 0.000000000000000000, 0.000000000000000000 ) ) ;
#12297 = ADVANCED_FACE ( 'NONE', ( #16252 ), #16421, .F. ) ;
#12298 = DIRECTION ( 'NONE',  ( 1.000000000000000000, 0.000000000000000000, 0.000000000000000000 ) ) ;
#12299 = CARTESIAN_POINT ( 'NONE',  ( 54.99999662536844625, -60.62177826491080168, -5.000000000000000000 ) ) ;
#12300 = DIRECTION ( 'NONE',  ( -1.000000000000000000, 0.000000000000000000, 0.000000000000000000 ) ) ;
#12301 = AXIS2_PLACEMENT_3D ( 'NONE', #27028, #30203, #15781 ) ;
#12302 = EDGE_CURVE ( 'NONE', #5493, #35478, #13745, .T. ) ;
#12303 = CIRCLE ( 'NONE', #35087, 2.000000000000001776 ) ;
#12304 = VECTOR ( 'NONE', #2050, 1000.000000000000000 ) ;
#12305 = DIRECTION ( 'NONE',  ( 1.000000000000000000, 0.000000000000000000, 0.000000000000000000 ) ) ;
#12306 = AXIS2_PLACEMENT_3D ( 'NONE', #10951, #4609, #22907 ) ;
#12307 = ORIENTED_EDGE ( 'NONE', *, *, #23377, .F. ) ;
#12308 = ORIENTED_EDGE ( 'NONE', *, *, #18350, .F. ) ;
#12309 = DIRECTION ( 'NONE',  ( -1.000000000000000000, 0.000000000000000000, 0.000000000000000000 ) ) ;
#12310 = CIRCLE ( 'NONE', #24337, 2.000000000000001776 ) ;
#12311 = EDGE_CURVE ( 'NONE', #11585, #6228, #31688, .T. ) ;
#12312 = CARTESIAN_POINT ( 'NONE',  ( -50.00000337463109190, 51.96152422706637708, 17.49999999999999645 ) ) ;
#12313 = VERTEX_POINT ( 'NONE', #18869 ) ;
#12314 = CARTESIAN_POINT ( 'NONE',  ( -5.284804376168106721, -3.015249596956847356, -4.366192694417986964 ) ) ;
#12315 = VERTEX_POINT ( 'NONE', #4628 ) ;
#12316 = AXIS2_PLACEMENT_3D ( 'NONE', #19083, #10430, #31058 ) ;
#12317 = VECTOR ( 'NONE', #22094, 1000.000000000000000 ) ;
#12318 = FACE_BOUND ( 'NONE', #9466, .T. ) ;
#12319 = ORIENTED_EDGE ( 'NONE', *, *, #13517, .F. ) ;
#12320 = ORIENTED_EDGE ( 'NONE', *, *, #26400, .F. ) ;
#12321 = CARTESIAN_POINT ( 'NONE',  ( 84.99999662536831124, -8.660254037844397956, -9.999999999999998224 ) ) ;
#12322 = ORIENTED_EDGE ( 'NONE', *, *, #12344, .F. ) ;
#12323 = CIRCLE ( 'NONE', #23109, 2.000000000000000000 ) ;
#12324 = CYLINDRICAL_SURFACE ( 'NONE', #2681, 2.000000000000001776 ) ;
#12325 = EDGE_CURVE ( 'NONE', #21059, #20978, #5383, .T. ) ;
#12326 = VECTOR ( 'NONE', #29845, 1000.000000000000000 ) ;
#12327 = CARTESIAN_POINT ( 'NONE',  ( 4.592054218142288313, 3.122278952918447814, -5.689399939901071512 ) ) ;
#12328 = DIRECTION ( 'NONE',  ( 0.000000000000000000, 0.000000000000000000, -1.000000000000000000 ) ) ;
#12329 = VERTEX_POINT ( 'NONE', #19250 ) ;
#12330 = ORIENTED_EDGE ( 'NONE', *, *, #17378, .T. ) ;
#12331 = AXIS2_PLACEMENT_3D ( 'NONE', #10783, #11329, #19943 ) ;
#12332 = AXIS2_PLACEMENT_3D ( 'NONE', #19752, #30789, #25202 ) ;
#12333 = ORIENTED_EDGE ( 'NONE', *, *, #7980, .T. ) ;
#12334 = CIRCLE ( 'NONE', #21949, 27.00000000000001421 ) ;
#12335 = ADVANCED_FACE ( 'NONE', ( #22410 ), #7621, .F. ) ;
#12336 = CIRCLE ( 'NONE', #7575, 3.500000000000003109 ) ;
#12337 = ORIENTED_EDGE ( 'NONE', *, *, #4254, .F. ) ;
#12338 = AXIS2_PLACEMENT_3D ( 'NONE', #18693, #4263, #15692 ) ;
#12339 = VERTEX_POINT ( 'NONE', #22237 ) ;
#12340 = CARTESIAN_POINT ( 'NONE',  ( 69.99999662536841072, 51.96152422706640550, -9.999999999999998224 ) ) ;
#12341 = EDGE_CURVE ( 'NONE', #23885, #10643, #19143, .T. ) ;
#12342 = CYLINDRICAL_SURFACE ( 'NONE', #35, 3.000000000000002665 ) ;
#12343 = ORIENTED_EDGE ( 'NONE', *, *, #19145, .T. ) ;
#12344 = EDGE_CURVE ( 'NONE', #18489, #3043, #19070, .T. ) ;
#12345 = DIRECTION ( 'NONE',  ( 0.000000000000000000, 0.000000000000000000, 1.000000000000000000 ) ) ;
#12346 = CARTESIAN_POINT ( 'NONE',  ( 98.21838448168142577, 66.76540064347040015, 32.50000000000000711 ) ) ;
#12347 = DIRECTION ( 'NONE',  ( 1.082992363797667670E-14, 1.000000000000000000, 0.000000000000000000 ) ) ;
#12348 = ORIENTED_EDGE ( 'NONE', *, *, #31420, .F. ) ;
#12349 = CARTESIAN_POINT ( 'NONE',  ( -55.00000337463109901, -60.62177826491083010, 12.50000000000000000 ) ) ;
#12350 = AXIS2_PLACEMENT_3D ( 'NONE', #9067, #18062, #31914 ) ;
#12351 = FACE_OUTER_BOUND ( 'NONE', #5288, .T. ) ;
#12352 = CARTESIAN_POINT ( 'NONE',  ( 5.750000000000035527, 83.21147890756138565, -24.99999999999999289 ) ) ;
#12353 = VERTEX_POINT ( 'NONE', #25414 ) ;
#12354 = CARTESIAN_POINT ( 'NONE',  ( 34.99999662536855283, 60.62177826491078747, 12.50000000000000000 ) ) ;
#12355 = DIRECTION ( 'NONE',  ( 1.000000000000000000, 0.000000000000000000, 0.000000000000000000 ) ) ;
#12356 = ORIENTED_EDGE ( 'NONE', *, *, #24105, .F. ) ;
#12357 = EDGE_LOOP ( 'NONE', ( #6729, #15760 ) ) ;
#12358 = CARTESIAN_POINT ( 'NONE',  ( 95.00000000000001421, 0.000000000000000000, 27.50000000000000000 ) ) ;
#12359 = EDGE_CURVE ( 'NONE', #8015, #22987, #26324, .T. ) ;
#12360 = CIRCLE ( 'NONE', #8188, 2.000000000000000000 ) ;
#12361 = DIRECTION ( 'NONE',  ( 0.000000000000000000, 0.000000000000000000, 1.000000000000000000 ) ) ;
#12362 = DIRECTION ( 'NONE',  ( -0.000000000000000000, -0.000000000000000000, 1.000000000000000000 ) ) ;
#12363 = DIRECTION ( 'NONE',  ( 0.000000000000000000, 0.000000000000000000, 1.000000000000000000 ) ) ;
#12364 = ORIENTED_EDGE ( 'NONE', *, *, #36802, .T. ) ;
#12365 = VERTEX_POINT ( 'NONE', #5176 ) ;
#12366 = VECTOR ( 'NONE', #10240, 1000.000000000000000 ) ;
#12367 = CARTESIAN_POINT ( 'NONE',  ( -5.000000000000000888, 1.953108124182649563, -0.2699991669428306595 ) ) ;
#12368 = FACE_BOUND ( 'NONE', #23487, .T. ) ;
#12369 = CIRCLE ( 'NONE', #24396, 1.999999999999998224 ) ;
#12370 = ORIENTED_EDGE ( 'NONE', *, *, #30074, .T. ) ;
#12371 = DIRECTION ( 'NONE',  ( 0.000000000000000000, -0.000000000000000000, -1.000000000000000000 ) ) ;
#12372 = ORIENTED_EDGE ( 'NONE', *, *, #2210, .F. ) ;
#12373 = DIRECTION ( 'NONE',  ( 0.000000000000000000, 0.000000000000000000, -1.000000000000000000 ) ) ;
#12374 = CIRCLE ( 'NONE', #7616, 2.000000000000001776 ) ;
#12375 = DIRECTION ( 'NONE',  ( 0.000000000000000000, 0.000000000000000000, -1.000000000000000000 ) ) ;
#12376 = EDGE_CURVE ( 'NONE', #26527, #15313, #33544, .T. ) ;
#12377 = DIRECTION ( 'NONE',  ( 0.000000000000000000, 0.000000000000000000, 1.000000000000000000 ) ) ;
#12378 = VERTEX_POINT ( 'NONE', #30665 ) ;
#12379 = EDGE_CURVE ( 'NONE', #23662, #29469, #13966, .T. ) ;
#12380 = ORIENTED_EDGE ( 'NONE', *, *, #4639, .F. ) ;
#12381 = VECTOR ( 'NONE', #16379, 1000.000000000000000 ) ;
#12382 = CIRCLE ( 'NONE', #8818, 2.000000000000001776 ) ;
#12383 = DIRECTION ( 'NONE',  ( 0.000000000000000000, 0.000000000000000000, 1.000000000000000000 ) ) ;
#12384 = EDGE_CURVE ( 'NONE', #21315, #22186, #25749, .T. ) ;
#12385 = AXIS2_PLACEMENT_3D ( 'NONE', #11216, #7867, #19304 ) ;
#12386 = ORIENTED_EDGE ( 'NONE', *, *, #7220, .T. ) ;
#12387 = DIRECTION ( 'NONE',  ( 1.000000000000000000, 0.000000000000000000, 0.000000000000000000 ) ) ;
#12388 = DIRECTION ( 'NONE',  ( 1.000000000000000000, 0.000000000000000000, 0.000000000000000000 ) ) ;
#12389 = EDGE_CURVE ( 'NONE', #2324, #7804, #35949, .T. ) ;
#12390 = DIRECTION ( 'NONE',  ( -0.000000000000000000, -0.000000000000000000, 1.000000000000000000 ) ) ;
#12391 = DIRECTION ( 'NONE',  ( 0.000000000000000000, 0.000000000000000000, -1.000000000000000000 ) ) ;
#12392 = CARTESIAN_POINT ( 'NONE',  ( -35.00000337463116296, 60.62177826491077326, -9.999999999999998224 ) ) ;
#12393 = EDGE_CURVE ( 'NONE', #14572, #20117, #29932, .T. ) ;
#12394 = AXIS2_PLACEMENT_3D ( 'NONE', #4973, #10794, #13397 ) ;
#12395 = EDGE_LOOP ( 'NONE', ( #27862, #23503 ) ) ;
#12396 = DIRECTION ( 'NONE',  ( -0.000000000000000000, -0.000000000000000000, 1.000000000000000000 ) ) ;
#12397 = AXIS2_PLACEMENT_3D ( 'NONE', #20223, #15839, #18485 ) ;
#12398 = CIRCLE ( 'NONE', #29193, 2.000000000000001776 ) ;
#12399 = DIRECTION ( 'NONE',  ( -1.000000000000000000, 0.000000000000000000, 0.000000000000000000 ) ) ;
#12400 = ORIENTED_EDGE ( 'NONE', *, *, #21686, .F. ) ;
#12401 = CYLINDRICAL_SURFACE ( 'NONE', #19044, 2.000000000000001776 ) ;
#12402 = DIRECTION ( 'NONE',  ( 0.000000000000000000, 0.000000000000000000, -1.000000000000000000 ) ) ;
#12403 = CARTESIAN_POINT ( 'NONE',  ( 46.99999662536851019, 77.94228634059959404, 17.49999999999999645 ) ) ;
#12404 = AXIS2_PLACEMENT_3D ( 'NONE', #5726, #33857, #31395 ) ;
#12405 = EDGE_CURVE ( 'NONE', #18518, #21193, #14976, .T. ) ;
#12406 = ORIENTED_EDGE ( 'NONE', *, *, #33798, .F. ) ;
#12407 = EDGE_CURVE ( 'NONE', #6635, #36626, #17971, .T. ) ;
#12408 = VERTEX_POINT ( 'NONE', #33304 ) ;
#12409 = EDGE_CURVE ( 'NONE', #17975, #26476, #16613, .T. ) ;
#12410 = VECTOR ( 'NONE', #6243, 1000.000000000000000 ) ;
#12411 = ADVANCED_FACE ( 'NONE', ( #5723 ), #23352, .F. ) ;
#12412 = CARTESIAN_POINT ( 'NONE',  ( 6.000000000000000000, 0.000000000000000000, 0.000000000000000000 ) ) ;
#12413 = DIRECTION ( 'NONE',  ( 0.000000000000000000, 0.000000000000000000, 1.000000000000000000 ) ) ;
#12414 = DIRECTION ( 'NONE',  ( 1.000000000000000000, 0.000000000000000000, 0.000000000000000000 ) ) ;
#12415 = VERTEX_POINT ( 'NONE', #31392 ) ;
#12416 = VERTEX_POINT ( 'NONE', #14159 ) ;
#12417 = AXIS2_PLACEMENT_3D ( 'NONE', #23178, #34629, #14176 ) ;
#12418 = CIRCLE ( 'NONE', #30392, 33.00000000000001421 ) ;
#12419 = VERTEX_POINT ( 'NONE', #3473 ) ;
#12420 = AXIS2_PLACEMENT_3D ( 'NONE', #8854, #22756, #20295 ) ;
#12421 = DIRECTION ( 'NONE',  ( 0.000000000000000000, 0.000000000000000000, 1.000000000000000000 ) ) ;
#12422 = CIRCLE ( 'NONE', #1655, 27.00000000000001421 ) ;
#12423 = ORIENTED_EDGE ( 'NONE', *, *, #36629, .F. ) ;
#12424 = DIRECTION ( 'NONE',  ( 0.000000000000000000, 0.000000000000000000, 1.000000000000000000 ) ) ;
#12425 = ORIENTED_EDGE ( 'NONE', *, *, #71, .F. ) ;
#12426 = CARTESIAN_POINT ( 'NONE',  ( 69.99999662536839651, -3.469446951953614189E-15, -9.999999999999998224 ) ) ;
#12427 = EDGE_LOOP ( 'NONE', ( #33547, #6482 ) ) ;
#12428 = VERTEX_POINT ( 'NONE', #25802 ) ;
#12429 = AXIS2_PLACEMENT_3D ( 'NONE', #34124, #5795, #19854 ) ;
#12430 = FACE_OUTER_BOUND ( 'NONE', #13272, .T. ) ;
#12431 = DIRECTION ( 'NONE',  ( -0.000000000000000000, -0.000000000000000000, -1.000000000000000000 ) ) ;
#12432 = VERTEX_POINT ( 'NONE', #37051 ) ;
#12433 = ORIENTED_EDGE ( 'NONE', *, *, #5338, .T. ) ;
#12434 = CYLINDRICAL_SURFACE ( 'NONE', #28065, 2.000000000000001776 ) ;
#12435 = CIRCLE ( 'NONE', #27416, 5.999999999999999112 ) ;
#12436 = DIRECTION ( 'NONE',  ( 1.000000000000000000, 0.000000000000000000, 0.000000000000000000 ) ) ;
#12437 = ADVANCED_FACE ( 'NONE', ( #22974 ), #11521, .F. ) ;
#12438 = CARTESIAN_POINT ( 'NONE',  ( 72.99999662536836809, 8.660254037844394404, 12.50000000000000000 ) ) ;
#12439 = CARTESIAN_POINT ( 'NONE',  ( -5.000000000000000888, -1.045018621958868854, -3.717859243272141789 ) ) ;
#12440 = ORIENTED_EDGE ( 'NONE', *, *, #18723, .T. ) ;
#12441 = DIRECTION ( 'NONE',  ( 0.000000000000000000, 0.000000000000000000, 1.000000000000000000 ) ) ;
#12443 = CIRCLE ( 'NONE', #33423, 1.999999999999998224 ) ;
#12442 = DIRECTION ( 'NONE',  ( 0.000000000000000000, 0.000000000000000000, 1.000000000000000000 ) ) ;
#12444 = ORIENTED_EDGE ( 'NONE', *, *, #15982, .F. ) ;
#12445 = CARTESIAN_POINT ( 'NONE',  ( -60.00000337463104216, 51.96152422706639129, -9.999999999999998224 ) ) ;
#12446 = AXIS2_PLACEMENT_3D ( 'NONE', #1040, #32916, #6491 ) ;
#12447 = AXIS2_PLACEMENT_3D ( 'NONE', #8497, #776, #12022 ) ;
#12448 = DIRECTION ( 'NONE',  ( 0.000000000000000000, 0.000000000000000000, 1.000000000000000000 ) ) ;
#12449 = FACE_OUTER_BOUND ( 'NONE', #35860, .T. ) ;
#12451 = AXIS2_PLACEMENT_3D ( 'NONE', #16662, #13841, #28442 ) ;
#12450 = DIRECTION ( 'NONE',  ( 0.000000000000000000, 0.000000000000000000, -1.000000000000000000 ) ) ;
#12452 = CARTESIAN_POINT ( 'NONE',  ( 71.99999662536839651, 34.64101615137758472, -9.999999999999998224 ) ) ;
#12453 = AXIS2_PLACEMENT_3D ( 'NONE', #31691, #3192, #17446 ) ;
#12454 = CARTESIAN_POINT ( 'NONE',  ( 5.000000000000000888, 0.5616961504262232285, -0.5576671450146228892 ) ) ;
#12455 = VERTEX_POINT ( 'NONE', #34791 ) ;
#12456 = FACE_OUTER_BOUND ( 'NONE', #23705, .T. ) ;
#12457 = DIRECTION ( 'NONE',  ( 0.000000000000000000, 0.000000000000000000, 1.000000000000000000 ) ) ;
#12458 = CARTESIAN_POINT ( 'NONE',  ( 6.497954182785949224E-14, 5.999999999999947597, 27.50000000000000000 ) ) ;
#12459 = ORIENTED_EDGE ( 'NONE', *, *, #16052, .T. ) ;
#12460 = VECTOR ( 'NONE', #21806, 1000.000000000000000 ) ;
#12461 = ORIENTED_EDGE ( 'NONE', *, *, #6240, .T. ) ;
#12462 = ORIENTED_EDGE ( 'NONE', *, *, #23758, .F. ) ;
#12463 = EDGE_CURVE ( 'NONE', #20714, #12474, #32938, .T. ) ;
#12464 = DIRECTION ( 'NONE',  ( 1.000000000000000000, 0.000000000000000000, 0.000000000000000000 ) ) ;
#12465 = CARTESIAN_POINT ( 'NONE',  ( 18.03952607653389961, -86.20686977408767859, -5.000000000000000000 ) ) ;
#12466 = DIRECTION ( 'NONE',  ( 1.000000000000000000, 0.000000000000000000, 0.000000000000000000 ) ) ;
#12467 = CIRCLE ( 'NONE', #8892, 2.000000000000001776 ) ;
#12468 = PRODUCT_DEFINITION_SHAPE ( 'NONE', 'NONE',  #37134 ) ;
#12469 = CARTESIAN_POINT ( 'NONE',  ( -107.2742747693529566, -47.50000423952285900, 32.50001250000000397 ) ) ;
#12470 = CIRCLE ( 'NONE', #19689, 27.00000000000001776 ) ;
#12471 = CARTESIAN_POINT ( 'NONE',  ( -35.00000337463117717, -77.94228634059963667, 12.50000000000000000 ) ) ;
#12472 = VERTEX_POINT ( 'NONE', #36849 ) ;
#12473 = DIRECTION ( 'NONE',  ( 0.000000000000000000, 0.000000000000000000, 1.000000000000000000 ) ) ;
#12474 = VERTEX_POINT ( 'NONE', #19803 ) ;
#12475 = AXIS2_PLACEMENT_3D ( 'NONE', #16720, #28145, #13158 ) ;
#12476 = FACE_BOUND ( 'NONE', #35886, .T. ) ;
#12477 = CIRCLE ( 'NONE', #11860, 2.000000000000000000 ) ;
#12478 = CARTESIAN_POINT ( 'NONE',  ( 37.50000000000000000, -103.4105893997321743, 32.50000000000000000 ) ) ;
#12479 = AXIS2_PLACEMENT_3D ( 'NONE', #16680, #31450, #31271 ) ;
#12480 = DIRECTION ( 'NONE',  ( 0.000000000000000000, 0.000000000000000000, 1.000000000000000000 ) ) ;
#12481 = DIRECTION ( 'NONE',  ( 1.000000000000000000, 0.000000000000000000, 0.000000000000000000 ) ) ;
#12482 = EDGE_LOOP ( 'NONE', ( #6558, #13714, #23137, #20124 ) ) ;
#12483 = CARTESIAN_POINT ( 'NONE',  ( 56.99999662536844625, 60.62177826491077326, 17.49999999999999645 ) ) ;
#12484 = ADVANCED_FACE ( 'NONE', ( #9080 ), #31765, .F. ) ;
#12485 = CARTESIAN_POINT ( 'NONE',  ( 3.851086116668511750E-13, -54.99999999999999289, 10.70000000000000107 ) ) ;
#12486 = AXIS2_PLACEMENT_3D ( 'NONE', #7740, #30604, #4921 ) ;
#12487 = ADVANCED_FACE ( 'NONE', ( #20504 ), #19972, .T. ) ;
#12488 = CARTESIAN_POINT ( 'NONE',  ( -15.97563234535668109, 90.60231327712331506, -4.999999999999997335 ) ) ;
#12489 = AXIS2_PLACEMENT_3D ( 'NONE', #10565, #33633, #33450 ) ;
#12490 = CARTESIAN_POINT ( 'NONE',  ( -5.000000000000000888, 2.886751345948107783, -5.700000000000000178 ) ) ;
#12491 = CARTESIAN_POINT ( 'NONE',  ( -55.00000337463107059, 43.30127018922197379, -9.999999999999998224 ) ) ;
#12492 = ORIENTED_EDGE ( 'NONE', *, *, #20477, .T. ) ;
#12493 = DIRECTION ( 'NONE',  ( 0.000000000000000000, 0.4999999999999951150, -0.8660254037844414832 ) ) ;
#12494 = EDGE_CURVE ( 'NONE', #17074, #6836, #7194, .T. ) ;
#12495 = CARTESIAN_POINT ( 'NONE',  ( 4.390739357591696154E-15, -5.773502691896305272, -3.984345921091785758 ) ) ;
#12496 = DIRECTION ( 'NONE',  ( -1.000000000000000000, 0.000000000000000000, 0.000000000000000000 ) ) ;
#12497 = VERTEX_POINT ( 'NONE', #14357 ) ;
#12498 = EDGE_CURVE ( 'NONE', #9458, #8382, #20353, .T. ) ;
#12499 = EDGE_LOOP ( 'NONE', ( #12247, #27128, #1198, #16461 ) ) ;
#12500 = AXIS2_PLACEMENT_3D ( 'NONE', #33551, #13837, #16290 ) ;
#12501 = ORIENTED_EDGE ( 'NONE', *, *, #25265, .T. ) ;
#12502 = VECTOR ( 'NONE', #10005, 1000.000000000000000 ) ;
#12503 = CARTESIAN_POINT ( 'NONE',  ( 72.99999662536836809, 43.30127018922198801, -9.999999999999998224 ) ) ;
#12504 = DIRECTION ( 'NONE',  ( 0.000000000000000000, 0.000000000000000000, 1.000000000000000000 ) ) ;
#12505 = CARTESIAN_POINT ( 'NONE',  ( -16.49657687835744113, 93.55673653615994567, -5.000000000000000000 ) ) ;
#12506 = ADVANCED_FACE ( 'NONE', ( #31584 ), #31928, .F. ) ;
#12507 = DIRECTION ( 'NONE',  ( 0.000000000000000000, 0.000000000000000000, -1.000000000000000000 ) ) ;
#12508 = DIRECTION ( 'NONE',  ( 0.000000000000000000, -0.8660254037844421493, -0.4999999999999942268 ) ) ;
#12510 = DIRECTION ( 'NONE',  ( 0.000000000000000000, 0.000000000000000000, 1.000000000000000000 ) ) ;
#12509 = AXIS2_PLACEMENT_3D ( 'NONE', #35601, #23587, #9713 ) ;
#12511 = ORIENTED_EDGE ( 'NONE', *, *, #28005, .T. ) ;
#12512 = VERTEX_POINT ( 'NONE', #25966 ) ;
#12513 = FACE_OUTER_BOUND ( 'NONE', #15944, .T. ) ;
#12514 = AXIS2_PLACEMENT_3D ( 'NONE', #31429, #118, #11548 ) ;
#12515 = CARTESIAN_POINT ( 'NONE',  ( -70.00000337463100664, -17.32050807568882078, 17.49999999999999645 ) ) ;
#12516 = EDGE_LOOP ( 'NONE', ( #22063, #17136, #21178, #19865, #23960 ) ) ;
#12517 = CIRCLE ( 'NONE', #20986, 2.000000000000001776 ) ;
#12518 = DIRECTION ( 'NONE',  ( -0.000000000000000000, -0.000000000000000000, 1.000000000000000000 ) ) ;
#12519 = ORIENTED_EDGE ( 'NONE', *, *, #20197, .F. ) ;
#12520 = CIRCLE ( 'NONE', #26913, 2.000000000000001776 ) ;
#12521 = DIRECTION ( 'NONE',  ( 0.000000000000000000, 0.4999999999999951150, -0.8660254037844414832 ) ) ;
#12522 = AXIS2_PLACEMENT_3D ( 'NONE', #35403, #32177, #32546 ) ;
#12523 = ORIENTED_EDGE ( 'NONE', *, *, #23362, .F. ) ;
#12524 = ORIENTED_EDGE ( 'NONE', *, *, #6887, .T. ) ;
#12525 = EDGE_CURVE ( 'NONE', #1000, #27610, #28779, .T. ) ;
#12526 = VECTOR ( 'NONE', #6551, 1000.000000000000000 ) ;
#12527 = CARTESIAN_POINT ( 'NONE',  ( 56.99999662536844625, 43.30127018922198801, 17.49999999999999645 ) ) ;
#12528 = ORIENTED_EDGE ( 'NONE', *, *, #9882, .F. ) ;
#12529 = SURFACE_STYLE_FILL_AREA ( #26786 ) ;
#12530 = DIRECTION ( 'NONE',  ( 0.7071067811865461294, -0.7071067811865489050, 0.000000000000000000 ) ) ;
#12531 = CARTESIAN_POINT ( 'NONE',  ( -80.00000337463094979, 17.32050807568878525, 12.50000000000000000 ) ) ;
#12532 = CARTESIAN_POINT ( 'NONE',  ( 35.19434990244975126, -52.39915983220758022, -4.999999999999997335 ) ) ;
#12533 = ORIENTED_EDGE ( 'NONE', *, *, #9083, .F. ) ;
#12534 =( REPRESENTATION_RELATIONSHIP ('NONE','NONE', #15268, #35880 ) REPRESENTATION_RELATIONSHIP_WITH_TRANSFORMATION ( #16607 )SHAPE_REPRESENTATION_RELATIONSHIP( ) );
#12535 = ORIENTED_EDGE ( 'NONE', *, *, #22497, .F. ) ;
#12536 = EDGE_CURVE ( 'NONE', #25059, #29874, #16191, .T. ) ;
#12537 = CIRCLE ( 'NONE', #29298, 2.000000000000001776 ) ;
#12538 = ORIENTED_EDGE ( 'NONE', *, *, #27063, .T. ) ;
#12539 = VERTEX_POINT ( 'NONE', #14528 ) ;
#12540 = VECTOR ( 'NONE', #12480, 1000.000000000000000 ) ;
#12541 = ADVANCED_FACE ( 'NONE', ( #16971 ), #6093, .T. ) ;
#12542 = ORIENTED_EDGE ( 'NONE', *, *, #627, .T. ) ;
#12543 = LINE ( 'NONE', #32799, #33802 ) ;
#12544 = FACE_OUTER_BOUND ( 'NONE', #21221, .T. ) ;
#12545 = EDGE_LOOP ( 'NONE', ( #4605, #7622 ) ) ;
#12546 = CYLINDRICAL_SURFACE ( 'NONE', #32832, 2.000000000000001776 ) ;
#12547 = CARTESIAN_POINT ( 'NONE',  ( 102.9785771442050333, 33.47437999733440250, 32.50000000000000000 ) ) ;
#12548 = CIRCLE ( 'NONE', #7780, 30.00000000000000000 ) ;
#12549 = CARTESIAN_POINT ( 'NONE',  ( 87.99999662536828282, 2.449293598294703949E-16, -9.999999999999998224 ) ) ;
#12550 = ORIENTED_EDGE ( 'NONE', *, *, #21405, .F. ) ;
#12551 = DIRECTION ( 'NONE',  ( 0.000000000000000000, 0.000000000000000000, -1.000000000000000000 ) ) ;
#12552 = DIRECTION ( 'NONE',  ( 1.000000000000000000, 0.000000000000000000, 0.000000000000000000 ) ) ;
#12553 = AXIS2_PLACEMENT_3D ( 'NONE', #267, #20158, #6268 ) ;
#12554 = DIRECTION ( 'NONE',  ( -1.000000000000000000, -0.000000000000000000, -0.000000000000000000 ) ) ;
#12555 = VERTEX_POINT ( 'NONE', #23157 ) ;
#12556 = CYLINDRICAL_SURFACE ( 'NONE', #1090, 2.000000000000001776 ) ;
#12557 = AXIS2_PLACEMENT_3D ( 'NONE', #2769, #14202, #11392 ) ;
#12558 = CARTESIAN_POINT ( 'NONE',  ( 3.000000000000000000, 2.935248768560057453, -3.903127820947815962E-15 ) ) ;
#12559 = ORIENTED_EDGE ( 'NONE', *, *, #26571, .T. ) ;
#12560 = ORIENTED_EDGE ( 'NONE', *, *, #5687, .F. ) ;
#12561 = EDGE_CURVE ( 'NONE', #23429, #24999, #22806, .T. ) ;
#12562 = CARTESIAN_POINT ( 'NONE',  ( -55.00000337463107059, 60.62177826491078747, 12.50000000000000000 ) ) ;
#12563 = CARTESIAN_POINT ( 'NONE',  ( -15.97563234535668109, 90.60231327712331506, 12.49999999999999822 ) ) ;
#12564 = FACE_OUTER_BOUND ( 'NONE', #13666, .T. ) ;
#12565 = DIRECTION ( 'NONE',  ( 1.000000000000000000, 0.000000000000000000, 0.000000000000000000 ) ) ;
#12566 = ORIENTED_EDGE ( 'NONE', *, *, #36316, .F. ) ;
#12567 = EDGE_CURVE ( 'NONE', #17104, #28322, #3272, .T. ) ;
#12568 = CARTESIAN_POINT ( 'NONE',  ( -51.68138994340220904, -113.8157894736842053, 27.50000000000000000 ) ) ;
#12569 = DIRECTION ( 'NONE',  ( 1.000000000000000000, 0.000000000000000000, 0.000000000000000000 ) ) ;
#12570 = VERTEX_POINT ( 'NONE', #15460 ) ;
#12571 = ADVANCED_FACE ( 'NONE', ( #35163 ), #20696, .T. ) ;
#12572 = AXIS2_PLACEMENT_3D ( 'NONE', #9047, #20470, #31892 ) ;
#12573 = DIRECTION ( 'NONE',  ( 0.000000000000000000, 0.000000000000000000, 1.000000000000000000 ) ) ;
#12574 = AXIS2_PLACEMENT_3D ( 'NONE', #11437, #3181, #17802 ) ;
#12575 = ORIENTED_EDGE ( 'NONE', *, *, #32520, .T. ) ;
#12576 = DIRECTION ( 'NONE',  ( 0.000000000000000000, 0.000000000000000000, 1.000000000000000000 ) ) ;
#12577 = DIRECTION ( 'NONE',  ( 0.000000000000000000, 0.000000000000000000, 1.000000000000000000 ) ) ;
#12578 = CIRCLE ( 'NONE', #33566, 2.000000000000001776 ) ;
#12579 = CARTESIAN_POINT ( 'NONE',  ( -47.00000337463112743, -60.62177826491080168, 12.50000000000000000 ) ) ;
#12580 = EDGE_LOOP ( 'NONE', ( #1431, #36659, #10968, #20502 ) ) ;
#12581 = ORIENTED_EDGE ( 'NONE', *, *, #6238, .T. ) ;
#12582 = EDGE_CURVE ( 'NONE', #6533, #6253, #15083, .T. ) ;
#12583 = EDGE_LOOP ( 'NONE', ( #26130, #23615, #4644, #16869 ) ) ;
#12584 = CARTESIAN_POINT ( 'NONE',  ( -55.00000337463110611, -43.30127018922202353, -5.000000000000000000 ) ) ;
#12585 = FACE_BOUND ( 'NONE', #17140, .T. ) ;
#12586 = AXIS2_PLACEMENT_3D ( 'NONE', #34029, #3243, #9052 ) ;
#12587 = DIRECTION ( 'NONE',  ( 1.000000000000000000, 0.000000000000000000, 0.000000000000000000 ) ) ;
#12588 = DIRECTION ( 'NONE',  ( 0.000000000000000000, 0.000000000000000000, 1.000000000000000000 ) ) ;
#12589 = CYLINDRICAL_SURFACE ( 'NONE', #20115, 2.000000000000001776 ) ;
#12590 = EDGE_LOOP ( 'NONE', ( #6047, #3207, #6107, #15619 ) ) ;
#12591 = CARTESIAN_POINT ( 'NONE',  ( -3.374631289687624047E-06, -69.28203230275519786, -9.999999999999998224 ) ) ;
#12592 = DIRECTION ( 'NONE',  ( 0.000000000000000000, 0.000000000000000000, 1.000000000000000000 ) ) ;
#12593 = AXIS2_PLACEMENT_3D ( 'NONE', #27764, #19888, #25335 ) ;
#12594 = DIRECTION ( 'NONE',  ( -1.000000000000000000, 0.000000000000000000, 0.000000000000000000 ) ) ;
#12595 = VERTEX_POINT ( 'NONE', #26896 ) ;
#12596 = CYLINDRICAL_SURFACE ( 'NONE', #19622, 2.000000000000001776 ) ;
#12597 = PLANE ( 'NONE',  #8775 ) ;
#12598 = DIRECTION ( 'NONE',  ( 0.000000000000000000, 0.000000000000000000, 1.000000000000000000 ) ) ;
#12599 = VERTEX_POINT ( 'NONE', #26344 ) ;
#12600 = VERTEX_POINT ( 'NONE', #21763 ) ;
#12601 = EDGE_CURVE ( 'NONE', #19493, #23515, #5989, .T. ) ;
#12602 = FACE_OUTER_BOUND ( 'NONE', #18144, .T. ) ;
#12603 = DIRECTION ( 'NONE',  ( 0.000000000000000000, 0.000000000000000000, 1.000000000000000000 ) ) ;
#12604 = EDGE_CURVE ( 'NONE', #25787, #14689, #824, .T. ) ;
#12605 = CARTESIAN_POINT ( 'NONE',  ( -0.9112620892301054321, -5.247385279376963751, -1.160540885688338131 ) ) ;
#12606 = ORIENTED_EDGE ( 'NONE', *, *, #806, .T. ) ;
#12607 = EDGE_LOOP ( 'NONE', ( #1665, #27230, #2914, #6865, #28013, #11557, #6341, #1751 ) ) ;
#12608 = ORIENTED_EDGE ( 'NONE', *, *, #11258, .F. ) ;
#12609 = EDGE_CURVE ( 'NONE', #36868, #10255, #26936, .T. ) ;
#12610 = CARTESIAN_POINT ( 'NONE',  ( -52.39915983220772233, -35.19434990244957362, -4.999999999999997335 ) ) ;
#12611 = ORIENTED_EDGE ( 'NONE', *, *, #35342, .T. ) ;
#12613 = EDGE_CURVE ( 'NONE', #17979, #8132, #27588, .T. ) ;
#12612 = VERTEX_POINT ( 'NONE', #29502 ) ;
#12614 = DIRECTION ( 'NONE',  ( -1.000000000000000000, 1.066533692637591978E-14, 0.000000000000000000 ) ) ;
#12615 = VERTEX_POINT ( 'NONE', #29685 ) ;
#12616 = EDGE_CURVE ( 'NONE', #25448, #13993, #4020, .T. ) ;
#12617 = ORIENTED_EDGE ( 'NONE', *, *, #35879, .T. ) ;
#12618 = DIRECTION ( 'NONE',  ( 0.000000000000000000, 0.000000000000000000, 1.000000000000000000 ) ) ;
#12620 = CIRCLE ( 'NONE', #17423, 2.000000000000001776 ) ;
#12619 = CYLINDRICAL_SURFACE ( 'NONE', #8702, 3.500000000000003109 ) ;
#12621 = ORIENTED_EDGE ( 'NONE', *, *, #33840, .T. ) ;
#12622 = ORIENTED_EDGE ( 'NONE', *, *, #16881, .T. ) ;
#12623 = CARTESIAN_POINT ( 'NONE',  ( -47.00000337463111322, -77.94228634059960825, 12.50000000000000000 ) ) ;
#12624 = CARTESIAN_POINT ( 'NONE',  ( -82.27241335952211898, -47.49999999999924682, 32.50002500000000083 ) ) ;
#12625 = ADVANCED_FACE ( 'NONE', ( #18256 ), #1718, .F. ) ;
#12626 = DIRECTION ( 'NONE',  ( -1.000000000000000000, 0.000000000000000000, 0.000000000000000000 ) ) ;
#12627 = EDGE_CURVE ( 'NONE', #755, #623, #29341, .T. ) ;
#12628 = CARTESIAN_POINT ( 'NONE',  ( -5.000000000000000888, -2.094350244328533339, -3.837520945129150540 ) ) ;
#12629 = EDGE_CURVE ( 'NONE', #6799, #17677, #31141, .T. ) ;
#12630 = VERTEX_POINT ( 'NONE', #32330 ) ;
#12631 = CARTESIAN_POINT ( 'NONE',  ( -68.00000337463099243, -2.428612866367529932E-14, -9.999999999999998224 ) ) ;
#12632 = ADVANCED_FACE ( 'NONE', ( #10327 ), #7518, .T. ) ;
#12633 = ORIENTED_EDGE ( 'NONE', *, *, #36634, .F. ) ;
#12634 = DIRECTION ( 'NONE',  ( 1.000000000000000000, 0.000000000000000000, 0.000000000000000000 ) ) ;
#12635 = EDGE_CURVE ( 'NONE', #18828, #32378, #20943, .T. ) ;
#12636 = CARTESIAN_POINT ( 'NONE',  ( 62.99999662536841072, -25.98076211353320275, 12.50000000000000000 ) ) ;
#12637 = CYLINDRICAL_SURFACE ( 'NONE', #1634, 3.499999999999989342 ) ;
#12638 = CARTESIAN_POINT ( 'NONE',  ( -2.269462870248036555E-13, -65.00000000000000000, 12.49999999999999822 ) ) ;
#12639 = DIRECTION ( 'NONE',  ( 0.000000000000000000, 0.000000000000000000, 1.000000000000000000 ) ) ;
#12640 = DIRECTION ( 'NONE',  ( -0.000000000000000000, -0.000000000000000000, 1.000000000000000000 ) ) ;
#12641 = EDGE_LOOP ( 'NONE', ( #20873, #444 ) ) ;
#12642 = DIRECTION ( 'NONE',  ( -0.000000000000000000, -0.000000000000000000, -1.000000000000000000 ) ) ;
#12643 = CIRCLE ( 'NONE', #10273, 2.000000000000001776 ) ;
#12644 = CYLINDRICAL_SURFACE ( 'NONE', #8166, 3.499999999999991562 ) ;
#12645 = DIRECTION ( 'NONE',  ( -0.000000000000000000, -0.000000000000000000, 1.000000000000000000 ) ) ;
#12646 = ORIENTED_EDGE ( 'NONE', *, *, #19549, .F. ) ;
#12647 = VERTEX_POINT ( 'NONE', #3655 ) ;
#12648 = ORIENTED_EDGE ( 'NONE', *, *, #12293, .T. ) ;
#12649 = DIRECTION ( 'NONE',  ( 1.000000000000000000, 0.000000000000000000, 0.000000000000000000 ) ) ;
#12650 = CARTESIAN_POINT ( 'NONE',  ( -72.00000337463100664, -17.32050807568882078, -9.999999999999998224 ) ) ;
#12651 = CARTESIAN_POINT ( 'NONE',  ( 83.10590767357027175, -8.018049208621958357, 12.50000000000000000 ) ) ;
#12652 = DIRECTION ( 'NONE',  ( 0.000000000000000000, -0.000000000000000000, -1.000000000000000000 ) ) ;
#12653 = CARTESIAN_POINT ( 'NONE',  ( 59.29837256189581041, 31.02796211690887418, -4.999999999999997335 ) ) ;
#12654 = CARTESIAN_POINT ( 'NONE',  ( 61.99999662536842493, -51.96152422706639840, -9.999999999999998224 ) ) ;
#12655 = ORIENTED_EDGE ( 'NONE', *, *, #19270, .T. ) ;
#12656 = PLANE ( 'NONE',  #10004 ) ;
#12657 = ORIENTED_EDGE ( 'NONE', *, *, #9585, .F. ) ;
#12658 = FACE_BOUND ( 'NONE', #36987, .T. ) ;
#12659 = DIRECTION ( 'NONE',  ( 0.000000000000000000, 0.000000000000000000, -1.000000000000000000 ) ) ;
#12660 = DIRECTION ( 'NONE',  ( 1.000000000000000000, 0.000000000000000000, 0.000000000000000000 ) ) ;
#12661 = VECTOR ( 'NONE', #9464, 1000.000000000000000 ) ;
#12662 = DIRECTION ( 'NONE',  ( 1.000000000000000000, 0.000000000000000000, 0.000000000000000000 ) ) ;
#12663 = ORIENTED_EDGE ( 'NONE', *, *, #3240, .T. ) ;
#12664 = CARTESIAN_POINT ( 'NONE',  ( 5.000000000000000888, 0.9828435001097636237, -5.956909652965543422 ) ) ;
#12665 = AXIS2_PLACEMENT_3D ( 'NONE', #17622, #29437, #3755 ) ;
#12666 = PRODUCT_CONTEXT ( 'NONE', #3174, 'mechanical' ) ;
#12667 = PLANE ( 'NONE',  #32036 ) ;
#12668 = EDGE_CURVE ( 'NONE', #19047, #14960, #36036, .T. ) ;
#12669 = FACE_BOUND ( 'NONE', #27643, .T. ) ;
#12670 = CARTESIAN_POINT ( 'NONE',  ( 66.99999662536841072, -25.98076211353320275, -5.000000000000000000 ) ) ;
#12671 = ADVANCED_FACE ( 'NONE', ( #4727 ), #6329, .F. ) ;
#12672 = ORIENTED_EDGE ( 'NONE', *, *, #16828, .T. ) ;
#12673 = DIRECTION ( 'NONE',  ( 1.000000000000000000, 0.000000000000000000, 0.000000000000000000 ) ) ;
#12674 = DIRECTION ( 'NONE',  ( 0.000000000000000000, -0.000000000000000000, 1.000000000000000000 ) ) ;
#12675 = DIRECTION ( 'NONE',  ( -0.000000000000000000, -0.000000000000000000, -1.000000000000000000 ) ) ;
#12676 = ORIENTED_EDGE ( 'NONE', *, *, #9193, .F. ) ;
#12677 = EDGE_LOOP ( 'NONE', ( #4437, #33561, #193, #32415 ) ) ;
#12678 = ORIENTED_EDGE ( 'NONE', *, *, #35531, .F. ) ;
#12679 = CARTESIAN_POINT ( 'NONE',  ( -60.00000337463104216, 34.64101615137757051, 12.50000000000000000 ) ) ;
#12680 = DIRECTION ( 'NONE',  ( -1.000000000000000000, 0.000000000000000000, 0.000000000000000000 ) ) ;
#12681 = DIRECTION ( 'NONE',  ( 0.000000000000000000, 0.000000000000000000, 1.000000000000000000 ) ) ;
#12682 = AXIS2_PLACEMENT_3D ( 'NONE', #18207, #27025, #29640 ) ;
#12683 = DIRECTION ( 'NONE',  ( 1.000000000000000000, 0.000000000000000000, 0.000000000000000000 ) ) ;
#12684 = CARTESIAN_POINT ( 'NONE',  ( -57.00000337463107059, 43.30127018922197379, -9.999999999999998224 ) ) ;
#12685 = CARTESIAN_POINT ( 'NONE',  ( -77.93337651276257816, 72.12094976675054170, 32.50001250000000397 ) ) ;
#12686 = EDGE_CURVE ( 'NONE', #13489, #22972, #28142, .T. ) ;
#12687 = ORIENTED_EDGE ( 'NONE', *, *, #9501, .F. ) ;
#12688 = ORIENTED_EDGE ( 'NONE', *, *, #3206, .T. ) ;
#12689 = SURFACE_STYLE_FILL_AREA ( #15530 ) ;
#12690 = CARTESIAN_POINT ( 'NONE',  ( -22.00000337463124112, 69.28203230275516944, -5.000000000000000000 ) ) ;
#12691 = EDGE_LOOP ( 'NONE', ( #5212, #2645 ) ) ;
#12692 = DIRECTION ( 'NONE',  ( -1.000000000000000000, 0.000000000000000000, 0.000000000000000000 ) ) ;
#12693 = ORIENTED_EDGE ( 'NONE', *, *, #20415, .F. ) ;
#12694 = PLANE ( 'NONE',  #27301 ) ;
#12695 = AXIS2_PLACEMENT_3D ( 'NONE', #14296, #23846, #15027 ) ;
#12696 = ADVANCED_FACE ( 'NONE', ( #35023 ), #26404, .F. ) ;
#12697 = VECTOR ( 'NONE', #13901, 1000.000000000000000 ) ;
#12698 = FACE_BOUND ( 'NONE', #11503, .T. ) ;
#12699 = VERTEX_POINT ( 'NONE', #32392 ) ;
#12700 = VERTEX_POINT ( 'NONE', #34677 ) ;
#12701 = CARTESIAN_POINT ( 'NONE',  ( 69.99999662536839651, -17.32050807568879947, -9.999999999999998224 ) ) ;
#12702 = ORIENTED_EDGE ( 'NONE', *, *, #20644, .T. ) ;
#12703 = DIRECTION ( 'NONE',  ( -0.000000000000000000, -0.000000000000000000, 1.000000000000000000 ) ) ;
#12704 = AXIS2_PLACEMENT_3D ( 'NONE', #175, #34506, #8814 ) ;
#12705 = PLANE ( 'NONE',  #35311 ) ;
#12706 = FACE_OUTER_BOUND ( 'NONE', #8360, .T. ) ;
#12707 = ADVANCED_FACE ( 'NONE', ( #705 ), #17767, .F. ) ;
#12708 = ORIENTED_EDGE ( 'NONE', *, *, #25836, .T. ) ;
#12709 = EDGE_LOOP ( 'NONE', ( #19141, #841, #2663, #19604 ) ) ;
#12710 = ORIENTED_EDGE ( 'NONE', *, *, #9671, .T. ) ;
#12711 = ORIENTED_EDGE ( 'NONE', *, *, #3656, .F. ) ;
#12712 = CARTESIAN_POINT ( 'NONE',  ( -80.00000337463094979, 17.32050807568878525, -5.000000000000000000 ) ) ;
#12713 = CARTESIAN_POINT ( 'NONE',  ( -75.00000337463097821, 25.98076211353318854, 12.50000000000000000 ) ) ;
#12714 = ORIENTED_EDGE ( 'NONE', *, *, #36011, .T. ) ;
#12715 = CARTESIAN_POINT ( 'NONE',  ( -5.000000000000000000, -0.2835658343809315807, -0.5205273423269579647 ) ) ;
#12716 = CARTESIAN_POINT ( 'NONE',  ( -50.00000337463110611, -69.28203230275519786, -9.999999999999998224 ) ) ;
#12717 = VERTEX_POINT ( 'NONE', #9324 ) ;
#12718 = DIRECTION ( 'NONE',  ( 1.000000000000000000, 0.000000000000000000, 0.000000000000000000 ) ) ;
#12719 = AXIS2_PLACEMENT_3D ( 'NONE', #4145, #12731, #9937 ) ;
#12720 = CARTESIAN_POINT ( 'NONE',  ( 0.4012132626380134348, 5.541862106709760205, -0.4203182062997347090 ) ) ;
#12721 = EDGE_CURVE ( 'NONE', #4461, #27222, #32340, .T. ) ;
#12722 = DIRECTION ( 'NONE',  ( 0.8660254037844344888, -0.5000000000000069944, 0.000000000000000000 ) ) ;
#12723 = ORIENTED_EDGE ( 'NONE', *, *, #25735, .F. ) ;
#12724 = CARTESIAN_POINT ( 'NONE',  ( -63.00000337463104927, -25.98076211353322051, 17.49999999999999645 ) ) ;
#12725 = CARTESIAN_POINT ( 'NONE',  ( -70.00000337463102085, -34.64101615137762025, -9.999999999999998224 ) ) ;
#12726 = EDGE_CURVE ( 'NONE', #25226, #11378, #10803, .T. ) ;
#12727 = VERTEX_POINT ( 'NONE', #20762 ) ;
#12728 = ORIENTED_EDGE ( 'NONE', *, *, #34398, .T. ) ;
#12729 = DIRECTION ( 'NONE',  ( 1.000000000000000000, 0.000000000000000000, 0.000000000000000000 ) ) ;
#12730 = AXIS2_PLACEMENT_3D ( 'NONE', #29898, #15657, #23722 ) ;
#12731 = DIRECTION ( 'NONE',  ( 0.000000000000000000, 0.000000000000000000, -1.000000000000000000 ) ) ;
#12732 = DIRECTION ( 'NONE',  ( 0.000000000000000000, 0.000000000000000000, -1.000000000000000000 ) ) ;
#12733 = AXIS2_PLACEMENT_3D ( 'NONE', #19582, #1781, #4403 ) ;
#12734 = CYLINDRICAL_SURFACE ( 'NONE', #14965, 2.000000000000001776 ) ;
#12735 = EDGE_CURVE ( 'NONE', #625, #24999, #35374, .T. ) ;
#12736 = ORIENTED_EDGE ( 'NONE', *, *, #26397, .F. ) ;
#12737 = DIRECTION ( 'NONE',  ( -0.000000000000000000, -0.000000000000000000, -1.000000000000000000 ) ) ;
#12738 = LINE ( 'NONE', #6587, #16547 ) ;
#12739 = EDGE_CURVE ( 'NONE', #20566, #27049, #23975, .T. ) ;
#12740 = VERTEX_POINT ( 'NONE', #29756 ) ;
#12741 = APPLICATION_CONTEXT ( 'automotive_design' ) ;
#12742 = DIRECTION ( 'NONE',  ( 0.000000000000000000, 0.000000000000000000, 1.000000000000000000 ) ) ;
#12743 = CIRCLE ( 'NONE', #22964, 3.500000000000003109 ) ;
#12744 = ORIENTED_EDGE ( 'NONE', *, *, #32087, .F. ) ;
#12745 = DIRECTION ( 'NONE',  ( 0.000000000000000000, 0.000000000000000000, -1.000000000000000000 ) ) ;
#12746 = CIRCLE ( 'NONE', #34931, 2.000000000000001776 ) ;
#12747 = FACE_OUTER_BOUND ( 'NONE', #36477, .T. ) ;
#12748 = DIRECTION ( 'NONE',  ( 0.000000000000000000, 0.000000000000000000, -1.000000000000000000 ) ) ;
#12749 = ADVANCED_FACE ( 'NONE', ( #31816 ), #26020, .F. ) ;
#12750 = ORIENTED_EDGE ( 'NONE', *, *, #10024, .T. ) ;
#12751 = ORIENTED_EDGE ( 'NONE', *, *, #30736, .T. ) ;
#12752 = ADVANCED_FACE ( 'NONE', ( #15137 ), #17576, .F. ) ;
#12753 = ORIENTED_EDGE ( 'NONE', *, *, #25679, .T. ) ;
#12754 = DIRECTION ( 'NONE',  ( -0.7071067811865388020, 0.7071067811865563435, 0.000000000000000000 ) ) ;
#12755 = AXIS2_PLACEMENT_3D ( 'NONE', #18616, #6422, #12594 ) ;
#12756 = DIRECTION ( 'NONE',  ( 0.000000000000000000, 0.000000000000000000, 1.000000000000000000 ) ) ;
#12757 = DIRECTION ( 'NONE',  ( -1.000000000000000000, 0.000000000000000000, 0.000000000000000000 ) ) ;
#12758 = CYLINDRICAL_SURFACE ( 'NONE', #17484, 8.500000000000000000 ) ;
#12759 = CARTESIAN_POINT ( 'NONE',  ( 69.99999662536838230, -51.96152422706639840, -9.999999999999998224 ) ) ;
#12760 = VERTEX_POINT ( 'NONE', #23410 ) ;
#12761 = FACE_OUTER_BOUND ( 'NONE', #13524, .T. ) ;
#12762 = EDGE_CURVE ( 'NONE', #18228, #34831, #36560, .T. ) ;
#12763 = PRODUCT_DEFINITION_SHAPE ( 'NONE', 'NONE',  #37135 ) ;
#12764 = DIRECTION ( 'NONE',  ( 1.000000000000000000, 0.000000000000000000, 0.000000000000000000 ) ) ;
#12765 = ADVANCED_FACE ( 'NONE', ( #23777 ), #29557, .F. ) ;
#12766 = DIRECTION ( 'NONE',  ( 0.000000000000000000, 0.000000000000000000, 1.000000000000000000 ) ) ;
#12767 = EDGE_LOOP ( 'NONE', ( #3297, #34605, #10318, #33696 ) ) ;
#12768 = CARTESIAN_POINT ( 'NONE',  ( 108.3061974404898820, 19.22934205794938478, 32.50000000000000000 ) ) ;
#12769 = PLANE ( 'NONE',  #19576 ) ;
#12770 = CIRCLE ( 'NONE', #17567, 3.000000000000003553 ) ;
#12771 = ORIENTED_EDGE ( 'NONE', *, *, #9315, .T. ) ;
#12772 = AXIS2_PLACEMENT_3D ( 'NONE', #19089, #35416, #35588 ) ;
#12773 = ORIENTED_EDGE ( 'NONE', *, *, #15903, .F. ) ;
#12774 = CARTESIAN_POINT ( 'NONE',  ( -60.00000337463104216, 51.96152422706639129, -9.999999999999998224 ) ) ;
#12775 = CARTESIAN_POINT ( 'NONE',  ( 2.999996625368676728, -77.94228634059960825, 17.49999999999999645 ) ) ;
#12776 = LINE ( 'NONE', #23882, #17800 ) ;
#12777 = ORIENTED_EDGE ( 'NONE', *, *, #25113, .F. ) ;
#12778 = ORIENTED_EDGE ( 'NONE', *, *, #24117, .T. ) ;
#12779 = ORIENTED_EDGE ( 'NONE', *, *, #30269, .T. ) ;
#12780 = VECTOR ( 'NONE', #14298, 1000.000000000000000 ) ;
#12781 = CARTESIAN_POINT ( 'NONE',  ( -63.10544949267008974, -59.98094631475026262, 12.50000000000000000 ) ) ;
#12782 = ADVANCED_FACE ( 'NONE', ( #15325 ), #529, .F. ) ;
#12783 = CIRCLE ( 'NONE', #7450, 4.700000000000000178 ) ;
#12784 = ORIENTED_EDGE ( 'NONE', *, *, #11134, .F. ) ;
#12785 = ORIENTED_EDGE ( 'NONE', *, *, #4118, .F. ) ;
#12786 = DIRECTION ( 'NONE',  ( 1.000000000000000000, 0.000000000000000000, 0.000000000000000000 ) ) ;
#12787 = EDGE_LOOP ( 'NONE', ( #35047, #32710, #15889, #29917, #35592, #36917, #26796, #18696 ) ) ;
#12788 = ORIENTED_EDGE ( 'NONE', *, *, #24324, .T. ) ;
#12789 = CARTESIAN_POINT ( 'NONE',  ( -3.368272016354731502, 78.44802294027070388, 32.49999999999999289 ) ) ;
#12790 = DIRECTION ( 'NONE',  ( 1.000000000000000000, 0.000000000000000000, 0.000000000000000000 ) ) ;
#12791 = ORIENTED_EDGE ( 'NONE', *, *, #12134, .F. ) ;
#12792 = VERTEX_POINT ( 'NONE', #34843 ) ;
#12793 = FACE_OUTER_BOUND ( 'NONE', #9147, .T. ) ;
#12794 = CARTESIAN_POINT ( 'NONE',  ( 5.253368672218635460, 3.033033817057773529, -4.359491423763652840 ) ) ;
#12795 = DIRECTION ( 'NONE',  ( -0.000000000000000000, -0.000000000000000000, -1.000000000000000000 ) ) ;
#12796 = DIRECTION ( 'NONE',  ( 1.000000000000000000, 0.000000000000000000, 0.000000000000000000 ) ) ;
#12797 = AXIS2_PLACEMENT_3D ( 'NONE', #36426, #25183, #32522 ) ;
#12798 = EDGE_CURVE ( 'NONE', #630, #1054, #22182, .T. ) ;
#12799 = ORIENTED_EDGE ( 'NONE', *, *, #26435, .F. ) ;
#12800 = CARTESIAN_POINT ( 'NONE',  ( -65.00000337463102085, 60.62177826491077326, 12.50000000000000000 ) ) ;
#12801 = ORIENTED_EDGE ( 'NONE', *, *, #27757, .T. ) ;
#12802 = EDGE_CURVE ( 'NONE', #10592, #7368, #12578, .T. ) ;
#12803 = DIRECTION ( 'NONE',  ( 0.000000000000000000, 0.000000000000000000, 1.000000000000000000 ) ) ;
#12804 = DIRECTION ( 'NONE',  ( 0.000000000000000000, 0.000000000000000000, 1.000000000000000000 ) ) ;
#12805 = CYLINDRICAL_SURFACE ( 'NONE', #7606, 33.00000000000001421 ) ;
#12806 = DIRECTION ( 'NONE',  ( 0.000000000000000000, 0.000000000000000000, 1.000000000000000000 ) ) ;
#12807 = DIRECTION ( 'NONE',  ( 0.000000000000000000, 0.000000000000000000, 1.000000000000000000 ) ) ;
#12808 = AXIS2_PLACEMENT_3D ( 'NONE', #21595, #33395, #6956 ) ;
#12809 = EDGE_CURVE ( 'NONE', #26240, #17105, #18887, .T. ) ;
#12810 = CYLINDRICAL_SURFACE ( 'NONE', #10164, 2.000000000000001776 ) ;
#12811 = AXIS2_PLACEMENT_3D ( 'NONE', #7684, #18930, #22122 ) ;
#12812 = EDGE_CURVE ( 'NONE', #126, #17536, #22084, .T. ) ;
#12813 = CARTESIAN_POINT ( 'NONE',  ( 57.99999662536843914, -34.64101615137759893, -5.000000000000000000 ) ) ;
#12814 = VERTEX_POINT ( 'NONE', #13073 ) ;
#12815 = FACE_OUTER_BOUND ( 'NONE', #12045, .T. ) ;
#12816 = ADVANCED_FACE ( 'NONE', ( #10087 ), #35775, .F. ) ;
#12817 = CARTESIAN_POINT ( 'NONE',  ( -83.00000337463092137, -25.98076211353322051, 17.49999999999999645 ) ) ;
#12818 = DIRECTION ( 'NONE',  ( -0.000000000000000000, -0.000000000000000000, -1.000000000000000000 ) ) ;
#12819 = ORIENTED_EDGE ( 'NONE', *, *, #33451, .T. ) ;
#12820 = EDGE_LOOP ( 'NONE', ( #24492, #27044 ) ) ;
#12821 = EDGE_LOOP ( 'NONE', ( #34404, #7689 ) ) ;
#12822 = CARTESIAN_POINT ( 'NONE',  ( 19.99999662536858835, 69.28203230275516944, 12.50000000000000000 ) ) ;
#12823 = FACE_OUTER_BOUND ( 'NONE', #1268, .T. ) ;
#12824 = CYLINDRICAL_SURFACE ( 'NONE', #12446, 3.500000000000000888 ) ;
#12825 = CIRCLE ( 'NONE', #5079, 2.000000000000001776 ) ;
#12826 = EDGE_LOOP ( 'NONE', ( #8559, #26232, #28123, #28697, #15599, #9694, #4379, #14040, #27546, #1778, #28871, #26884 ) ) ;
#12827 = B_SPLINE_CURVE_WITH_KNOTS ( 'NONE', 3,
 ( #14322, #27813, #2689, #37018, #8337, #11323 ),
 .UNSPECIFIED., .F., .F.,
 ( 4, 2, 4 ),
 ( 0.004308305454211683143, 0.005784651566377464055, 0.007260997678543244099 ),
 .UNSPECIFIED. ) ;
#12828 = EDGE_CURVE ( 'NONE', #17978, #10472, #6015, .T. ) ;
#12829 = DIRECTION ( 'NONE',  ( 0.000000000000000000, 0.000000000000000000, 1.000000000000000000 ) ) ;
#12830 = EDGE_CURVE ( 'NONE', #27264, #20315, #24813, .T. ) ;
#12831 = CARTESIAN_POINT ( 'NONE',  ( 69.99999662536839651, -3.469446951953614189E-15, -9.999999999999998224 ) ) ;
#12832 = VERTEX_POINT ( 'NONE', #15527 ) ;
#12833 = CYLINDRICAL_SURFACE ( 'NONE', #21547, 2.000000000000001776 ) ;
#12834 = ORIENTED_EDGE ( 'NONE', *, *, #13082, .F. ) ;
#12835 = CARTESIAN_POINT ( 'NONE',  ( -106.7731239591675205, 98.28784258493143966, 32.50000000000000000 ) ) ;
#12836 = AXIS2_PLACEMENT_3D ( 'NONE', #8611, #20046, #20783 ) ;
#12837 = AXIS2_PLACEMENT_3D ( 'NONE', #4106, #26972, #1282 ) ;
#12838 = DIRECTION ( 'NONE',  ( 0.000000000000000000, 1.000000000000000000, -1.625241993126352989E-15 ) ) ;
#12839 = CARTESIAN_POINT ( 'NONE',  ( 86.99999662536831124, -8.660254037844397956, 17.49999999999999645 ) ) ;
#12840 = CIRCLE ( 'NONE', #3270, 2.000000000000000000 ) ;
#12841 = DIRECTION ( 'NONE',  ( 0.000000000000000000, 0.000000000000000000, -1.000000000000000000 ) ) ;
#12842 = VERTEX_POINT ( 'NONE', #26957 ) ;
#12843 = CARTESIAN_POINT ( 'NONE',  ( -20.00000000000001066, 89.94802294027088863, 27.49999999999999645 ) ) ;
#12844 = CONTEXT_DEPENDENT_SHAPE_REPRESENTATION ( #36746, #30144 ) ;
#12845 =( BOUNDED_CURVE ( )  B_SPLINE_CURVE ( 3, ( #6384, #6753, #18186, #29615 ),
 .UNSPECIFIED., .F., .F. ) 
 B_SPLINE_CURVE_WITH_KNOTS ( ( 4, 4 ),
 ( 1.570796326794896558, 3.141592653589793116 ),
 .UNSPECIFIED. ) 
 CURVE ( )  GEOMETRIC_REPRESENTATION_ITEM ( )  RATIONAL_B_SPLINE_CURVE ( ( 1.000000000000000000, 0.8047378541243649375, 0.8047378541243649375, 1.000000000000000000 ) ) 
 REPRESENTATION_ITEM ( '' )  );
#12846 = DIRECTION ( 'NONE',  ( 0.4999999999999919509, -0.8660254037844433705, 0.000000000000000000 ) ) ;
#12847 = ADVANCED_FACE ( 'NONE', ( #1267 ), #21320, .F. ) ;
#12848 = VECTOR ( 'NONE', #6569, 1000.000000000000000 ) ;
#12849 = DIRECTION ( 'NONE',  ( 1.000000000000000000, 0.000000000000000000, 0.000000000000000000 ) ) ;
#12850 = CARTESIAN_POINT ( 'NONE',  ( -13.00000337463125710, -77.94228634059960825, 17.49999999999999645 ) ) ;
#12851 = ORIENTED_EDGE ( 'NONE', *, *, #5571, .F. ) ;
#12852 = EDGE_CURVE ( 'NONE', #11966, #24803, #14838, .T. ) ;
#12853 = LINE ( 'NONE', #7255, #22598 ) ;
#12854 = CIRCLE ( 'NONE', #34449, 33.00000000000001421 ) ;
#12855 = CARTESIAN_POINT ( 'NONE',  ( 96.53048327204960799, 102.5304832720492527, 32.55002500000000509 ) ) ;
#12856 = DIRECTION ( 'NONE',  ( 0.000000000000000000, 0.000000000000000000, 1.000000000000000000 ) ) ;
#12857 = CIRCLE ( 'NONE', #27204, 2.000000000000001776 ) ;
#12858 = ORIENTED_EDGE ( 'NONE', *, *, #33538, .T. ) ;
#12859 = ORIENTED_EDGE ( 'NONE', *, *, #23789, .F. ) ;
#12860 = EDGE_CURVE ( 'NONE', #33375, #30431, #20219, .T. ) ;
#12861 = CARTESIAN_POINT ( 'NONE',  ( 69.99999662536838230, -34.64101615137759183, -9.999999999999998224 ) ) ;
#12862 = DIRECTION ( 'NONE',  ( 0.000000000000000000, 0.000000000000000000, 1.000000000000000000 ) ) ;
#12863 = AXIS2_PLACEMENT_3D ( 'NONE', #13446, #13651, #33899 ) ;
#12864 = AXIS2_PLACEMENT_3D ( 'NONE', #15249, #26688, #25957 ) ;
#12865 = DIRECTION ( 'NONE',  ( 0.000000000000000000, 0.000000000000000000, 1.000000000000000000 ) ) ;
#12866 = ORIENTED_EDGE ( 'NONE', *, *, #5059, .F. ) ;
#12867 = PLANE ( 'NONE',  #21192 ) ;
#12868 = PLANE ( 'NONE',  #1677 ) ;
#12869 = DIRECTION ( 'NONE',  ( -0.000000000000000000, -0.000000000000000000, 1.000000000000000000 ) ) ;
#12870 = CARTESIAN_POINT ( 'NONE',  ( -99.75152572807942875, 65.47112307816239252, 32.50000000000000000 ) ) ;
#12871 = ADVANCED_FACE ( 'NONE', ( #15887 ), #27316, .F. ) ;
#12872 = VERTEX_POINT ( 'NONE', #33126 ) ;
#12874 = VERTEX_POINT ( 'NONE', #5698 ) ;
#12873 = ADVANCED_FACE ( 'NONE', ( #7445 ), #11331, .F. ) ;
#12875 = DIRECTION ( 'NONE',  ( 1.000000000000000000, 0.000000000000000000, 0.000000000000000000 ) ) ;
#12876 = EDGE_CURVE ( 'NONE', #23345, #31169, #20668, .T. ) ;
#12877 = VECTOR ( 'NONE', #19605, 1000.000000000000000 ) ;
#12878 = DIRECTION ( 'NONE',  ( -1.000000000000000000, 0.000000000000000000, 0.000000000000000000 ) ) ;
#12880 = EDGE_CURVE ( 'NONE', #21760, #4105, #4656, .T. ) ;
#12879 = VERTEX_POINT ( 'NONE', #20321 ) ;
#12881 = AXIS2_PLACEMENT_3D ( 'NONE', #20469, #9611, #28905 ) ;
#12882 = DIRECTION ( 'NONE',  ( -0.000000000000000000, -0.000000000000000000, 1.000000000000000000 ) ) ;
#12883 = EDGE_LOOP ( 'NONE', ( #25287, #21103, #6555, #2708 ) ) ;
#12884 = DIRECTION ( 'NONE',  ( -1.000000000000000000, 0.000000000000000000, 0.000000000000000000 ) ) ;
#12885 = AXIS2_PLACEMENT_3D ( 'NONE', #4845, #22637, #36144 ) ;
#12886 = AXIS2_PLACEMENT_3D ( 'NONE', #3340, #3541, #332 ) ;
#12887 = CARTESIAN_POINT ( 'NONE',  ( -3.500000000000000888, 55.00000000000000000, 5.000000000000000888 ) ) ;
#12888 = ORIENTED_EDGE ( 'NONE', *, *, #32650, .T. ) ;
#12889 = EDGE_LOOP ( 'NONE', ( #1306, #28563 ) ) ;
#12890 = CARTESIAN_POINT ( 'NONE',  ( -60.00000337463104216, 51.96152422706639129, -5.000000000000000000 ) ) ;
#12891 = ORIENTED_EDGE ( 'NONE', *, *, #29672, .F. ) ;
#12892 = CIRCLE ( 'NONE', #16493, 2.000000000000001776 ) ;
#12893 = SHAPE_REPRESENTATION_RELATIONSHIP ( 'NONE' , 'NONE' ,  #35440, #30477 ) ;
#12894 = CIRCLE ( 'NONE', #22486, 2.000000000000001776 ) ;
#12895 = CARTESIAN_POINT ( 'NONE',  ( -52.39915983220772233, -35.19434990244957362, 12.49999999999999822 ) ) ;
#12896 = FACE_OUTER_BOUND ( 'NONE', #19963, .T. ) ;
#12897 = DIRECTION ( 'NONE',  ( 0.000000000000000000, -0.000000000000000000, 1.000000000000000000 ) ) ;
#12898 = ORIENTED_EDGE ( 'NONE', *, *, #33113, .T. ) ;
#12899 = FACE_OUTER_BOUND ( 'NONE', #11861, .T. ) ;
#12900 = DIRECTION ( 'NONE',  ( 0.000000000000000000, 0.000000000000000000, 1.000000000000000000 ) ) ;
#12901 = ORIENTED_EDGE ( 'NONE', *, *, #7768, .F. ) ;
#12902 = EDGE_CURVE ( 'NONE', #36225, #14998, #25612, .T. ) ;
#12903 = ORIENTED_EDGE ( 'NONE', *, *, #1192, .T. ) ;
#12904 = ORIENTED_EDGE ( 'NONE', *, *, #29292, .T. ) ;
#12906 = FACE_OUTER_BOUND ( 'NONE', #24816, .T. ) ;
#12905 = AXIS2_PLACEMENT_3D ( 'NONE', #12024, #17854, #18037 ) ;
#12907 = DIRECTION ( 'NONE',  ( 1.000000000000000000, 0.000000000000000000, 0.000000000000000000 ) ) ;
#12908 = EDGE_LOOP ( 'NONE', ( #5361, #15251, #12753, #33363, #1726, #30429 ) ) ;
#12909 = VECTOR ( 'NONE', #974, 1000.000000000000000 ) ;
#12910 = DIRECTION ( 'NONE',  ( -0.000000000000000000, -0.000000000000000000, 1.000000000000000000 ) ) ;
#12911 = AXIS2_PLACEMENT_3D ( 'NONE', #8969, #9321, #20761 ) ;
#12912 = CARTESIAN_POINT ( 'NONE',  ( 47.99999662536846756, 69.28203230275516944, -5.000000000000000000 ) ) ;
#12913 = AXIS2_PLACEMENT_3D ( 'NONE', #7699, #15947, #33385 ) ;
#12914 = EDGE_LOOP ( 'NONE', ( #33726, #6008 ) ) ;
#12915 = CIRCLE ( 'NONE', #9923, 2.000000000000001776 ) ;
#12916 = DIRECTION ( 'NONE',  ( 0.000000000000000000, 0.000000000000000000, 1.000000000000000000 ) ) ;
#12917 = AXIS2_PLACEMENT_3D ( 'NONE', #1646, #36336, #1835 ) ;
#12918 = DIRECTION ( 'NONE',  ( -1.000000000000000000, 0.000000000000000000, 0.000000000000000000 ) ) ;
#12919 = CARTESIAN_POINT ( 'NONE',  ( 31.02796211690949235, -59.29837256189548356, -49.86561046011506448 ) ) ;
#12920 = CARTESIAN_POINT ( 'NONE',  ( -3.000003374631308173, 77.94228634059957983, 17.49999999999999645 ) ) ;
#12921 = DIRECTION ( 'NONE',  ( 1.000000000000000000, 0.000000000000000000, 0.000000000000000000 ) ) ;
#12922 = CARTESIAN_POINT ( 'NONE',  ( -1.648146632869002426, -4.821944789745372439, -6.000000000000000000 ) ) ;
#12923 = VERTEX_POINT ( 'NONE', #9232 ) ;
#12924 = VERTEX_POINT ( 'NONE', #5899 ) ;
#12925 = LINE ( 'NONE', #4320, #3288 ) ;
#12926 = CARTESIAN_POINT ( 'NONE',  ( 34.99999662536855283, 60.62177826491078747, -5.000000000000000000 ) ) ;
#12927 = ADVANCED_FACE ( 'NONE', ( #34387 ), #3251, .F. ) ;
#12928 = CARTESIAN_POINT ( 'NONE',  ( -60.00000337463104216, 51.96152422706639129, -9.999999999999998224 ) ) ;
#12929 = DIRECTION ( 'NONE',  ( 0.000000000000000000, 0.000000000000000000, -1.000000000000000000 ) ) ;
#12930 = ORIENTED_EDGE ( 'NONE', *, *, #21090, .F. ) ;
#12931 = AXIS2_PLACEMENT_3D ( 'NONE', #23351, #34790, #6648 ) ;
#12932 = DIRECTION ( 'NONE',  ( 1.000000000000000000, 0.000000000000000000, 0.000000000000000000 ) ) ;
#12933 = CARTESIAN_POINT ( 'NONE',  ( 64.99999662536839651, 60.62177826491078747, -5.000000000000000000 ) ) ;
#12934 = CIRCLE ( 'NONE', #14144, 3.499999999999996003 ) ;
#12935 = ORIENTED_EDGE ( 'NONE', *, *, #18683, .T. ) ;
#12936 =( GEOMETRIC_REPRESENTATION_CONTEXT ( 3 ) GLOBAL_UNCERTAINTY_ASSIGNED_CONTEXT ( ( #28668 ) ) GLOBAL_UNIT_ASSIGNED_CONTEXT ( ( #25495, #5613, #11589 ) ) REPRESENTATION_CONTEXT ( 'NONE', 'WORKASPACE' ) );
#12937 = CARTESIAN_POINT ( 'NONE',  ( 91.99999662536828282, 0.000000000000000000, -9.999999999999998224 ) ) ;
#12938 = ORIENTED_EDGE ( 'NONE', *, *, #14475, .F. ) ;
#12939 = AXIS2_PLACEMENT_3D ( 'NONE', #2347, #13583, #17329 ) ;
#12940 = AXIS2_PLACEMENT_3D ( 'NONE', #876, #6319, #12107 ) ;
#12941 = CARTESIAN_POINT ( 'NONE',  ( 27.78182860042856461, 56.67878100130339902, 12.49999999999999822 ) ) ;
#12942 = VECTOR ( 'NONE', #36818, 1000.000000000000000 ) ;
#12943 = CARTESIAN_POINT ( 'NONE',  ( -62.00000337463104927, 51.96152422706639129, 12.50000000000000000 ) ) ;
#12944 = AXIS2_PLACEMENT_3D ( 'NONE', #7669, #36357, #10668 ) ;
#12945 = DIRECTION ( 'NONE',  ( 1.000000000000000000, 0.000000000000000000, 0.000000000000000000 ) ) ;
#12946 = ORIENTED_EDGE ( 'NONE', *, *, #33435, .F. ) ;
#12947 = ORIENTED_EDGE ( 'NONE', *, *, #23510, .T. ) ;
#12948 = EDGE_CURVE ( 'NONE', #3254, #6819, #13087, .T. ) ;
#12949 = CIRCLE ( 'NONE', #1585, 27.00000000000001421 ) ;
#12950 = VERTEX_POINT ( 'NONE', #5004 ) ;
#12951 = DIRECTION ( 'NONE',  ( 0.000000000000000000, 0.000000000000000000, -1.000000000000000000 ) ) ;
#12952 = DIRECTION ( 'NONE',  ( 0.000000000000000000, 0.000000000000000000, 1.000000000000000000 ) ) ;
#12953 = ADVANCED_FACE ( 'NONE', ( #25945 ), #8883, .T. ) ;
#12954 = DIRECTION ( 'NONE',  ( 0.000000000000000000, 0.000000000000000000, 1.000000000000000000 ) ) ;
#12955 = LINE ( 'NONE', #18609, #28292 ) ;
#12956 = CARTESIAN_POINT ( 'NONE',  ( -31.74999999999995737, 0.000000000000000000, 0.000000000000000000 ) ) ;
#12957 = ORIENTED_EDGE ( 'NONE', *, *, #4655, .T. ) ;
#12958 = CARTESIAN_POINT ( 'NONE',  ( -82.00000337463096400, -34.64101615137762025, 12.50000000000000000 ) ) ;
#12959 = AXIS2_PLACEMENT_3D ( 'NONE', #29454, #3420, #9409 ) ;
#12960 = CARTESIAN_POINT ( 'NONE',  ( -5.000000000000000000, -2.886751345948133540, -6.000000000000000000 ) ) ;
#12961 = EDGE_CURVE ( 'NONE', #25364, #30431, #27393, .T. ) ;
#12962 = AXIS2_PLACEMENT_3D ( 'NONE', #28956, #22289, #11025 ) ;
#12963 = LINE ( 'NONE', #27412, #10418 ) ;
#12964 = VERTEX_POINT ( 'NONE', #25092 ) ;
#12965 = CARTESIAN_POINT ( 'NONE',  ( 64.99999662536842493, 43.30127018922200222, -9.999999999999998224 ) ) ;
#12966 = PRODUCT_DEFINITION_FORMATION_WITH_SPECIFIED_SOURCE ( 'ANY', '', #20242, .NOT_KNOWN. ) ;
#12967 = DIRECTION ( 'NONE',  ( 0.000000000000000000, 0.000000000000000000, 1.000000000000000000 ) ) ;
#12968 = CIRCLE ( 'NONE', #21948, 2.000000000000000000 ) ;
#12969 = ORIENTED_EDGE ( 'NONE', *, *, #30072, .F. ) ;
#12970 = CIRCLE ( 'NONE', #18960, 3.000000000000006217 ) ;
#12971 = EDGE_LOOP ( 'NONE', ( #35830, #29548, #27182, #5174 ) ) ;
#12972 = CIRCLE ( 'NONE', #2199, 2.000000000000000000 ) ;
#12973 = DIRECTION ( 'NONE',  ( 0.000000000000000000, 0.000000000000000000, -1.000000000000000000 ) ) ;
#12974 = EDGE_CURVE ( 'NONE', #21666, #27114, #5271, .T. ) ;
#12975 = DIRECTION ( 'NONE',  ( -1.000000000000000000, -0.000000000000000000, -0.000000000000000000 ) ) ;
#12976 = CARTESIAN_POINT ( 'NONE',  ( 31.99999662536856704, 69.28203230275518365, -9.999999999999998224 ) ) ;
#12977 = VERTEX_POINT ( 'NONE', #26320 ) ;
#12978 = ORIENTED_EDGE ( 'NONE', *, *, #10501, .F. ) ;
#12979 = ORIENTED_EDGE ( 'NONE', *, *, #27891, .T. ) ;
#12980 = CIRCLE ( 'NONE', #22574, 3.000000000000002665 ) ;
#12981 = DIRECTION ( 'NONE',  ( -0.000000000000000000, -0.000000000000000000, 1.000000000000000000 ) ) ;
#12982 = ORIENTED_EDGE ( 'NONE', *, *, #11486, .F. ) ;
#12983 = ORIENTED_EDGE ( 'NONE', *, *, #6192, .F. ) ;
#12984 = FACE_BOUND ( 'NONE', #20414, .T. ) ;
#12985 = ORIENTED_EDGE ( 'NONE', *, *, #8603, .F. ) ;
#12986 = AXIS2_PLACEMENT_3D ( 'NONE', #7641, #27513, #35773 ) ;
#12987 = AXIS2_PLACEMENT_3D ( 'NONE', #7715, #8078, #36210 ) ;
#12988 = ORIENTED_EDGE ( 'NONE', *, *, #27860, .T. ) ;
#12989 = DIRECTION ( 'NONE',  ( 0.000000000000000000, 0.000000000000000000, -1.000000000000000000 ) ) ;
#12990 = CIRCLE ( 'NONE', #32151, 3.000000000000000000 ) ;
#12991 = CIRCLE ( 'NONE', #16596, 3.500000000000003109 ) ;
#12992 = EDGE_CURVE ( 'NONE', #15625, #5415, #14879, .T. ) ;
#12993 = CARTESIAN_POINT ( 'NONE',  ( 19.99999662536861678, -69.28203230275519786, 17.49999999999999645 ) ) ;
#12994 = ORIENTED_EDGE ( 'NONE', *, *, #5235, .T. ) ;
#12995 = ORIENTED_EDGE ( 'NONE', *, *, #11886, .F. ) ;
#12996 = CYLINDRICAL_SURFACE ( 'NONE', #27505, 2.000000000000001776 ) ;
#12997 = CARTESIAN_POINT ( 'NONE',  ( -65.00000337463102085, 60.62177826491077326, 17.49999999999999645 ) ) ;
#12998 = AXIS2_PLACEMENT_3D ( 'NONE', #22047, #33666, #28217 ) ;
#12999 = VECTOR ( 'NONE', #34516, 1000.000000000000000 ) ;
#13000 = CARTESIAN_POINT ( 'NONE',  ( -80.00000337463096400, -34.64101615137762025, 12.50000000000000000 ) ) ;
#13001 = CARTESIAN_POINT ( 'NONE',  ( 32.99999662536853862, 77.94228634059959404, -9.999999999999998224 ) ) ;
#13002 = CIRCLE ( 'NONE', #16017, 2.000000000000001776 ) ;
#13003 = EDGE_LOOP ( 'NONE', ( #21203, #937, #11332, #36995 ) ) ;
#13004 = CARTESIAN_POINT ( 'NONE',  ( -70.00000337463099243, 17.32050807568877460, -9.999999999999998224 ) ) ;
#13005 = VERTEX_POINT ( 'NONE', #27866 ) ;
#13006 = CARTESIAN_POINT ( 'NONE',  ( -10.00000337463128197, 86.60254037844397601, -9.999999999999998224 ) ) ;
#13007 = EDGE_CURVE ( 'NONE', #11624, #23282, #28594, .T. ) ;
#13008 = DIRECTION ( 'NONE',  ( 0.000000000000000000, 0.000000000000000000, -1.000000000000000000 ) ) ;
#13009 = CARTESIAN_POINT ( 'NONE',  ( 4.999996625368676284, -77.94228634059960825, -5.000000000000000000 ) ) ;
#13010 = CIRCLE ( 'NONE', #29783, 30.00000000000000000 ) ;
#13011 = DIRECTION ( 'NONE',  ( -0.7650473262243666639, 0.6439740589782693148, -0.000000000000000000 ) ) ;
#13012 = DIRECTION ( 'NONE',  ( 0.000000000000000000, -0.000000000000000000, 1.000000000000000000 ) ) ;
#13013 = DIRECTION ( 'NONE',  ( -0.5000000000000098810, -0.8660254037844328234, 0.000000000000000000 ) ) ;
#13014 = EDGE_CURVE ( 'NONE', #2540, #11374, #8515, .T. ) ;
#13015 = AXIS2_PLACEMENT_3D ( 'NONE', #15433, #6436, #1356 ) ;
#13016 = CARTESIAN_POINT ( 'NONE',  ( -66.50936994187880202, 41.98909163213660634, -5.000000000000000000 ) ) ;
#13017 = ORIENTED_EDGE ( 'NONE', *, *, #15156, .F. ) ;
#13018 = DIRECTION ( 'NONE',  ( 1.000000000000000000, 0.000000000000000000, 0.000000000000000000 ) ) ;
#13019 = AXIS2_PLACEMENT_3D ( 'NONE', #9821, #12448, #32896 ) ;
#13020 = DIRECTION ( 'NONE',  ( 0.000000000000000000, 0.4999999999999991118, -0.8660254037844391517 ) ) ;
#13021 = LINE ( 'NONE', #27640, #9752 ) ;
#13022 = CIRCLE ( 'NONE', #4064, 2.000000000000001776 ) ;
#13023 = VERTEX_POINT ( 'NONE', #31905 ) ;
#13024 = ORIENTED_EDGE ( 'NONE', *, *, #26092, .F. ) ;
#13025 = VERTEX_POINT ( 'NONE', #31370 ) ;
#13026 = CIRCLE ( 'NONE', #9446, 33.00000000000001421 ) ;
#13027 = CARTESIAN_POINT ( 'NONE',  ( 51.13139720814399425, -27.50000000000022737, -10.00000000000000178 ) ) ;
#13028 = DIRECTION ( 'NONE',  ( 1.000000000000000000, 0.000000000000000000, 0.000000000000000000 ) ) ;
#13029 = ORIENTED_EDGE ( 'NONE', *, *, #20590, .T. ) ;
#13030 = VECTOR ( 'NONE', #24746, 1000.000000000000000 ) ;
#13031 = CIRCLE ( 'NONE', #34011, 2.000000000000001776 ) ;
#13032 = DIRECTION ( 'NONE',  ( 1.000000000000000000, 0.000000000000000000, 0.000000000000000000 ) ) ;
#13033 = ADVANCED_FACE ( 'NONE', ( #17139 ), #20483, .F. ) ;
#13034 = CARTESIAN_POINT ( 'NONE',  ( 5.999999999999947597, -2.132877728683645235E-15, 32.50000000000000000 ) ) ;
#13035 = VERTEX_POINT ( 'NONE', #14507 ) ;
#13036 = DIRECTION ( 'NONE',  ( 0.000000000000000000, 0.000000000000000000, 1.000000000000000000 ) ) ;
#13037 = ORIENTED_EDGE ( 'NONE', *, *, #35053, .F. ) ;
#13038 = DIRECTION ( 'NONE',  ( 0.000000000000000000, 0.000000000000000000, 1.000000000000000000 ) ) ;
#13039 = CIRCLE ( 'NONE', #34017, 27.00000000000001776 ) ;
#13040 = EDGE_CURVE ( 'NONE', #11692, #14483, #34607, .T. ) ;
#13041 = DIRECTION ( 'NONE',  ( 1.000000000000000000, 0.000000000000000000, 0.000000000000000000 ) ) ;
#13042 = DIRECTION ( 'NONE',  ( -0.7071067811865439090, 0.7071067811865512365, 0.000000000000000000 ) ) ;
#13043 = CIRCLE ( 'NONE', #6432, 65.00000000000000000 ) ;
#13044 = EDGE_CURVE ( 'NONE', #14998, #36225, #8263, .T. ) ;
#13045 = SURFACE_SIDE_STYLE ('',( #35749 ) ) ;
#13046 = EDGE_LOOP ( 'NONE', ( #8660, #16285, #28530, #5062 ) ) ;
#13047 = DIRECTION ( 'NONE',  ( 1.000000000000000000, 0.000000000000000000, 0.000000000000000000 ) ) ;
#13048 = CIRCLE ( 'NONE', #34612, 2.000000000000001776 ) ;
#13049 = AXIS2_PLACEMENT_3D ( 'NONE', #2073, #7524, #4907 ) ;
#13050 = CIRCLE ( 'NONE', #25650, 2.000000000000001776 ) ;
#13051 = DIRECTION ( 'NONE',  ( 0.000000000000000000, 0.000000000000000000, 1.000000000000000000 ) ) ;
#13052 = FACE_OUTER_BOUND ( 'NONE', #27825, .T. ) ;
#13053 = VECTOR ( 'NONE', #24218, 1000.000000000000000 ) ;
#13054 = CARTESIAN_POINT ( 'NONE',  ( 81.99999662536833966, -3.469446951953614189E-15, -9.999999999999998224 ) ) ;
#13055 = DIRECTION ( 'NONE',  ( 0.000000000000000000, 0.000000000000000000, 1.000000000000000000 ) ) ;
#13056 = ORIENTED_EDGE ( 'NONE', *, *, #23273, .T. ) ;
#13057 = DIRECTION ( 'NONE',  ( 0.000000000000000000, 0.000000000000000000, -1.000000000000000000 ) ) ;
#13058 = CARTESIAN_POINT ( 'NONE',  ( 74.99999662536835388, -25.98076211353319565, -9.999999999999998224 ) ) ;
#13059 = DIRECTION ( 'NONE',  ( 0.000000000000000000, 0.000000000000000000, 1.000000000000000000 ) ) ;
#13060 = VERTEX_POINT ( 'NONE', #21228 ) ;
#13061 = EDGE_CURVE ( 'NONE', #5447, #21544, #29198, .T. ) ;
#13062 = ORIENTED_EDGE ( 'NONE', *, *, #13007, .T. ) ;
#13063 = CYLINDRICAL_SURFACE ( 'NONE', #31539, 2.000000000000001776 ) ;
#13064 = AXIS2_PLACEMENT_3D ( 'NONE', #19839, #16846, #22840 ) ;
#13065 = DIRECTION ( 'NONE',  ( 0.000000000000000000, 0.000000000000000000, 1.000000000000000000 ) ) ;
#13066 = CARTESIAN_POINT ( 'NONE',  ( -108.3061974404900241, -19.22934205794863516, 32.50000000000000000 ) ) ;
#13067 = ORIENTED_EDGE ( 'NONE', *, *, #8140, .F. ) ;
#13068 = CIRCLE ( 'NONE', #8298, 2.000000000000001776 ) ;
#13069 = CARTESIAN_POINT ( 'NONE',  ( 149.8799519615616589, 5.999999999999476863, 32.50000000000000000 ) ) ;
#13070 = DIRECTION ( 'NONE',  ( 0.000000000000000000, 0.000000000000000000, -1.000000000000000000 ) ) ;
#13071 = CIRCLE ( 'NONE', #13668, 2.000000000000001776 ) ;
#13072 = DIRECTION ( 'NONE',  ( 1.000000000000000000, 0.000000000000000000, 0.000000000000000000 ) ) ;
#13073 = CARTESIAN_POINT ( 'NONE',  ( 77.99999662536833966, 17.32050807568879236, -5.000000000000000000 ) ) ;
#13074 = ORIENTED_EDGE ( 'NONE', *, *, #6106, .F. ) ;
#13075 = CIRCLE ( 'NONE', #19669, 2.000000000000001776 ) ;
#13076 = ORIENTED_EDGE ( 'NONE', *, *, #3782, .T. ) ;
#13077 = DIRECTION ( 'NONE',  ( 1.000000000000000000, 0.000000000000000000, 0.000000000000000000 ) ) ;
#13078 = ADVANCED_FACE ( 'NONE', ( #24433 ), #35502, .F. ) ;
#13079 = AXIS2_PLACEMENT_3D ( 'NONE', #27365, #9930, #33167 ) ;
#13080 = DIRECTION ( 'NONE',  ( 0.000000000000000000, 0.000000000000000000, -1.000000000000000000 ) ) ;
#13081 = EDGE_LOOP ( 'NONE', ( #35062, #31290 ) ) ;
#13082 = EDGE_CURVE ( 'NONE', #28140, #24230, #23216, .T. ) ;
#13083 = CARTESIAN_POINT ( 'NONE',  ( -0.6806757771963263259, -5.380514348701145089, -3.838711833383647853 ) ) ;
#13084 = ORIENTED_EDGE ( 'NONE', *, *, #732, .T. ) ;
#13085 = CARTESIAN_POINT ( 'NONE',  ( -75.00000337463097821, 8.660254037844374864, -9.999999999999998224 ) ) ;
#13086 = AXIS2_PLACEMENT_3D ( 'NONE', #20079, #5480, #19901 ) ;
#13087 =( BOUNDED_CURVE ( )  B_SPLINE_CURVE ( 3, ( #17332, #74, #2193, #31742 ),
 .UNSPECIFIED., .F., .F. ) 
 B_SPLINE_CURVE_WITH_KNOTS ( ( 4, 4 ),
 ( 1.570796326794896558, 3.141592653589793116 ),
 .UNSPECIFIED. ) 
 CURVE ( )  GEOMETRIC_REPRESENTATION_ITEM ( )  RATIONAL_B_SPLINE_CURVE ( ( 1.000000000000000000, 0.8047378541243649375, 0.8047378541243649375, 1.000000000000000000 ) ) 
 REPRESENTATION_ITEM ( '' )  );
#13088 = EDGE_CURVE ( 'NONE', #24516, #14569, #22605, .T. ) ;
#13089 = AXIS2_PLACEMENT_3D ( 'NONE', #820, #12232, #20898 ) ;
#13090 = CARTESIAN_POINT ( 'NONE',  ( -77.00000337463100664, -43.30127018922202353, 12.50000000000000000 ) ) ;
#13091 = ORIENTED_EDGE ( 'NONE', *, *, #19334, .T. ) ;
#13092 = EDGE_CURVE ( 'NONE', #13968, #27821, #12776, .T. ) ;
#13093 = CARTESIAN_POINT ( 'NONE',  ( 35.99999999999999289, 3.334407072378457159E-16, -2.445500000000000007 ) ) ;
#13094 = ORIENTED_EDGE ( 'NONE', *, *, #16661, .T. ) ;
#13095 = EDGE_CURVE ( 'NONE', #34413, #3514, #24228, .T. ) ;
#13096 = FILL_AREA_STYLE ('',( #36155 ) ) ;
#13097 = PRODUCT_DEFINITION_SHAPE ( 'NONE', 'NONE',  #37124 ) ;
#13098 = FACE_OUTER_BOUND ( 'NONE', #11745, .T. ) ;
#13099 = AXIS2_PLACEMENT_3D ( 'NONE', #10323, #24202, #1155 ) ;
#13100 = CARTESIAN_POINT ( 'NONE',  ( 81.99999662536833966, 17.32050807568879236, -5.000000000000000000 ) ) ;
#13101 = DIRECTION ( 'NONE',  ( 0.8660254037844413721, 0.4999999999999950595, 0.000000000000000000 ) ) ;
#13102 = EDGE_LOOP ( 'NONE', ( #3732, #15535, #19998, #33957 ) ) ;
#13103 = DIRECTION ( 'NONE',  ( 0.000000000000000000, 0.000000000000000000, -1.000000000000000000 ) ) ;
#13104 = CARTESIAN_POINT ( 'NONE',  ( -107.2777746127022453, 46.05181527023793819, 32.50000000000000711 ) ) ;
#13105 = LINE ( 'NONE', #1669, #21326 ) ;
#13106 = EDGE_CURVE ( 'NONE', #14689, #4744, #13043, .T. ) ;
#13107 = EDGE_LOOP ( 'NONE', ( #29517, #24362 ) ) ;
#13108 = ADVANCED_FACE ( 'NONE', ( #18628 ), #35331, .F. ) ;
#13109 = EDGE_LOOP ( 'NONE', ( #23864, #17598, #22813, #3568 ) ) ;
#13110 = ORIENTED_EDGE ( 'NONE', *, *, #31522, .F. ) ;
#13111 = EDGE_CURVE ( 'NONE', #29187, #14423, #1053, .T. ) ;
#13112 = DIRECTION ( 'NONE',  ( -1.000000000000000000, 0.000000000000000000, 0.000000000000000000 ) ) ;
#13113 = ADVANCED_FACE ( 'NONE', ( #29657 ), #27041, .F. ) ;
#13114 = CIRCLE ( 'NONE', #33493, 2.000000000000001776 ) ;
#13115 = DIRECTION ( 'NONE',  ( 0.000000000000000000, 0.000000000000000000, -1.000000000000000000 ) ) ;
#13116 = VERTEX_POINT ( 'NONE', #35679 ) ;
#13117 = CARTESIAN_POINT ( 'NONE',  ( 0.000000000000000000, -55.00000000000000000, -10.00000000000000178 ) ) ;
#13118 = CARTESIAN_POINT ( 'NONE',  ( -32.00000337463119848, -69.28203230275522628, -9.999999999999998224 ) ) ;
#13119 = AXIS2_PLACEMENT_3D ( 'NONE', #23033, #11236, #22684 ) ;
#13120 = DIRECTION ( 'NONE',  ( 1.000000000000000000, 0.000000000000000000, 0.000000000000000000 ) ) ;
#13121 = CYLINDRICAL_SURFACE ( 'NONE', #53, 2.000000000000001776 ) ;
#13122 = AXIS2_PLACEMENT_3D ( 'NONE', #25653, #25276, #5760 ) ;
#13123 = DIRECTION ( 'NONE',  ( -1.000000000000000000, 1.798972493605577187E-15, 0.000000000000000000 ) ) ;
#13124 = AXIS2_PLACEMENT_3D ( 'NONE', #9268, #31937, #6479 ) ;
#13125 = CARTESIAN_POINT ( 'NONE',  ( 79.99999662536833966, 17.32050807568879236, -9.999999999999998224 ) ) ;
#13126 = DIRECTION ( 'NONE',  ( -0.000000000000000000, -0.000000000000000000, 1.000000000000000000 ) ) ;
#13127 = FACE_OUTER_BOUND ( 'NONE', #29253, .T. ) ;
#13128 = ORIENTED_EDGE ( 'NONE', *, *, #26345, .F. ) ;
#13129 = ORIENTED_EDGE ( 'NONE', *, *, #25447, .T. ) ;
#13130 = CARTESIAN_POINT ( 'NONE',  ( 0.000000000000000000, 0.000000000000000000, 27.50000000000000000 ) ) ;
#13131 = CIRCLE ( 'NONE', #20299, 2.000000000000001776 ) ;
#13132 = CARTESIAN_POINT ( 'NONE',  ( -68.00000337463099243, 17.32050807568877460, 17.49999999999999645 ) ) ;
#13133 = CARTESIAN_POINT ( 'NONE',  ( 19.99999662536857770, 86.60254037844397601, -5.000000000000000000 ) ) ;
#13134 = DIRECTION ( 'NONE',  ( 0.000000000000000000, 0.000000000000000000, 1.000000000000000000 ) ) ;
#13135 = ORIENTED_EDGE ( 'NONE', *, *, #22868, .T. ) ;
#13136 = CIRCLE ( 'NONE', #4769, 8.500000000000007105 ) ;
#13137 = DIRECTION ( 'NONE',  ( 0.000000000000000000, 0.000000000000000000, 1.000000000000000000 ) ) ;
#13138 = DIRECTION ( 'NONE',  ( -1.000000000000000000, 0.000000000000000000, 0.000000000000000000 ) ) ;
#13139 = FACE_OUTER_BOUND ( 'NONE', #34678, .T. ) ;
#13140 = ORIENTED_EDGE ( 'NONE', *, *, #30948, .T. ) ;
#13141 = FACE_OUTER_BOUND ( 'NONE', #13263, .T. ) ;
#13142 = ORIENTED_EDGE ( 'NONE', *, *, #16907, .T. ) ;
#13143 = CIRCLE ( 'NONE', #35909, 2.000000000000001776 ) ;
#13144 = DIRECTION ( 'NONE',  ( 1.000000000000000000, 0.000000000000000000, 0.000000000000000000 ) ) ;
#13145 = CARTESIAN_POINT ( 'NONE',  ( 3.000000000000000000, 2.935248768560057453, -3.903127820947815962E-15 ) ) ;
#13146 = AXIS2_PLACEMENT_3D ( 'NONE', #28804, #24116, #23553 ) ;
#13147 = DIRECTION ( 'NONE',  ( 0.000000000000000000, 0.000000000000000000, -1.000000000000000000 ) ) ;
#13148 = ORIENTED_EDGE ( 'NONE', *, *, #11989, .T. ) ;
#13149 = AXIS2_PLACEMENT_3D ( 'NONE', #10023, #30073, #4398 ) ;
#13150 = VERTEX_POINT ( 'NONE', #12976 ) ;
#13151 = DIRECTION ( 'NONE',  ( 0.000000000000000000, 0.000000000000000000, 1.000000000000000000 ) ) ;
#13152 = VERTEX_POINT ( 'NONE', #9984 ) ;
#13153 = DIRECTION ( 'NONE',  ( 1.000000000000000000, 0.000000000000000000, 0.000000000000000000 ) ) ;
#13154 = AXIS2_PLACEMENT_3D ( 'NONE', #29542, #15869, #26554 ) ;
#13155 = EDGE_CURVE ( 'NONE', #14823, #32711, #36983, .T. ) ;
#13156 = FACE_BOUND ( 'NONE', #25727, .T. ) ;
#13157 = AXIS2_PLACEMENT_3D ( 'NONE', #25834, #8020, #28088 ) ;
#13158 = DIRECTION ( 'NONE',  ( -1.000000000000000000, 0.000000000000000000, 0.000000000000000000 ) ) ;
#13159 = CARTESIAN_POINT ( 'NONE',  ( 29.99999662536856349, 69.28203230275518365, 12.50000000000000000 ) ) ;
#13160 = CARTESIAN_POINT ( 'NONE',  ( 16.99999662536859901, 77.94228634059957983, -9.999999999999998224 ) ) ;
#13161 = EDGE_LOOP ( 'NONE', ( #31661, #34069 ) ) ;
#13162 = CARTESIAN_POINT ( 'NONE',  ( -77.93343913441597692, 72.12058696850911588, 27.50000000000000000 ) ) ;
#13163 = CARTESIAN_POINT ( 'NONE',  ( 56.99999662536844625, 60.62177826491077326, -9.999999999999998224 ) ) ;
#13164 = FACE_OUTER_BOUND ( 'NONE', #22283, .T. ) ;
#13165 = VERTEX_POINT ( 'NONE', #17877 ) ;
#13166 = CARTESIAN_POINT ( 'NONE',  ( 84.99999662536831124, -8.660254037844397956, 12.50000000000000000 ) ) ;
#13167 = LINE ( 'NONE', #24621, #32123 ) ;
#13168 = VECTOR ( 'NONE', #1795, 1000.000000000000000 ) ;
#13169 = ORIENTED_EDGE ( 'NONE', *, *, #12086, .F. ) ;
#13170 = ORIENTED_EDGE ( 'NONE', *, *, #1479, .F. ) ;
#13171 = VECTOR ( 'NONE', #36231, 1000.000000000000000 ) ;
#13172 = DIRECTION ( 'NONE',  ( 1.000000000000000000, 0.000000000000000000, 0.000000000000000000 ) ) ;
#13173 =( GEOMETRIC_REPRESENTATION_CONTEXT ( 3 ) GLOBAL_UNCERTAINTY_ASSIGNED_CONTEXT ( ( #36927 ) ) GLOBAL_UNIT_ASSIGNED_CONTEXT ( ( #25929, #17859, #34755 ) ) REPRESENTATION_CONTEXT ( 'NONE', 'WORKASPACE' ) );
#13174 = CARTESIAN_POINT ( 'NONE',  ( -44.13139720814437794, -27.49999999999955591, -15.00000000000000000 ) ) ;
#13175 = CARTESIAN_POINT ( 'NONE',  ( -104.3563124639471908, -35.61515136444246821, 32.49999999999999289 ) ) ;
#13176 = ORIENTED_EDGE ( 'NONE', *, *, #1079, .F. ) ;
#13177 = ORIENTED_EDGE ( 'NONE', *, *, #11404, .T. ) ;
#13178 = AXIS2_PLACEMENT_3D ( 'NONE', #969, #26652, #12388 ) ;
#13179 = VERTEX_POINT ( 'NONE', #29306 ) ;
#13180 = EDGE_CURVE ( 'NONE', #27228, #3559, #9437, .T. ) ;
#13181 = EDGE_CURVE ( 'NONE', #20872, #31806, #30387, .T. ) ;
#13182 = CARTESIAN_POINT ( 'NONE',  ( 47.63139720814418610, 27.49999999999988987, 5.000000000000000888 ) ) ;
#13183 = ORIENTED_EDGE ( 'NONE', *, *, #16539, .F. ) ;
#13184 = CIRCLE ( 'NONE', #13782, 5.000000000000000888 ) ;
#13185 = LINE ( 'NONE', #30430, #20190 ) ;
#13186 = VERTEX_POINT ( 'NONE', #32478 ) ;
#13187 = ORIENTED_EDGE ( 'NONE', *, *, #21206, .F. ) ;
#13188 = EDGE_CURVE ( 'NONE', #30738, #8351, #36400, .T. ) ;
#13189 = CARTESIAN_POINT ( 'NONE',  ( 59.99999662536843914, -34.64101615137759893, -9.999999999999998224 ) ) ;
#13190 = CARTESIAN_POINT ( 'NONE',  ( -73.00000337463100664, -43.30127018922202353, -9.999999999999998224 ) ) ;
#13191 = ORIENTED_EDGE ( 'NONE', *, *, #17832, .T. ) ;
#13192 = AXIS2_PLACEMENT_3D ( 'NONE', #37019, #25938, #23316 ) ;
#13193 = ORIENTED_EDGE ( 'NONE', *, *, #32232, .F. ) ;
#13194 = CARTESIAN_POINT ( 'NONE',  ( -75.00000337463100664, -43.30127018922202353, -9.999999999999998224 ) ) ;
#13195 = DIRECTION ( 'NONE',  ( 1.000000000000000000, 0.000000000000000000, 0.000000000000000000 ) ) ;
#13196 = CARTESIAN_POINT ( 'NONE',  ( -75.00000337463097821, 43.30127018922197379, -9.999999999999998224 ) ) ;
#13197 = FACE_OUTER_BOUND ( 'NONE', #16220, .T. ) ;
#13198 = ORIENTED_EDGE ( 'NONE', *, *, #23377, .T. ) ;
#13199 = CARTESIAN_POINT ( 'NONE',  ( 42.99999662536848888, -77.94228634059960825, -5.000000000000000000 ) ) ;
#13200 = ORIENTED_EDGE ( 'NONE', *, *, #2945, .T. ) ;
#13201 = VECTOR ( 'NONE', #17811, 1000.000000000000000 ) ;
#13202 = EDGE_CURVE ( 'NONE', #26731, #23730, #3780, .T. ) ;
#13203 = CARTESIAN_POINT ( 'NONE',  ( 47.63139720814400846, -27.50000000000022737, -5.000000000000000888 ) ) ;
#13204 = DIRECTION ( 'NONE',  ( 1.000000000000000000, 0.000000000000000000, 0.000000000000000000 ) ) ;
#13205 = AXIS2_PLACEMENT_3D ( 'NONE', #12713, #27156, #12907 ) ;
#13206 = DIRECTION ( 'NONE',  ( 1.000000000000000000, 0.000000000000000000, 0.000000000000000000 ) ) ;
#13207 = CYLINDRICAL_SURFACE ( 'NONE', #23704, 2.000000000000001776 ) ;
#13208 = DIRECTION ( 'NONE',  ( 0.000000000000000000, 0.000000000000000000, 1.000000000000000000 ) ) ;
#13209 = CARTESIAN_POINT ( 'NONE',  ( 86.45172111230354517, -31.46585318596159553, -4.999999999999997335 ) ) ;
#13210 = DIRECTION ( 'NONE',  ( 1.000000000000000000, 0.000000000000000000, 0.000000000000000000 ) ) ;
#13211 = VERTEX_POINT ( 'NONE', #22177 ) ;
#13212 = CARTESIAN_POINT ( 'NONE',  ( -45.00000337463112743, -60.62177826491080168, 17.49999999999999645 ) ) ;
#13213 = DIRECTION ( 'NONE',  ( 0.000000000000000000, 0.000000000000000000, -1.000000000000000000 ) ) ;
#13214 = DIRECTION ( 'NONE',  ( 0.000000000000000000, 0.000000000000000000, 1.000000000000000000 ) ) ;
#13215 = ORIENTED_EDGE ( 'NONE', *, *, #5423, .T. ) ;
#13216 = ORIENTED_EDGE ( 'NONE', *, *, #19835, .T. ) ;
#13217 = ORIENTED_EDGE ( 'NONE', *, *, #25143, .F. ) ;
#13218 = ADVANCED_FACE ( 'NONE', ( #33616 ), #4750, .T. ) ;
#13219 = DIRECTION ( 'NONE',  ( 0.000000000000000000, 0.000000000000000000, 1.000000000000000000 ) ) ;
#13220 = CARTESIAN_POINT ( 'NONE',  ( -3.374631327851540519E-06, 86.60254037844397601, -9.999999999999998224 ) ) ;
#13221 = VERTEX_POINT ( 'NONE', #4551 ) ;
#13222 = EDGE_CURVE ( 'NONE', #16872, #8805, #27029, .T. ) ;
#13223 = DIRECTION ( 'NONE',  ( 0.000000000000000000, 0.000000000000000000, 1.000000000000000000 ) ) ;
#13224 = FACE_OUTER_BOUND ( 'NONE', #17742, .T. ) ;
#13225 = VERTEX_POINT ( 'NONE', #21784 ) ;
#13226 = AXIS2_PLACEMENT_3D ( 'NONE', #7870, #19305, #30718 ) ;
#13227 = FACE_BOUND ( 'NONE', #25637, .T. ) ;
#13228 = EDGE_CURVE ( 'NONE', #31910, #29798, #13635, .T. ) ;
#13229 = EDGE_LOOP ( 'NONE', ( #973, #11395, #34813, #27407, #14166, #8616 ) ) ;
#13230 = LINE ( 'NONE', #32926, #5153 ) ;
#13231 = EDGE_CURVE ( 'NONE', #3923, #24921, #36863, .T. ) ;
#13232 = CARTESIAN_POINT ( 'NONE',  ( -46.00000000000000000, 103.4105893997321886, -19.99999999999999645 ) ) ;
#13233 = LINE ( 'NONE', #24677, #24535 ) ;
#13234 = CARTESIAN_POINT ( 'NONE',  ( 26.99999662536859546, -77.94228634059960825, 17.49999999999999645 ) ) ;
#13235 = ORIENTED_EDGE ( 'NONE', *, *, #26768, .T. ) ;
#13236 = CARTESIAN_POINT ( 'NONE',  ( 69.99999662536839651, 34.64101615137758472, -5.000000000000000000 ) ) ;
#13237 = DIRECTION ( 'NONE',  ( -1.000000000000000000, 0.000000000000000000, 0.000000000000000000 ) ) ;
#13238 = DIRECTION ( 'NONE',  ( -0.000000000000000000, -0.000000000000000000, 1.000000000000000000 ) ) ;
#13239 = ORIENTED_EDGE ( 'NONE', *, *, #12134, .T. ) ;
#13240 = DIRECTION ( 'NONE',  ( -1.000000000000000000, 0.000000000000000000, 0.000000000000000000 ) ) ;
#13241 = DIRECTION ( 'NONE',  ( 0.000000000000000000, 0.000000000000000000, 1.000000000000000000 ) ) ;
#13242 = ORIENTED_EDGE ( 'NONE', *, *, #2980, .T. ) ;
#13243 = DIRECTION ( 'NONE',  ( 1.000000000000000000, 0.000000000000000000, 0.000000000000000000 ) ) ;
#13244 = CARTESIAN_POINT ( 'NONE',  ( 110.2237710830529664, -101.7384897088154929, 32.55002500000000509 ) ) ;
#13245 = CARTESIAN_POINT ( 'NONE',  ( 77.93343913441647430, -72.12058696850856165, 32.50002500000000083 ) ) ;
#13246 = EDGE_CURVE ( 'NONE', #19401, #3360, #28010, .T. ) ;
#13247 = ORIENTED_EDGE ( 'NONE', *, *, #35219, .F. ) ;
#13248 = EDGE_LOOP ( 'NONE', ( #8228, #9745, #24483, #2396 ) ) ;
#13249 = CARTESIAN_POINT ( 'NONE',  ( 62.97617850287784336, 4.279621169095339184, -49.86561046011506448 ) ) ;
#13250 = CARTESIAN_POINT ( 'NONE',  ( -5.000000000000006217, 2.886751345948105563, -4.069520038198739087 ) ) ;
#13251 = EDGE_CURVE ( 'NONE', #19079, #28212, #2295, .T. ) ;
#13252 = DIRECTION ( 'NONE',  ( 0.000000000000000000, 0.000000000000000000, -1.000000000000000000 ) ) ;
#13253 = ORIENTED_EDGE ( 'NONE', *, *, #31625, .F. ) ;
#13254 = ADVANCED_FACE ( 'NONE', ( #10538 ), #21983, .F. ) ;
#13255 = DIRECTION ( 'NONE',  ( -1.000000000000000000, 0.000000000000000000, 0.000000000000000000 ) ) ;
#13256 = CARTESIAN_POINT ( 'NONE',  ( -57.00000337463107059, 60.62177826491078747, 17.49999999999999645 ) ) ;
#13257 = CARTESIAN_POINT ( 'NONE',  ( 0.3000000000000016542, 0.000000000000000000, 0.000000000000000000 ) ) ;
#13258 = DIRECTION ( 'NONE',  ( 1.000000000000000000, 0.000000000000000000, 0.000000000000000000 ) ) ;
#13259 = VERTEX_POINT ( 'NONE', #33426 ) ;
#13260 = EDGE_LOOP ( 'NONE', ( #18700, #24452 ) ) ;
#13261 = CARTESIAN_POINT ( 'NONE',  ( -20.00000337463122690, 86.60254037844397601, -9.999999999999998224 ) ) ;
#13262 = DIRECTION ( 'NONE',  ( 0.000000000000000000, 0.000000000000000000, -1.000000000000000000 ) ) ;
#13263 = EDGE_LOOP ( 'NONE', ( #10979, #14888, #24846, #2826 ) ) ;
#13264 = DIRECTION ( 'NONE',  ( 0.000000000000000000, 0.000000000000000000, 1.000000000000000000 ) ) ;
#13265 = VERTEX_POINT ( 'NONE', #7359 ) ;
#13266 = AXIS2_PLACEMENT_3D ( 'NONE', #32042, #752, #6383 ) ;
#13267 = DIRECTION ( 'NONE',  ( 0.000000000000000000, 0.000000000000000000, -1.000000000000000000 ) ) ;
#13268 = EDGE_CURVE ( 'NONE', #3324, #24335, #16104, .T. ) ;
#13269 = CARTESIAN_POINT ( 'NONE',  ( 66.99999662536841072, 25.98076211353318854, -9.999999999999998224 ) ) ;
#13270 = EDGE_LOOP ( 'NONE', ( #36686, #11799, #15786, #27647 ) ) ;
#13271 = DIRECTION ( 'NONE',  ( 0.000000000000000000, 0.000000000000000000, 1.000000000000000000 ) ) ;
#13272 = EDGE_LOOP ( 'NONE', ( #23432, #3323 ) ) ;
#13273 = DIRECTION ( 'NONE',  ( 1.000000000000000000, 0.000000000000000000, 0.000000000000000000 ) ) ;
#13274 = CYLINDRICAL_SURFACE ( 'NONE', #21538, 2.000000000000001776 ) ;
#13275 = DIRECTION ( 'NONE',  ( 0.000000000000000000, 0.000000000000000000, 1.000000000000000000 ) ) ;
#13276 = VERTEX_POINT ( 'NONE', #16355 ) ;
#13277 = CARTESIAN_POINT ( 'NONE',  ( -19.53925848833874213, 89.94802294027088863, 30.77834620192012594 ) ) ;
#13278 = DIRECTION ( 'NONE',  ( 1.000000000000000000, 0.000000000000000000, 0.000000000000000000 ) ) ;
#13279 = CYLINDRICAL_SURFACE ( 'NONE', #11156, 2.000000000000000000 ) ;
#13280 = ORIENTED_EDGE ( 'NONE', *, *, #32087, .T. ) ;
#13281 = EDGE_LOOP ( 'NONE', ( #35927, #12819 ) ) ;
#13282 = EDGE_CURVE ( 'NONE', #24999, #625, #8391, .T. ) ;
#13283 = VERTEX_POINT ( 'NONE', #5303 ) ;
#13284 = VECTOR ( 'NONE', #17852, 1000.000000000000000 ) ;
#13285 = CYLINDRICAL_SURFACE ( 'NONE', #20961, 2.000000000000001776 ) ;
#13286 = EDGE_CURVE ( 'NONE', #11018, #13221, #2309, .T. ) ;
#13287 = ORIENTED_EDGE ( 'NONE', *, *, #34712, .T. ) ;
#13288 = CARTESIAN_POINT ( 'NONE',  ( -5.000000000000000000, -1.349638343847294752, -0.8687551798607462405 ) ) ;
#13289 = CARTESIAN_POINT ( 'NONE',  ( -65.00000337463104927, -25.98076211353322051, -5.000000000000000000 ) ) ;
#13290 = EDGE_CURVE ( 'NONE', #10452, #28544, #1124, .T. ) ;
#13291 = CYLINDRICAL_SURFACE ( 'NONE', #3065, 2.000000000000001776 ) ;
#13292 = DIRECTION ( 'NONE',  ( 0.000000000000000000, 0.000000000000000000, 1.000000000000000000 ) ) ;
#13293 = LINE ( 'NONE', #16137, #8309 ) ;
#13294 = DIRECTION ( 'NONE',  ( -0.8191520442889917986, 1.003171929053524747E-16, 0.5735764363510460484 ) ) ;
#13295 = EDGE_CURVE ( 'NONE', #1072, #30254, #8313, .T. ) ;
#13296 = DIRECTION ( 'NONE',  ( 0.000000000000000000, 0.000000000000000000, 1.000000000000000000 ) ) ;
#13297 = ADVANCED_FACE ( 'NONE', ( #17623 ), #36979, .T. ) ;
#13298 = CARTESIAN_POINT ( 'NONE',  ( -9.974659986866640793E-15, -5.773502691896262640, -5.553418012614792509 ) ) ;
#13299 = ORIENTED_EDGE ( 'NONE', *, *, #16427, .F. ) ;
#13300 = ORIENTED_EDGE ( 'NONE', *, *, #27783, .F. ) ;
#13301 = DIRECTION ( 'NONE',  ( 0.000000000000000000, 0.000000000000000000, 1.000000000000000000 ) ) ;
#13302 = CARTESIAN_POINT ( 'NONE',  ( 62.99999662536839651, 60.62177826491078747, -9.999999999999998224 ) ) ;
#13303 = FACE_OUTER_BOUND ( 'NONE', #9794, .T. ) ;
#13304 = CARTESIAN_POINT ( 'NONE',  ( 14.99999662536863632, -77.94228634059960825, 12.50000000000000000 ) ) ;
#13305 = ORIENTED_EDGE ( 'NONE', *, *, #21943, .F. ) ;
#13306 = EDGE_CURVE ( 'NONE', #3560, #4570, #35937, .T. ) ;
#13307 = ADVANCED_FACE ( 'NONE', ( #191 ), #28712, .T. ) ;
#13308 = LINE ( 'NONE', #16321, #3952 ) ;
#13309 = EDGE_CURVE ( 'NONE', #16830, #9234, #34525, .T. ) ;
#13310 = CARTESIAN_POINT ( 'NONE',  ( 5.000000000000000888, -1.831125658499874742, -1.158123955083391943 ) ) ;
#13311 = VERTEX_POINT ( 'NONE', #17086 ) ;
#13312 = AXIS2_PLACEMENT_3D ( 'NONE', #7525, #13511, #24612 ) ;
#13313 = EDGE_CURVE ( 'NONE', #18465, #6603, #28515, .T. ) ;
#13314 = DIRECTION ( 'NONE',  ( 0.000000000000000000, -0.5000000000000013323, -0.8660254037844379305 ) ) ;
#13315 = ORIENTED_EDGE ( 'NONE', *, *, #23821, .F. ) ;
#13316 = DIRECTION ( 'NONE',  ( -1.000000000000000000, 0.000000000000000000, 0.000000000000000000 ) ) ;
#13317 = CARTESIAN_POINT ( 'NONE',  ( 52.99999662536844625, 43.30127018922198801, -9.999999999999998224 ) ) ;
#13318 = CARTESIAN_POINT ( 'NONE',  ( 0.9112620892300974385, 5.247385279376962863, -1.160540885688332136 ) ) ;
#13319 = ORIENTED_EDGE ( 'NONE', *, *, #24114, .T. ) ;
#13320 = ORIENTED_EDGE ( 'NONE', *, *, #9854, .T. ) ;
#13321 = VECTOR ( 'NONE', #34934, 1000.000000000000000 ) ;
#13322 = EDGE_CURVE ( 'NONE', #14326, #26888, #34065, .T. ) ;
#13323 = VERTEX_POINT ( 'NONE', #31163 ) ;
#13324 = PLANE ( 'NONE',  #13586 ) ;
#13325 = DIRECTION ( 'NONE',  ( 1.000000000000000000, 0.000000000000000000, 0.000000000000000000 ) ) ;
#13326 = CARTESIAN_POINT ( 'NONE',  ( 71.99999662536839651, -17.32050807568879947, 12.50000000000000000 ) ) ;
#13327 = PLANE ( 'NONE',  #22874 ) ;
#13328 = CARTESIAN_POINT ( 'NONE',  ( -19.31922176934808633, 76.99660315353983719, 27.49999999999999645 ) ) ;
#13329 = ORIENTED_EDGE ( 'NONE', *, *, #806, .F. ) ;
#13330 = DIRECTION ( 'NONE',  ( -1.000000000000000000, 0.000000000000000000, 0.000000000000000000 ) ) ;
#13331 = CYLINDRICAL_SURFACE ( 'NONE', #15612, 2.000000000000000000 ) ;
#13332 = CYLINDRICAL_SURFACE ( 'NONE', #2037, 2.000000000000001776 ) ;
#13333 = ORIENTED_EDGE ( 'NONE', *, *, #6612, .T. ) ;
#13334 = AXIS2_PLACEMENT_3D ( 'NONE', #5689, #25774, #28367 ) ;
#13335 = DIRECTION ( 'NONE',  ( 0.000000000000000000, 0.000000000000000000, 1.000000000000000000 ) ) ;
#13336 = EDGE_CURVE ( 'NONE', #19938, #36735, #22137, .T. ) ;
#13337 = CARTESIAN_POINT ( 'NONE',  ( 3.000000000000000000, -2.935248768560059229, 3.469446951953614189E-15 ) ) ;
#13338 = ORIENTED_EDGE ( 'NONE', *, *, #20789, .T. ) ;
#13339 = ORIENTED_EDGE ( 'NONE', *, *, #18244, .T. ) ;
#13340 = DIRECTION ( 'NONE',  ( 0.000000000000000000, 0.000000000000000000, 1.000000000000000000 ) ) ;
#13341 = CARTESIAN_POINT ( 'NONE',  ( 5.211749180171788787, -2.764497899775276935, -4.027903350935054583 ) ) ;
#13342 = CARTESIAN_POINT ( 'NONE',  ( -2.500000000000006217, -4.330127018922186544, 0.000000000000000000 ) ) ;
#13343 = ORIENTED_EDGE ( 'NONE', *, *, #27036, .T. ) ;
#13344 = VERTEX_POINT ( 'NONE', #5847 ) ;
#13345 = VERTEX_POINT ( 'NONE', #11817 ) ;
#13346 = ADVANCED_FACE ( 'NONE', ( #25731 ), #29058, .F. ) ;
#13347 = DIRECTION ( 'NONE',  ( 1.000000000000000000, 0.000000000000000000, -0.000000000000000000 ) ) ;
#13348 = ADVANCED_FACE ( 'NONE', ( #14629 ), #20275, .F. ) ;
#13349 = VERTEX_POINT ( 'NONE', #14079 ) ;
#13350 = ADVANCED_FACE ( 'NONE', ( #6034 ), #25532, .F. ) ;
#13351 = DIRECTION ( 'NONE',  ( 0.000000000000000000, 0.000000000000000000, 1.000000000000000000 ) ) ;
#13352 = VERTEX_POINT ( 'NONE', #22530 ) ;
#13353 = EDGE_LOOP ( 'NONE', ( #25939, #19367, #9808, #13067 ) ) ;
#13354 = DIRECTION ( 'NONE',  ( -1.000000000000000000, 0.000000000000000000, 0.000000000000000000 ) ) ;
#13355 = AXIS2_PLACEMENT_3D ( 'NONE', #35622, #27359, #1300 ) ;
#13356 = DIRECTION ( 'NONE',  ( 0.000000000000000000, 0.000000000000000000, 1.000000000000000000 ) ) ;
#13357 = VERTEX_POINT ( 'NONE', #20443 ) ;
#13358 = ORIENTED_EDGE ( 'NONE', *, *, #4783, .F. ) ;
#13359 = FACE_OUTER_BOUND ( 'NONE', #20006, .T. ) ;
#13360 = DIRECTION ( 'NONE',  ( 0.000000000000000000, 0.000000000000000000, 1.000000000000000000 ) ) ;
#13361 = DIRECTION ( 'NONE',  ( -0.000000000000000000, -0.000000000000000000, -1.000000000000000000 ) ) ;
#13362 = CARTESIAN_POINT ( 'NONE',  ( 59.99999662536842493, -51.96152422706639840, -9.999999999999998224 ) ) ;
#13363 = ORIENTED_EDGE ( 'NONE', *, *, #32475, .T. ) ;
#13364 = CARTESIAN_POINT ( 'NONE',  ( -40.00000337463113453, 69.28203230275516944, 17.49999999999999645 ) ) ;
#13365 = FACE_BOUND ( 'NONE', #17699, .T. ) ;
#13366 = CARTESIAN_POINT ( 'NONE',  ( 4.999996625368645198, 77.94228634059957983, 17.49999999999999645 ) ) ;
#13367 = AXIS2_PLACEMENT_3D ( 'NONE', #3250, #29110, #31741 ) ;
#13368 = CARTESIAN_POINT ( 'NONE',  ( -45.00000000000000711, 5.510910596163090344E-15, -10.00000000000000000 ) ) ;
#13369 = CARTESIAN_POINT ( 'NONE',  ( 79.99999662536833966, 17.32050807568879236, 17.49999999999999645 ) ) ;
#13370 = ADVANCED_FACE ( 'NONE', ( #26076 ), #31862, .F. ) ;
#13371 = DIRECTION ( 'NONE',  ( 0.000000000000000000, 0.000000000000000000, 1.000000000000000000 ) ) ;
#13372 = AXIS2_PLACEMENT_3D ( 'NONE', #7451, #24144, #10094 ) ;
#13373 = FACE_OUTER_BOUND ( 'NONE', #13907, .T. ) ;
#13374 = DIRECTION ( 'NONE',  ( -0.7071067811865288100, 8.659560562355164586E-17, -0.7071067811865663355 ) ) ;
#13375 = ORIENTED_EDGE ( 'NONE', *, *, #25915, .F. ) ;
#13376 = CARTESIAN_POINT ( 'NONE',  ( -63.00000337463102085, 43.30127018922198801, 17.49999999999999645 ) ) ;
#13377 = CARTESIAN_POINT ( 'NONE',  ( 59.99999662536845335, 34.64101615137759893, 17.49999999999999645 ) ) ;
#13378 = DIRECTION ( 'NONE',  ( 0.000000000000000000, 0.000000000000000000, 1.000000000000000000 ) ) ;
#13379 = MECHANICAL_DESIGN_GEOMETRIC_PRESENTATION_REPRESENTATION (  '', ( #26574 ), #2627 ) ;
#13380 = EDGE_LOOP ( 'NONE', ( #9290, #8793, #6449, #12538 ) ) ;
#13381 = ORIENTED_EDGE ( 'NONE', *, *, #18888, .T. ) ;
#13382 = ORIENTED_EDGE ( 'NONE', *, *, #1848, .T. ) ;
#13383 = CIRCLE ( 'NONE', #20544, 2.000000000000001776 ) ;
#13384 = DIRECTION ( 'NONE',  ( 1.000000000000000000, 0.000000000000000000, 0.000000000000000000 ) ) ;
#13385 = DIRECTION ( 'NONE',  ( 1.000000000000000000, 0.000000000000000000, 0.000000000000000000 ) ) ;
#13386 = ORIENTED_EDGE ( 'NONE', *, *, #1476, .T. ) ;
#13387 = AXIS2_PLACEMENT_3D ( 'NONE', #15662, #12818, #838 ) ;
#13388 = PRODUCT_DEFINITION_SHAPE ( 'NONE', 'NONE',  #37130 ) ;
#13389 = CARTESIAN_POINT ( 'NONE',  ( 24.99999662536857059, 77.94228634059957983, 17.49999999999999645 ) ) ;
#13390 = CARTESIAN_POINT ( 'NONE',  ( -73.00000337463097821, 43.30127018922197379, 12.50000000000000000 ) ) ;
#13391 = ORIENTED_EDGE ( 'NONE', *, *, #25173, .T. ) ;
#13392 = EDGE_CURVE ( 'NONE', #13968, #1946, #35851, .T. ) ;
#13393 = CARTESIAN_POINT ( 'NONE',  ( -25.00000337463120914, 77.94228634059957983, -9.999999999999998224 ) ) ;
#13394 = EDGE_LOOP ( 'NONE', ( #555, #17418 ) ) ;
#13395 = FACE_BOUND ( 'NONE', #8553, .T. ) ;
#13396 = AXIS2_PLACEMENT_3D ( 'NONE', #36689, #8384, #2741 ) ;
#13397 = DIRECTION ( 'NONE',  ( 1.000000000000000000, 0.000000000000000000, 0.000000000000000000 ) ) ;
#13398 = DIRECTION ( 'NONE',  ( 0.000000000000000000, 0.000000000000000000, 1.000000000000000000 ) ) ;
#13399 = DIRECTION ( 'NONE',  ( -1.000000000000000000, 0.000000000000000000, 0.000000000000000000 ) ) ;
#13400 = ORIENTED_EDGE ( 'NONE', *, *, #20660, .T. ) ;
#13401 = DIRECTION ( 'NONE',  ( 1.000000000000000000, 0.000000000000000000, 0.000000000000000000 ) ) ;
#13402 = CIRCLE ( 'NONE', #2653, 2.000000000000000000 ) ;
#13403 = CARTESIAN_POINT ( 'NONE',  ( -20.00000337463124112, 69.28203230275516944, -9.999999999999998224 ) ) ;
#13404 = DIRECTION ( 'NONE',  ( 0.000000000000000000, 0.000000000000000000, 1.000000000000000000 ) ) ;
#13405 = ORIENTED_EDGE ( 'NONE', *, *, #32263, .T. ) ;
#13406 = CARTESIAN_POINT ( 'NONE',  ( 39.99999662536853151, 69.28203230275518365, -5.000000000000000000 ) ) ;
#13407 = DIRECTION ( 'NONE',  ( 0.000000000000000000, 0.000000000000000000, 1.000000000000000000 ) ) ;
#13408 = EDGE_LOOP ( 'NONE', ( #24145, #31132, #765, #25241, #30132 ) ) ;
#13409 = DIRECTION ( 'NONE',  ( 0.000000000000000000, 0.000000000000000000, -1.000000000000000000 ) ) ;
#13410 = DIRECTION ( 'NONE',  ( 1.000000000000000000, 0.000000000000000000, 0.000000000000000000 ) ) ;
#13411 = DIRECTION ( 'NONE',  ( 0.000000000000000000, 0.000000000000000000, 1.000000000000000000 ) ) ;
#13412 = ADVANCED_FACE ( 'NONE', ( #35078 ), #34895, .F. ) ;
#13413 = ORIENTED_EDGE ( 'NONE', *, *, #21563, .T. ) ;
#13414 = EDGE_LOOP ( 'NONE', ( #18994, #32798 ) ) ;
#13415 = EDGE_CURVE ( 'NONE', #875, #18552, #22676, .T. ) ;
#13416 = LINE ( 'NONE', #18523, #20754 ) ;
#13417 = CARTESIAN_POINT ( 'NONE',  ( -4.279621169095561228, 62.97617850287782915, -4.999999999999997335 ) ) ;
#13418 = AXIS2_PLACEMENT_3D ( 'NONE', #32352, #6838, #12464 ) ;
#13419 = CARTESIAN_POINT ( 'NONE',  ( -30.00000337463118427, 69.28203230275516944, 12.50000000000000000 ) ) ;
#13421 = ORIENTED_EDGE ( 'NONE', *, *, #34300, .F. ) ;
#13420 = EDGE_CURVE ( 'NONE', #816, #17546, #5122, .T. ) ;
#13422 = EDGE_LOOP ( 'NONE', ( #22031, #12142, #26094, #25959 ) ) ;
#13423 = DIRECTION ( 'NONE',  ( 0.000000000000000000, 0.000000000000000000, 1.000000000000000000 ) ) ;
#13424 = CYLINDRICAL_SURFACE ( 'NONE', #6473, 65.00000000000000000 ) ;
#13425 = DIRECTION ( 'NONE',  ( 1.000000000000000000, 0.000000000000000000, 0.000000000000000000 ) ) ;
#13426 = DIRECTION ( 'NONE',  ( 0.000000000000000000, 0.000000000000000000, 1.000000000000000000 ) ) ;
#13427 = VERTEX_POINT ( 'NONE', #32255 ) ;
#13428 = AXIS2_PLACEMENT_3D ( 'NONE', #3555, #29578, #12133 ) ;
#13429 = CIRCLE ( 'NONE', #260, 2.000000000000001776 ) ;
#13430 = ORIENTED_EDGE ( 'NONE', *, *, #1950, .T. ) ;
#13431 = CARTESIAN_POINT ( 'NONE',  ( 5.000000000000000888, 1.953108124182682648, -0.2699991669428374874 ) ) ;
#13432 = AXIS2_PLACEMENT_3D ( 'NONE', #15932, #27721, #16477 ) ;
#13433 = DIRECTION ( 'NONE',  ( -0.000000000000000000, -0.000000000000000000, 1.000000000000000000 ) ) ;
#13434 = ORIENTED_EDGE ( 'NONE', *, *, #36596, .F. ) ;
#13435 = EDGE_CURVE ( 'NONE', #7613, #14564, #10101, .T. ) ;
#13436 = CARTESIAN_POINT ( 'NONE',  ( -19.13981058454750794, 60.93295298010998806, 12.49999999999999822 ) ) ;
#13437 = VERTEX_POINT ( 'NONE', #4323 ) ;
#13438 = DIRECTION ( 'NONE',  ( 1.000000000000000000, 0.000000000000000000, 0.000000000000000000 ) ) ;
#13439 = DIRECTION ( 'NONE',  ( 0.000000000000000000, 0.000000000000000000, 1.000000000000000000 ) ) ;
#13440 = CIRCLE ( 'NONE', #24841, 2.000000000000001776 ) ;
#13441 = AXIS2_PLACEMENT_3D ( 'NONE', #12145, #23054, #29237 ) ;
#13442 = CYLINDRICAL_SURFACE ( 'NONE', #28445, 2.000000000000001776 ) ;
#13443 = EDGE_LOOP ( 'NONE', ( #4267, #27642 ) ) ;
#13444 = EDGE_CURVE ( 'NONE', #8665, #13345, #17299, .T. ) ;
#13445 = VECTOR ( 'NONE', #29612, 1000.000000000000000 ) ;
#13446 = CARTESIAN_POINT ( 'NONE',  ( 19.99999662536858835, 69.28203230275516944, 17.49999999999999645 ) ) ;
#13447 = FACE_OUTER_BOUND ( 'NONE', #9727, .T. ) ;
#13448 = DIRECTION ( 'NONE',  ( 0.000000000000000000, -0.5000000000000011102, -0.8660254037844379305 ) ) ;
#13449 = ADVANCED_FACE ( 'NONE', ( #35286 ), #12734, .F. ) ;
#13450 = EDGE_LOOP ( 'NONE', ( #19098, #2990, #8186, #16908 ) ) ;
#13451 = CARTESIAN_POINT ( 'NONE',  ( -52.39915983220772233, -35.19434990244957362, 12.49999999999999822 ) ) ;
#13452 = DIRECTION ( 'NONE',  ( 0.000000000000000000, 0.000000000000000000, 1.000000000000000000 ) ) ;
#13453 = DIRECTION ( 'NONE',  ( 1.000000000000000000, 0.000000000000000000, 0.000000000000000000 ) ) ;
#13454 = ORIENTED_EDGE ( 'NONE', *, *, #5438, .F. ) ;
#13455 = AXIS2_PLACEMENT_3D ( 'NONE', #17946, #32174, #31796 ) ;
#13456 = EDGE_CURVE ( 'NONE', #16882, #1598, #19108, .T. ) ;
#13457 = VECTOR ( 'NONE', #28936, 1000.000000000000000 ) ;
#13458 = EDGE_LOOP ( 'NONE', ( #20531, #29676, #24537, #22161, #9235 ) ) ;
#13459 = AXIS2_PLACEMENT_3D ( 'NONE', #14730, #484, #7827 ) ;
#13460 = ORIENTED_EDGE ( 'NONE', *, *, #238, .F. ) ;
#13461 = CARTESIAN_POINT ( 'NONE',  ( 47.99999662536848177, -51.96152422706640550, -9.999999999999998224 ) ) ;
#13462 = APPLICATION_CONTEXT ( 'automotive_design' ) ;
#13463 = ORIENTED_EDGE ( 'NONE', *, *, #15761, .F. ) ;
#13464 = EDGE_CURVE ( 'NONE', #3339, #14569, #29438, .T. ) ;
#13465 = DIRECTION ( 'NONE',  ( -0.000000000000000000, -0.000000000000000000, -1.000000000000000000 ) ) ;
#13466 = CARTESIAN_POINT ( 'NONE',  ( -10.00000337463128197, 86.60254037844397601, -9.999999999999998224 ) ) ;
#13467 = CARTESIAN_POINT ( 'NONE',  ( -45.00000337463111322, -77.94228634059960825, -9.999999999999998224 ) ) ;
#13468 = EDGE_CURVE ( 'NONE', #14001, #27785, #34144, .T. ) ;
#13469 = CARTESIAN_POINT ( 'NONE',  ( -51.13139720814438505, -27.49999999999955591, 5.000000000000000888 ) ) ;
#13470 = DIRECTION ( 'NONE',  ( 0.000000000000000000, 0.000000000000000000, 1.000000000000000000 ) ) ;
#13471 = CYLINDRICAL_SURFACE ( 'NONE', #32354, 2.000000000000001776 ) ;
#13472 = AXIS2_PLACEMENT_3D ( 'NONE', #7026, #1386, #36265 ) ;
#13473 = CARTESIAN_POINT ( 'NONE',  ( 32.99999662536855283, -60.62177826491080168, -9.999999999999998224 ) ) ;
#13474 = CYLINDRICAL_SURFACE ( 'NONE', #10660, 2.000000000000001776 ) ;
#13475 = AXIS2_PLACEMENT_3D ( 'NONE', #26179, #113, #22826 ) ;
#13476 = EDGE_LOOP ( 'NONE', ( #31447, #9676 ) ) ;
#13477 = AXIS2_PLACEMENT_3D ( 'NONE', #2604, #34479, #31653 ) ;
#13478 = EDGE_LOOP ( 'NONE', ( #19906, #35429 ) ) ;
#13479 = DIRECTION ( 'NONE',  ( 0.000000000000000000, 0.000000000000000000, -1.000000000000000000 ) ) ;
#13480 = DIRECTION ( 'NONE',  ( -0.000000000000000000, -0.000000000000000000, 1.000000000000000000 ) ) ;
#13481 = DIRECTION ( 'NONE',  ( 1.000000000000000000, 0.000000000000000000, 0.000000000000000000 ) ) ;
#13482 = DIRECTION ( 'NONE',  ( 0.000000000000000000, 0.000000000000000000, -1.000000000000000000 ) ) ;
#13483 = EDGE_LOOP ( 'NONE', ( #3153, #22700 ) ) ;
#13484 = CIRCLE ( 'NONE', #8117, 2.000000000000001776 ) ;
#13485 = VECTOR ( 'NONE', #21854, 999.9999999999998863 ) ;
#13486 = CARTESIAN_POINT ( 'NONE',  ( -62.00000337463107769, -34.64101615137762025, -5.000000000000000000 ) ) ;
#13487 = EDGE_CURVE ( 'NONE', #23506, #22424, #23886, .T. ) ;
#13488 = DIRECTION ( 'NONE',  ( 1.000000000000000000, 0.000000000000000000, 0.000000000000000000 ) ) ;
#13489 = VERTEX_POINT ( 'NONE', #18588 ) ;
#13490 = DIRECTION ( 'NONE',  ( 1.000000000000000000, 0.000000000000000000, 0.000000000000000000 ) ) ;
#13491 = ORIENTED_EDGE ( 'NONE', *, *, #2294, .F. ) ;
#13492 = SURFACE_STYLE_FILL_AREA ( #1888 ) ;
#13493 = DIRECTION ( 'NONE',  ( 0.000000000000000000, 0.000000000000000000, -1.000000000000000000 ) ) ;
#13494 = EDGE_CURVE ( 'NONE', #26470, #14180, #12845, .T. ) ;
#13495 = CARTESIAN_POINT ( 'NONE',  ( 20.00000000000001066, 89.94802294027088863, -19.99999999999999645 ) ) ;
#13496 = AXIS2_PLACEMENT_3D ( 'NONE', #19244, #34235, #31036 ) ;
#13497 = LINE ( 'NONE', #22148, #29256 ) ;
#13498 = EDGE_CURVE ( 'NONE', #3789, #24921, #32440, .T. ) ;
#13499 = ORIENTED_EDGE ( 'NONE', *, *, #36442, .F. ) ;
#13500 = AXIS2_PLACEMENT_3D ( 'NONE', #35113, #12396, #222 ) ;
#13501 = ORIENTED_EDGE ( 'NONE', *, *, #36200, .F. ) ;
#13502 = ADVANCED_FACE ( 'NONE', ( #21188 ), #17825, .F. ) ;
#13503 = VECTOR ( 'NONE', #15525, 1000.000000000000000 ) ;
#13504 = AXIS2_PLACEMENT_3D ( 'NONE', #30607, #27782, #16190 ) ;
#13505 = CIRCLE ( 'NONE', #8752, 2.000000000000001776 ) ;
#13506 = AXIS2_PLACEMENT_3D ( 'NONE', #30323, #4843, #15707 ) ;
#13507 = ORIENTED_EDGE ( 'NONE', *, *, #26839, .T. ) ;
#13508 = LINE ( 'NONE', #19708, #401 ) ;
#13509 = DIRECTION ( 'NONE',  ( -0.000000000000000000, -0.000000000000000000, 1.000000000000000000 ) ) ;
#13510 = CARTESIAN_POINT ( 'NONE',  ( 4.999999999999999112, -2.886751345948144198, -3.984345921091770659 ) ) ;
#13511 = DIRECTION ( 'NONE',  ( 0.000000000000000000, 0.000000000000000000, 1.000000000000000000 ) ) ;
#13512 = CYLINDRICAL_SURFACE ( 'NONE', #1564, 2.000000000000001776 ) ;
#13513 = VERTEX_POINT ( 'NONE', #29259 ) ;
#13514 = CARTESIAN_POINT ( 'NONE',  ( 24.99999662536859546, -77.94228634059960825, 12.50000000000000000 ) ) ;
#13515 = AXIS2_PLACEMENT_3D ( 'NONE', #6199, #3046, #25898 ) ;
#13516 = CYLINDRICAL_SURFACE ( 'NONE', #26369, 3.499999999999991562 ) ;
#13517 = EDGE_CURVE ( 'NONE', #29590, #16919, #7712, .T. ) ;
#13518 = DIRECTION ( 'NONE',  ( 1.000000000000000000, 0.000000000000000000, 0.000000000000000000 ) ) ;
#13519 = ORIENTED_EDGE ( 'NONE', *, *, #8071, .F. ) ;
#13520 = CARTESIAN_POINT ( 'NONE',  ( -12.00000337463127842, -69.28203230275519786, -9.999999999999998224 ) ) ;
#13521 = CARTESIAN_POINT ( 'NONE',  ( 43.00330684490809574, 60.50675687296563865, 12.50000000000000000 ) ) ;
#13522 = ORIENTED_EDGE ( 'NONE', *, *, #28077, .F. ) ;
#13523 = AXIS2_PLACEMENT_3D ( 'NONE', #15082, #12441, #11698 ) ;
#13524 = EDGE_LOOP ( 'NONE', ( #29670, #5346, #13869, #2565 ) ) ;
#13525 = DIRECTION ( 'NONE',  ( 0.000000000000000000, 0.000000000000000000, -1.000000000000000000 ) ) ;
#13526 = FACE_OUTER_BOUND ( 'NONE', #31379, .T. ) ;
#13527 = DIRECTION ( 'NONE',  ( 0.000000000000000000, 0.000000000000000000, 1.000000000000000000 ) ) ;
#13528 = AXIS2_PLACEMENT_3D ( 'NONE', #12591, #29847, #30404 ) ;
#13529 = DIRECTION ( 'NONE',  ( 0.000000000000000000, 0.000000000000000000, 1.000000000000000000 ) ) ;
#13530 = EDGE_LOOP ( 'NONE', ( #5849, #18187 ) ) ;
#13531 = EDGE_LOOP ( 'NONE', ( #3246, #35756 ) ) ;
#13532 = CIRCLE ( 'NONE', #27907, 45.00000000000000000 ) ;
#13533 = VECTOR ( 'NONE', #9522, 1000.000000000000000 ) ;
#13534 = AXIS2_PLACEMENT_3D ( 'NONE', #30258, #7400, #9830 ) ;
#13535 = CARTESIAN_POINT ( 'NONE',  ( 64.99999662536842493, 43.30127018922200222, 17.49999999999999645 ) ) ;
#13536 = CIRCLE ( 'NONE', #14127, 2.000000000000001776 ) ;
#13537 = EDGE_CURVE ( 'NONE', #6894, #23662, #21471, .T. ) ;
#13538 = ORIENTED_EDGE ( 'NONE', *, *, #34909, .T. ) ;
#13539 = EDGE_CURVE ( 'NONE', #23807, #7638, #21550, .T. ) ;
#13540 = FACE_BOUND ( 'NONE', #24597, .T. ) ;
#13541 = VERTEX_POINT ( 'NONE', #19492 ) ;
#13542 = EDGE_LOOP ( 'NONE', ( #18583, #8826, #3583, #1745 ) ) ;
#13543 = AXIS2_PLACEMENT_3D ( 'NONE', #24112, #13038, #35559 ) ;
#13544 = EDGE_CURVE ( 'NONE', #29981, #20212, #30733, .T. ) ;
#13545 = CARTESIAN_POINT ( 'NONE',  ( -62.97617850287781494, -4.279621169095772615, -49.86561046011506448 ) ) ;
#13546 = CYLINDRICAL_SURFACE ( 'NONE', #17830, 2.000000000000001776 ) ;
#13547 = ORIENTED_EDGE ( 'NONE', *, *, #32717, .T. ) ;
#13548 = ORIENTED_EDGE ( 'NONE', *, *, #2508, .T. ) ;
#13549 = EDGE_CURVE ( 'NONE', #35451, #20281, #17962, .T. ) ;
#13550 = DIRECTION ( 'NONE',  ( 0.000000000000000000, 0.000000000000000000, 1.000000000000000000 ) ) ;
#13551 = DIRECTION ( 'NONE',  ( -0.000000000000000000, -0.000000000000000000, -1.000000000000000000 ) ) ;
#13552 = EDGE_CURVE ( 'NONE', #16108, #25244, #31049, .T. ) ;
#13553 = AXIS2_PLACEMENT_3D ( 'NONE', #5128, #10926, #16567 ) ;
#13554 = PLANE ( 'NONE',  #7299 ) ;
#13555 = LINE ( 'NONE', #18646, #13681 ) ;
#13556 = AXIS2_PLACEMENT_3D ( 'NONE', #17439, #563, #6019 ) ;
#13557 = ORIENTED_EDGE ( 'NONE', *, *, #11671, .F. ) ;
#13558 = DIRECTION ( 'NONE',  ( 0.000000000000000000, 0.000000000000000000, 1.000000000000000000 ) ) ;
#13559 = CARTESIAN_POINT ( 'NONE',  ( 72.99999662536836809, 43.30127018922198801, 12.50000000000000000 ) ) ;
#13560 = AXIS2_PLACEMENT_3D ( 'NONE', #20195, #25450, #22445 ) ;
#13561 = DIRECTION ( 'NONE',  ( 1.000000000000000000, 0.000000000000000000, 0.000000000000000000 ) ) ;
#13562 = DIRECTION ( 'NONE',  ( -0.000000000000000000, -0.000000000000000000, 1.000000000000000000 ) ) ;
#13563 = AXIS2_PLACEMENT_3D ( 'NONE', #10946, #22577, #25044 ) ;
#13564 = DIRECTION ( 'NONE',  ( 1.000000000000000000, 0.000000000000000000, 0.000000000000000000 ) ) ;
#13565 = ADVANCED_FACE ( 'NONE', ( #5053 ), #10310, .F. ) ;
#13566 = CIRCLE ( 'NONE', #21974, 27.00000000000001421 ) ;
#13567 = DIRECTION ( 'NONE',  ( 1.000000000000000000, 0.000000000000000000, 0.000000000000000000 ) ) ;
#13568 = VECTOR ( 'NONE', #980, 1000.000000000000000 ) ;
#13569 = EDGE_CURVE ( 'NONE', #29323, #22235, #33176, .T. ) ;
#13570 = AXIS2_PLACEMENT_3D ( 'NONE', #6869, #18310, #26558 ) ;
#13571 = CARTESIAN_POINT ( 'NONE',  ( -2.000003374631327713, 86.60254037844397601, 12.50000000000000000 ) ) ;
#13572 = EDGE_CURVE ( 'NONE', #27735, #33050, #26903, .T. ) ;
#13573 = EDGE_CURVE ( 'NONE', #25826, #29785, #5954, .T. ) ;
#13574 = DIRECTION ( 'NONE',  ( 0.000000000000000000, 0.000000000000000000, 1.000000000000000000 ) ) ;
#13575 = EDGE_LOOP ( 'NONE', ( #9278, #23778 ) ) ;
#13576 = DIRECTION ( 'NONE',  ( 0.000000000000000000, 0.000000000000000000, 1.000000000000000000 ) ) ;
#13577 = CARTESIAN_POINT ( 'NONE',  ( 24.99999662536859546, -77.94228634059960825, -5.000000000000000000 ) ) ;
#13578 = FACE_OUTER_BOUND ( 'NONE', #240, .T. ) ;
#13579 = ORIENTED_EDGE ( 'NONE', *, *, #35131, .T. ) ;
#13580 = AXIS2_PLACEMENT_3D ( 'NONE', #10362, #23893, #27614 ) ;
#13581 = VERTEX_POINT ( 'NONE', #5254 ) ;
#13582 = ORIENTED_EDGE ( 'NONE', *, *, #11493, .T. ) ;
#13583 = DIRECTION ( 'NONE',  ( 0.000000000000000000, 0.000000000000000000, -1.000000000000000000 ) ) ;
#13584 = CYLINDRICAL_SURFACE ( 'NONE', #10675, 2.000000000000001776 ) ;
#13585 = ORIENTED_EDGE ( 'NONE', *, *, #15029, .T. ) ;
#13586 = AXIS2_PLACEMENT_3D ( 'NONE', #10715, #16339, #36761 ) ;
#13587 = DIRECTION ( 'NONE',  ( -1.000000000000000000, 0.000000000000000000, 0.000000000000000000 ) ) ;
#13588 = VECTOR ( 'NONE', #34706, 1000.000000000000000 ) ;
#13589 = DIRECTION ( 'NONE',  ( 1.000000000000000000, 0.000000000000000000, 0.000000000000000000 ) ) ;
#13590 = ORIENTED_EDGE ( 'NONE', *, *, #14301, .F. ) ;
#13591 = AXIS2_PLACEMENT_3D ( 'NONE', #42, #19741, #36791 ) ;
#13592 = DIRECTION ( 'NONE',  ( 1.000000000000000000, 0.000000000000000000, 0.000000000000000000 ) ) ;
#13593 = ORIENTED_EDGE ( 'NONE', *, *, #34850, .T. ) ;
#13594 = DIRECTION ( 'NONE',  ( 0.000000000000000000, 0.000000000000000000, 1.000000000000000000 ) ) ;
#13595 = AXIS2_PLACEMENT_3D ( 'NONE', #18179, #29608, #3933 ) ;
#13596 = VECTOR ( 'NONE', #36583, 1000.000000000000000 ) ;
#13597 = CIRCLE ( 'NONE', #4643, 1.999999999999998224 ) ;
#13598 = CARTESIAN_POINT ( 'NONE',  ( 0.000000000000000000, 98.60827697811544112, 27.49999999999999645 ) ) ;
#13599 = CARTESIAN_POINT ( 'NONE',  ( 3.866666666667000651, 0.000000000000000000, 3.400000000000000355 ) ) ;
#13600 = ORIENTED_EDGE ( 'NONE', *, *, #16938, .T. ) ;
#13601 = DIRECTION ( 'NONE',  ( -1.000000000000000000, 0.000000000000000000, 0.000000000000000000 ) ) ;
#13602 = AXIS2_PLACEMENT_3D ( 'NONE', #13809, #22412, #11162 ) ;
#13603 = ITEM_DEFINED_TRANSFORMATION ( 'NONE', 'NONE', #9383,  #21385 ) ;
#13604 = AXIS2_PLACEMENT_3D ( 'NONE', #26280, #28883, #23086 ) ;
#13605 = CARTESIAN_POINT ( 'NONE',  ( 29.99999662536857770, -69.28203230275519786, -9.999999999999998224 ) ) ;
#13606 = CYLINDRICAL_SURFACE ( 'NONE', #9172, 2.000000000000001776 ) ;
#13607 = EDGE_LOOP ( 'NONE', ( #26239, #25579, #6391, #1149 ) ) ;
#13608 = CYLINDRICAL_SURFACE ( 'NONE', #26355, 2.000000000000001776 ) ;
#13609 = DIRECTION ( 'NONE',  ( 0.000000000000000000, 0.000000000000000000, 1.000000000000000000 ) ) ;
#13610 = ORIENTED_EDGE ( 'NONE', *, *, #24087, .T. ) ;
#13611 = CARTESIAN_POINT ( 'NONE',  ( -37.50000000000000000, 103.4105893997321743, 27.50000000000000000 ) ) ;
#13612 = VECTOR ( 'NONE', #7216, 1000.000000000000000 ) ;
#13613 = CARTESIAN_POINT ( 'NONE',  ( 79.99999662536832545, -17.32050807568879591, -5.000000000000000000 ) ) ;
#13614 = CARTESIAN_POINT ( 'NONE',  ( 5.185163620696820352, -2.993655612201285621, -4.330826434870608033 ) ) ;
#13615 = AXIS2_PLACEMENT_3D ( 'NONE', #14306, #34361, #8662 ) ;
#13616 = EDGE_LOOP ( 'NONE', ( #293, #33439, #9571, #27153 ) ) ;
#13617 = CIRCLE ( 'NONE', #19592, 2.000000000000001776 ) ;
#13618 = EDGE_CURVE ( 'NONE', #10634, #16319, #25103, .T. ) ;
#13619 = ORIENTED_EDGE ( 'NONE', *, *, #13569, .T. ) ;
#13620 = DIRECTION ( 'NONE',  ( 1.000000000000000000, 0.000000000000000000, 0.000000000000000000 ) ) ;
#13621 = DIRECTION ( 'NONE',  ( 1.000000000000000000, 0.000000000000000000, 0.000000000000000000 ) ) ;
#13622 = MECHANICAL_DESIGN_GEOMETRIC_PRESENTATION_REPRESENTATION (  '', ( #5256 ), #12936 ) ;
#13623 = CIRCLE ( 'NONE', #16628, 2.000000000000000000 ) ;
#13624 = CARTESIAN_POINT ( 'NONE',  ( -58.00000337463104216, 34.64101615137757051, 12.50000000000000000 ) ) ;
#13625 = AXIS2_PLACEMENT_3D ( 'NONE', #31382, #19409, #13795 ) ;
#13626 = EDGE_LOOP ( 'NONE', ( #29394, #9488, #18398, #16280 ) ) ;
#13627 = EDGE_LOOP ( 'NONE', ( #31851, #16180, #31045, #1789, #25510 ) ) ;
#13628 = CARTESIAN_POINT ( 'NONE',  ( -55.88972745734155012, 34.00000000000049027, -49.22241343995295892 ) ) ;
#13629 = DIRECTION ( 'NONE',  ( -0.000000000000000000, 0.000000000000000000, -1.000000000000000000 ) ) ;
#13630 = CARTESIAN_POINT ( 'NONE',  ( -78.00000337463096400, -34.64101615137762025, 17.49999999999999645 ) ) ;
#13631 = CARTESIAN_POINT ( 'NONE',  ( 69.99999662536841072, 51.96152422706640550, 12.50000000000000000 ) ) ;
#13632 = VERTEX_POINT ( 'NONE', #36573 ) ;
#13633 = ORIENTED_EDGE ( 'NONE', *, *, #4844, .F. ) ;
#13634 = CARTESIAN_POINT ( 'NONE',  ( 64.99999662536839651, -43.30127018922199511, -5.000000000000000000 ) ) ;
#13635 = CIRCLE ( 'NONE', #18434, 2.000000000000001776 ) ;
#13636 = DIRECTION ( 'NONE',  ( 1.000000000000000000, 0.000000000000000000, 0.000000000000000000 ) ) ;
#13637 = ORIENTED_EDGE ( 'NONE', *, *, #34904, .F. ) ;
#13638 = FACE_OUTER_BOUND ( 'NONE', #8199, .T. ) ;
#13639 = ORIENTED_EDGE ( 'NONE', *, *, #28441, .F. ) ;
#13640 = AXIS2_PLACEMENT_3D ( 'NONE', #34809, #11371, #31412 ) ;
#13641 = FACE_BOUND ( 'NONE', #12427, .T. ) ;
#13642 = EDGE_CURVE ( 'NONE', #34086, #13708, #27734, .T. ) ;
#13643 = EDGE_CURVE ( 'NONE', #27222, #28579, #10869, .T. ) ;
#13644 = CIRCLE ( 'NONE', #34000, 2.000000000000001776 ) ;
#13645 = CIRCLE ( 'NONE', #1061, 27.00000000000001066 ) ;
#13646 = CARTESIAN_POINT ( 'NONE',  ( -85.00000337463092137, 25.98076211353317433, -5.000000000000000000 ) ) ;
#13647 = PRODUCT_RELATED_PRODUCT_CATEGORY ( 'part', '', ( #11249 ) ) ;
#13648 = CARTESIAN_POINT ( 'NONE',  ( -3.374631289687624047E-06, -69.28203230275519786, -5.000000000000000000 ) ) ;
#13649 = ORIENTED_EDGE ( 'NONE', *, *, #2544, .T. ) ;
#13650 = DIRECTION ( 'NONE',  ( 0.2958803951453795600, 0.9552249953642408808, -2.706694063014923180E-17 ) ) ;
#13651 = DIRECTION ( 'NONE',  ( 0.000000000000000000, 0.000000000000000000, 1.000000000000000000 ) ) ;
#13652 = AXIS2_PLACEMENT_3D ( 'NONE', #28173, #2492, #13914 ) ;
#13653 = EDGE_CURVE ( 'NONE', #36171, #19268, #22307, .T. ) ;
#13654 = CYLINDRICAL_SURFACE ( 'NONE', #10785, 2.000000000000000000 ) ;
#13655 = DIRECTION ( 'NONE',  ( 0.000000000000000000, 0.000000000000000000, -1.000000000000000000 ) ) ;
#13656 = VERTEX_POINT ( 'NONE', #7319 ) ;
#13657 = DIRECTION ( 'NONE',  ( 1.000000000000000000, 0.000000000000000000, 0.000000000000000000 ) ) ;
#13658 = LINE ( 'NONE', #31442, #17810 ) ;
#13659 = AXIS2_PLACEMENT_3D ( 'NONE', #33508, #11353, #14161 ) ;
#13660 = CYLINDRICAL_SURFACE ( 'NONE', #22538, 2.000000000000001776 ) ;
#13661 = ORIENTED_EDGE ( 'NONE', *, *, #6407, .F. ) ;
#13662 = ORIENTED_EDGE ( 'NONE', *, *, #20660, .F. ) ;
#13663 = AXIS2_PLACEMENT_3D ( 'NONE', #29076, #14476, #28889 ) ;
#13664 = EDGE_CURVE ( 'NONE', #16153, #20325, #25703, .T. ) ;
#13665 = FACE_OUTER_BOUND ( 'NONE', #3117, .T. ) ;
#13666 = EDGE_LOOP ( 'NONE', ( #1289, #83, #18521, #892 ) ) ;
#13667 = CIRCLE ( 'NONE', #34637, 2.000000000000000000 ) ;
#13668 = AXIS2_PLACEMENT_3D ( 'NONE', #17804, #20993, #35267 ) ;
#13669 = DIRECTION ( 'NONE',  ( 0.000000000000000000, 0.000000000000000000, -1.000000000000000000 ) ) ;
#13670 = CARTESIAN_POINT ( 'NONE',  ( 3.000000000000000000, -2.201436576420045643, -1.270999999999998575 ) ) ;
#13671 = AXIS2_PLACEMENT_3D ( 'NONE', #14207, #25285, #25663 ) ;
#13672 = CARTESIAN_POINT ( 'NONE',  ( -35.19434990244938888, 52.39915983220783602, 12.49999999999999822 ) ) ;
#13673 = CIRCLE ( 'NONE', #19067, 2.000000000000001776 ) ;
#13674 = DIRECTION ( 'NONE',  ( 0.000000000000000000, 0.000000000000000000, 1.000000000000000000 ) ) ;
#13675 = CARTESIAN_POINT ( 'NONE',  ( 96.68603628058367860, -67.93726725791121623, 32.50000000000000711 ) ) ;
#13676 = DIRECTION ( 'NONE',  ( -1.000000000000000000, 0.000000000000000000, 0.000000000000000000 ) ) ;
#13677 = LINE ( 'NONE', #25476, #27381 ) ;
#13678 = CARTESIAN_POINT ( 'NONE',  ( 82.99999662536831124, -25.98076211353319565, -9.999999999999998224 ) ) ;
#13679 = ORIENTED_EDGE ( 'NONE', *, *, #16952, .T. ) ;
#13680 = VERTEX_POINT ( 'NONE', #27573 ) ;
#13681 = VECTOR ( 'NONE', #27996, 1000.000000000000000 ) ;
#13682 = DIRECTION ( 'NONE',  ( 0.000000000000000000, 0.000000000000000000, 1.000000000000000000 ) ) ;
#13683 = EDGE_CURVE ( 'NONE', #18775, #23924, #14911, .T. ) ;
#13684 = DIRECTION ( 'NONE',  ( -0.000000000000000000, -0.000000000000000000, -1.000000000000000000 ) ) ;
#13685 = DIRECTION ( 'NONE',  ( 0.000000000000000000, 0.000000000000000000, -1.000000000000000000 ) ) ;
#13686 = CARTESIAN_POINT ( 'NONE',  ( 52.39915983220795681, 35.19434990244919703, 12.49999999999999822 ) ) ;
#13687 = ORIENTED_EDGE ( 'NONE', *, *, #1217, .T. ) ;
#13688 = AXIS2_PLACEMENT_3D ( 'NONE', #14100, #23097, #17305 ) ;
#13689 = FACE_OUTER_BOUND ( 'NONE', #9245, .T. ) ;
#13690 = CIRCLE ( 'NONE', #34099, 2.000000000000001776 ) ;
#13691 = ORIENTED_EDGE ( 'NONE', *, *, #22232, .T. ) ;
#13692 = ORIENTED_EDGE ( 'NONE', *, *, #29414, .F. ) ;
#13693 = EDGE_CURVE ( 'NONE', #5473, #28380, #18756, .T. ) ;
#13694 = AXIS2_PLACEMENT_3D ( 'NONE', #12055, #26144, #31577 ) ;
#13695 = CARTESIAN_POINT ( 'NONE',  ( -48.00000337463109190, 51.96152422706637708, -9.999999999999998224 ) ) ;
#13696 = ORIENTED_EDGE ( 'NONE', *, *, #28820, .F. ) ;
#13697 = CARTESIAN_POINT ( 'NONE',  ( -55.00000337463109901, -60.62177826491083010, -9.999999999999998224 ) ) ;
#13698 = FACE_OUTER_BOUND ( 'NONE', #31335, .T. ) ;
#13699 = EDGE_CURVE ( 'NONE', #1955, #4119, #4505, .T. ) ;
#13700 = CIRCLE ( 'NONE', #35262, 2.000000000000000000 ) ;
#13701 = LINE ( 'NONE', #14050, #15488 ) ;
#13702 = CIRCLE ( 'NONE', #7120, 1.999999999999998224 ) ;
#13703 = VERTEX_POINT ( 'NONE', #1698 ) ;
#13704 = ORIENTED_EDGE ( 'NONE', *, *, #3656, .T. ) ;
#13705 = AXIS2_PLACEMENT_3D ( 'NONE', #36018, #10493, #4706 ) ;
#13706 = ORIENTED_EDGE ( 'NONE', *, *, #15550, .F. ) ;
#13707 = AXIS2_PLACEMENT_3D ( 'NONE', #31882, #26648, #3224 ) ;
#13708 = VERTEX_POINT ( 'NONE', #1878 ) ;
#13709 = DIRECTION ( 'NONE',  ( 0.000000000000000000, -1.000000000000000000, 1.034244904716769672E-15 ) ) ;
#13710 = CARTESIAN_POINT ( 'NONE',  ( 0.000000000000000000, 101.4480229402710734, 32.49999999999999289 ) ) ;
#13711 = DIRECTION ( 'NONE',  ( -1.000000000000000000, 0.000000000000000000, -0.000000000000000000 ) ) ;
#13712 = DIRECTION ( 'NONE',  ( 1.000000000000000000, 0.000000000000000000, 0.000000000000000000 ) ) ;
#13713 = CARTESIAN_POINT ( 'NONE',  ( 4.999999999999999112, 1.044517492640908651, -3.717833924169676507 ) ) ;
#13714 = ORIENTED_EDGE ( 'NONE', *, *, #32709, .F. ) ;
#13715 = DIRECTION ( 'NONE',  ( 1.000000000000000000, 0.000000000000000000, 0.000000000000000000 ) ) ;
#13716 = EDGE_CURVE ( 'NONE', #29194, #10781, #36189, .T. ) ;
#13717 = DIRECTION ( 'NONE',  ( 1.000000000000000000, 0.000000000000000000, 0.000000000000000000 ) ) ;
#13718 = CARTESIAN_POINT ( 'NONE',  ( -2.308176576174226117E-14, -5.999999999999947597, 32.50000000000000000 ) ) ;
#13719 = EDGE_LOOP ( 'NONE', ( #766, #14479 ) ) ;
#13720 = CARTESIAN_POINT ( 'NONE',  ( -20.39230267490738768, 84.64139243425341874, 12.50000000000000000 ) ) ;
#13721 = AXIS2_PLACEMENT_3D ( 'NONE', #22001, #13550, #27794 ) ;
#13722 = LINE ( 'NONE', #27769, #16575 ) ;
#13723 = ORIENTED_EDGE ( 'NONE', *, *, #934, .F. ) ;
#13724 = ADVANCED_FACE ( 'NONE', ( #19147 ), #36924, .F. ) ;
#13725 = ORIENTED_EDGE ( 'NONE', *, *, #31656, .T. ) ;
#13726 = DIRECTION ( 'NONE',  ( 0.000000000000000000, 0.000000000000000000, -1.000000000000000000 ) ) ;
#13727 = AXIS2_PLACEMENT_3D ( 'NONE', #24282, #24489, #6842 ) ;
#13728 = ADVANCED_FACE ( 'NONE', ( #22482 ), #13862, .F. ) ;
#13729 = DIRECTION ( 'NONE',  ( 0.000000000000000000, 0.000000000000000000, 1.000000000000000000 ) ) ;
#13730 = CARTESIAN_POINT ( 'NONE',  ( -62.00000337463108480, -51.96152422706641971, -5.000000000000000000 ) ) ;
#13731 = CARTESIAN_POINT ( 'NONE',  ( -0.4012132626380694456, -5.541862106709765534, -0.4203182062997422030 ) ) ;
#13732 = VERTEX_POINT ( 'NONE', #25858 ) ;
#13733 = ORIENTED_EDGE ( 'NONE', *, *, #37075, .T. ) ;
#13734 = VECTOR ( 'NONE', #16643, 1000.000000000000000 ) ;
#13735 = CARTESIAN_POINT ( 'NONE',  ( -68.00000000000000000, 0.000000000000000000, 12.49999999999999822 ) ) ;
#13736 = AXIS2_PLACEMENT_3D ( 'NONE', #6898, #18342, #15539 ) ;
#13737 = ORIENTED_EDGE ( 'NONE', *, *, #2811, .F. ) ;
#13738 = AXIS2_PLACEMENT_3D ( 'NONE', #24088, #7027, #35717 ) ;
#13739 = PLANE ( 'NONE',  #8208 ) ;
#13740 = ORIENTED_EDGE ( 'NONE', *, *, #20793, .F. ) ;
#13741 = ORIENTED_EDGE ( 'NONE', *, *, #35933, .T. ) ;
#13742 = AXIS2_PLACEMENT_3D ( 'NONE', #10156, #9952, #2056 ) ;
#13743 = DIRECTION ( 'NONE',  ( 1.000000000000000000, 0.000000000000000000, 0.000000000000000000 ) ) ;
#13744 = EDGE_CURVE ( 'NONE', #14529, #26415, #20286, .T. ) ;
#13745 = CIRCLE ( 'NONE', #37091, 2.000000000000001776 ) ;
#13746 = PLANE ( 'NONE',  #1704 ) ;
#13747 = ORIENTED_EDGE ( 'NONE', *, *, #28124, .T. ) ;
#13748 = ORIENTED_EDGE ( 'NONE', *, *, #1892, .F. ) ;
#13749 = DIRECTION ( 'NONE',  ( 0.000000000000000000, 0.4999999999999944489, 0.8660254037844418162 ) ) ;
#13750 = CIRCLE ( 'NONE', #4796, 3.000000000000004885 ) ;
#13751 = DIRECTION ( 'NONE',  ( 1.000000000000000000, 0.000000000000000000, 0.000000000000000000 ) ) ;
#13752 = LINE ( 'NONE', #4936, #10292 ) ;
#13753 = FACE_OUTER_BOUND ( 'NONE', #4093, .T. ) ;
#13754 = VERTEX_POINT ( 'NONE', #31821 ) ;
#13755 = DIRECTION ( 'NONE',  ( 1.000000000000000000, 0.000000000000000000, 0.000000000000000000 ) ) ;
#13756 =( REPRESENTATION_RELATIONSHIP ('NONE','NONE', #15268, #33015 ) REPRESENTATION_RELATIONSHIP_WITH_TRANSFORMATION ( #30488 )SHAPE_REPRESENTATION_RELATIONSHIP( ) );
#13757 = FACE_BOUND ( 'NONE', #20776, .T. ) ;
#13758 = CYLINDRICAL_SURFACE ( 'NONE', #4031, 2.000000000000001776 ) ;
#13759 = FACE_OUTER_BOUND ( 'NONE', #19125, .T. ) ;
#13760 = DIRECTION ( 'NONE',  ( 1.000000000000000000, 0.000000000000000000, 0.000000000000000000 ) ) ;
#13761 = AXIS2_PLACEMENT_3D ( 'NONE', #33839, #31375, #8520 ) ;
#13762 = DIRECTION ( 'NONE',  ( 0.000000000000000000, 0.000000000000000000, 1.000000000000000000 ) ) ;
#13763 = CIRCLE ( 'NONE', #25739, 150.0000000000000284 ) ;
#13764 = EDGE_CURVE ( 'NONE', #25525, #12740, #26282, .T. ) ;
#13765 = CARTESIAN_POINT ( 'NONE',  ( -2.000003374631327713, 86.60254037844397601, -9.999999999999998224 ) ) ;
#13766 = MECHANICAL_DESIGN_GEOMETRIC_PRESENTATION_REPRESENTATION (  '', ( #33559 ), #13173 ) ;
#13767 = CARTESIAN_POINT ( 'NONE',  ( 67.99999662536838230, 34.64101615137758472, -9.999999999999998224 ) ) ;
#13768 = VERTEX_POINT ( 'NONE', #28470 ) ;
#13769 = EDGE_CURVE ( 'NONE', #25339, #22877, #20405, .T. ) ;
#13770 = FACE_OUTER_BOUND ( 'NONE', #10391, .T. ) ;
#13771 = CARTESIAN_POINT ( 'NONE',  ( -70.00000337463099243, 17.32050807568877460, -5.000000000000000000 ) ) ;
#13772 = AXIS2_PLACEMENT_3D ( 'NONE', #22510, #27592, #7523 ) ;
#13773 = DIRECTION ( 'NONE',  ( 1.000000000000000000, 0.000000000000000000, 0.000000000000000000 ) ) ;
#13774 = ORIENTED_EDGE ( 'NONE', *, *, #24031, .T. ) ;
#13775 = ADVANCED_FACE ( 'NONE', ( #25308 ), #31462, .F. ) ;
#13776 = EDGE_LOOP ( 'NONE', ( #29999, #8417 ) ) ;
#13777 = VERTEX_POINT ( 'NONE', #8250 ) ;
#13778 = AXIS2_PLACEMENT_3D ( 'NONE', #35363, #32129, #29331 ) ;
#13779 = DIRECTION ( 'NONE',  ( -1.000000000000000000, 0.000000000000000000, -0.000000000000000000 ) ) ;
#13780 = FACE_OUTER_BOUND ( 'NONE', #7926, .T. ) ;
#13781 = EDGE_CURVE ( 'NONE', #10047, #25550, #29867, .T. ) ;
#13782 = AXIS2_PLACEMENT_3D ( 'NONE', #15687, #1614, #18688 ) ;
#13783 = VERTEX_POINT ( 'NONE', #28665 ) ;
#13784 = ADVANCED_FACE ( 'NONE', ( #3158 ), #28288, .F. ) ;
#13785 = DIRECTION ( 'NONE',  ( -1.000000000000000000, 0.000000000000000000, 0.000000000000000000 ) ) ;
#13786 = CARTESIAN_POINT ( 'NONE',  ( 101.4249800177814933, 31.43204461043894327, 32.50002500000000083 ) ) ;
#13787 = ORIENTED_EDGE ( 'NONE', *, *, #21790, .F. ) ;
#13788 = DIRECTION ( 'NONE',  ( 1.000000000000000000, 0.000000000000000000, 0.000000000000000000 ) ) ;
#13789 = ORIENTED_EDGE ( 'NONE', *, *, #1519, .T. ) ;
#13790 = CARTESIAN_POINT ( 'NONE',  ( -87.83969979969872099, -14.80603122773087499, 12.49999999999999645 ) ) ;
#13791 = AXIS2_PLACEMENT_3D ( 'NONE', #30182, #5060, #16697 ) ;
#13792 = EDGE_CURVE ( 'NONE', #8784, #29817, #10127, .T. ) ;
#13793 = EDGE_CURVE ( 'NONE', #32680, #28932, #8339, .T. ) ;
#13794 = CARTESIAN_POINT ( 'NONE',  ( -2.500000000000003997, 4.330127018922192761, -6.000000000000000000 ) ) ;
#13795 = DIRECTION ( 'NONE',  ( 1.000000000000000000, 0.000000000000000000, 0.000000000000000000 ) ) ;
#13796 = EDGE_CURVE ( 'NONE', #6148, #19879, #35878, .T. ) ;
#13797 = EDGE_CURVE ( 'NONE', #28577, #167, #528, .T. ) ;
#13798 = AXIS2_PLACEMENT_3D ( 'NONE', #3380, #2839, #8628 ) ;
#13799 = EDGE_CURVE ( 'NONE', #14564, #11272, #32266, .T. ) ;
#13800 = VERTEX_POINT ( 'NONE', #11769 ) ;
#13801 = DIRECTION ( 'NONE',  ( -0.000000000000000000, -0.000000000000000000, -1.000000000000000000 ) ) ;
#13802 = AXIS2_PLACEMENT_3D ( 'NONE', #32988, #10123, #15558 ) ;
#13803 = DIRECTION ( 'NONE',  ( 0.000000000000000000, 0.000000000000000000, 1.000000000000000000 ) ) ;
#13804 = CARTESIAN_POINT ( 'NONE',  ( 5.000000000000000000, 2.886751345948125991, -6.000000000000000000 ) ) ;
#13805 = ORIENTED_EDGE ( 'NONE', *, *, #11225, .F. ) ;
#13806 = CARTESIAN_POINT ( 'NONE',  ( 49.99999662536848177, -51.96152422706640550, 12.50000000000000000 ) ) ;
#13807 = DIRECTION ( 'NONE',  ( 1.000000000000000000, 0.000000000000000000, 0.000000000000000000 ) ) ;
#13808 = ORIENTED_EDGE ( 'NONE', *, *, #4159, .F. ) ;
#13809 = CARTESIAN_POINT ( 'NONE',  ( -80.00000337463094979, -17.32050807568882078, -5.000000000000000000 ) ) ;
#13810 = DIRECTION ( 'NONE',  ( -0.4999999999999979461, 0.8660254037844397068, 0.000000000000000000 ) ) ;
#13811 = PLANE ( 'NONE',  #31516 ) ;
#13812 = CARTESIAN_POINT ( 'NONE',  ( 79.99999662536833966, 34.64101615137759183, -5.000000000000000000 ) ) ;
#13813 = ORIENTED_EDGE ( 'NONE', *, *, #11225, .T. ) ;
#13814 = ORIENTED_EDGE ( 'NONE', *, *, #17665, .T. ) ;
#13815 = DIRECTION ( 'NONE',  ( -0.000000000000000000, -0.000000000000000000, 1.000000000000000000 ) ) ;
#13816 = CARTESIAN_POINT ( 'NONE',  ( -66.86787810013036903, 2.778182860042780700, 12.49999999999999645 ) ) ;
#13817 = ORIENTED_EDGE ( 'NONE', *, *, #33196, .F. ) ;
#13818 = ORIENTED_EDGE ( 'NONE', *, *, #21012, .T. ) ;
#13819 = CIRCLE ( 'NONE', #23403, 3.000000000000002665 ) ;
#13820 = CARTESIAN_POINT ( 'NONE',  ( 36.99999662536853862, 77.94228634059959404, -9.999999999999998224 ) ) ;
#13821 = DIRECTION ( 'NONE',  ( 0.000000000000000000, 0.000000000000000000, 1.000000000000000000 ) ) ;
#13822 = DIRECTION ( 'NONE',  ( 0.000000000000000000, 0.000000000000000000, -1.000000000000000000 ) ) ;
#13823 = ORIENTED_EDGE ( 'NONE', *, *, #27551, .F. ) ;
#13824 = ORIENTED_EDGE ( 'NONE', *, *, #607, .F. ) ;
#13825 = FACE_OUTER_BOUND ( 'NONE', #35146, .T. ) ;
#13826 = VERTEX_POINT ( 'NONE', #8432 ) ;
#13827 = LINE ( 'NONE', #36698, #1772 ) ;
#13828 = ORIENTED_EDGE ( 'NONE', *, *, #20870, .F. ) ;
#13829 = FACE_BOUND ( 'NONE', #5903, .T. ) ;
#13830 = EDGE_CURVE ( 'NONE', #27851, #34166, #334, .T. ) ;
#13831 = DIRECTION ( 'NONE',  ( 0.000000000000000000, 0.000000000000000000, 1.000000000000000000 ) ) ;
#13832 = ADVANCED_FACE ( 'NONE', ( #19861 ), #5441, .T. ) ;
#13833 = EDGE_LOOP ( 'NONE', ( #8270, #13704 ) ) ;
#13834 = DIRECTION ( 'NONE',  ( 0.000000000000000000, 0.000000000000000000, 1.000000000000000000 ) ) ;
#13835 = LINE ( 'NONE', #16655, #878 ) ;
#13836 = FACE_OUTER_BOUND ( 'NONE', #10597, .T. ) ;
#13837 = DIRECTION ( 'NONE',  ( -1.000000000000000000, -0.000000000000000000, -0.000000000000000000 ) ) ;
#13838 = AXIS2_PLACEMENT_3D ( 'NONE', #29749, #20756, #24137 ) ;
#13839 = ORIENTED_EDGE ( 'NONE', *, *, #17869, .F. ) ;
#13840 = DIRECTION ( 'NONE',  ( 1.000000000000000000, 0.000000000000000000, 0.000000000000000000 ) ) ;
#13841 = DIRECTION ( 'NONE',  ( 0.000000000000000000, 0.000000000000000000, -1.000000000000000000 ) ) ;
#13842 = DIRECTION ( 'NONE',  ( 1.000000000000000000, 0.000000000000000000, 0.000000000000000000 ) ) ;
#13843 = VERTEX_POINT ( 'NONE', #31657 ) ;
#13844 = EDGE_LOOP ( 'NONE', ( #391, #34050 ) ) ;
#13845 = ORIENTED_EDGE ( 'NONE', *, *, #7980, .F. ) ;
#13846 = DIRECTION ( 'NONE',  ( 0.000000000000000000, 0.000000000000000000, -1.000000000000000000 ) ) ;
#13847 = CARTESIAN_POINT ( 'NONE',  ( 4.279621169095998212, -62.97617850287780072, 12.49999999999999822 ) ) ;
#13848 = EDGE_CURVE ( 'NONE', #21808, #2177, #14324, .T. ) ;
#13849 = CARTESIAN_POINT ( 'NONE',  ( 69.99999662536839651, -17.32050807568879947, -5.000000000000000000 ) ) ;
#13850 = DIRECTION ( 'NONE',  ( -0.000000000000000000, -0.000000000000000000, 1.000000000000000000 ) ) ;
#13851 = FACE_OUTER_BOUND ( 'NONE', #35138, .T. ) ;
#13852 = LINE ( 'NONE', #7686, #4829 ) ;
#13853 = VECTOR ( 'NONE', #16691, 1000.000000000000000 ) ;
#13854 = CARTESIAN_POINT ( 'NONE',  ( 5.000000000000000000, 24.49489742783178414, 15.00000000000000000 ) ) ;
#13855 = DIRECTION ( 'NONE',  ( -1.000000000000000000, -0.000000000000000000, -0.000000000000000000 ) ) ;
#13856 = ORIENTED_EDGE ( 'NONE', *, *, #32785, .T. ) ;
#13857 = ORIENTED_EDGE ( 'NONE', *, *, #19494, .F. ) ;
#13858 = EDGE_CURVE ( 'NONE', #13783, #28708, #10712, .T. ) ;
#13859 = CARTESIAN_POINT ( 'NONE',  ( -65.00000337463102085, 43.30127018922198801, -9.999999999999998224 ) ) ;
#13860 = CARTESIAN_POINT ( 'NONE',  ( -33.99999999999945288, 58.88972745734214698, 12.49999999999999822 ) ) ;
#13861 = DIRECTION ( 'NONE',  ( 0.000000000000000000, 0.000000000000000000, 1.000000000000000000 ) ) ;
#13862 = CYLINDRICAL_SURFACE ( 'NONE', #16711, 2.000000000000001776 ) ;
#13863 = ORIENTED_EDGE ( 'NONE', *, *, #11445, .T. ) ;
#13864 = CARTESIAN_POINT ( 'NONE',  ( 4.999999999999999112, -0.2835658343809315252, -0.5205273423269578537 ) ) ;
#13865 = ORIENTED_EDGE ( 'NONE', *, *, #28798, .F. ) ;
#13866 = EDGE_LOOP ( 'NONE', ( #12092, #17520, #16801, #31332 ) ) ;
#13867 = EDGE_CURVE ( 'NONE', #29077, #7029, #21498, .T. ) ;
#13868 = CARTESIAN_POINT ( 'NONE',  ( 51.99999662536847467, -69.28203230275519786, -5.000000000000000000 ) ) ;
#13869 = ORIENTED_EDGE ( 'NONE', *, *, #31354, .F. ) ;
#13870 = SURFACE_SIDE_STYLE ('',( #9411 ) ) ;
#13871 = CARTESIAN_POINT ( 'NONE',  ( -2.500000000000000000, 3.061616997868383141E-16, -6.000000000000000000 ) ) ;
#13872 = DIRECTION ( 'NONE',  ( 1.000000000000000000, 0.000000000000000000, 0.000000000000000000 ) ) ;
#13873 = AXIS2_PLACEMENT_3D ( 'NONE', #37047, #23348, #34786 ) ;
#13874 = DIRECTION ( 'NONE',  ( 0.000000000000000000, 0.000000000000000000, 1.000000000000000000 ) ) ;
#13875 = ORIENTED_EDGE ( 'NONE', *, *, #25205, .F. ) ;
#13876 = ORIENTED_EDGE ( 'NONE', *, *, #12258, .F. ) ;
#13877 = CIRCLE ( 'NONE', #4307, 2.000000000000001776 ) ;
#13878 = VERTEX_POINT ( 'NONE', #32576 ) ;
#13879 = ORIENTED_EDGE ( 'NONE', *, *, #20715, .T. ) ;
#13880 = ORIENTED_EDGE ( 'NONE', *, *, #5589, .F. ) ;
#13881 = DIRECTION ( 'NONE',  ( -1.000000000000000000, 3.491481338843133750E-15, 0.000000000000000000 ) ) ;
#13882 = EDGE_CURVE ( 'NONE', #13165, #23444, #34092, .T. ) ;
#13883 = DIRECTION ( 'NONE',  ( 1.000000000000000000, 0.000000000000000000, 0.000000000000000000 ) ) ;
#13884 = DIRECTION ( 'NONE',  ( 1.000000000000000000, 0.000000000000000000, 0.000000000000000000 ) ) ;
#13885 = CARTESIAN_POINT ( 'NONE',  ( 4.999996625368645198, 77.94228634059957983, -9.999999999999998224 ) ) ;
#13886 = CARTESIAN_POINT ( 'NONE',  ( -111.8061974404900241, -19.22934205794863516, 32.50000000000000000 ) ) ;
#13887 = ADVANCED_FACE ( 'NONE', ( #24146 ), #14780, .F. ) ;
#13888 = ORIENTED_EDGE ( 'NONE', *, *, #35419, .F. ) ;
#13889 = CARTESIAN_POINT ( 'NONE',  ( 3.000000000000000000, -2.935248768560059229, 3.469446951953614189E-15 ) ) ;
#13890 = DIRECTION ( 'NONE',  ( 0.000000000000000000, 0.000000000000000000, 1.000000000000000000 ) ) ;
#13891 = DIRECTION ( 'NONE',  ( 0.000000000000000000, 0.000000000000000000, 1.000000000000000000 ) ) ;
#13892 = ORIENTED_EDGE ( 'NONE', *, *, #13764, .F. ) ;
#13893 = CARTESIAN_POINT ( 'NONE',  ( -80.00000337463094979, -17.32050807568882078, -9.999999999999998224 ) ) ;
#13894 = ADVANCED_FACE ( 'NONE', ( #6893 ), #26777, .F. ) ;
#13895 = CYLINDRICAL_SURFACE ( 'NONE', #14766, 3.000000000000000888 ) ;
#13896 = ORIENTED_EDGE ( 'NONE', *, *, #1607, .T. ) ;
#13897 = EDGE_LOOP ( 'NONE', ( #645, #27989, #14427, #28761 ) ) ;
#13898 = ADVANCED_FACE ( 'NONE', ( #29010 ), #35425, .F. ) ;
#13899 = FACE_OUTER_BOUND ( 'NONE', #6190, .T. ) ;
#13900 = AXIS2_PLACEMENT_3D ( 'NONE', #28357, #8498, #220 ) ;
#13901 = DIRECTION ( 'NONE',  ( 0.000000000000000000, 0.000000000000000000, 1.000000000000000000 ) ) ;
#13902 = CARTESIAN_POINT ( 'NONE',  ( -40.00000337463113453, 69.28203230275516944, -9.999999999999998224 ) ) ;
#13903 = CARTESIAN_POINT ( 'NONE',  ( -2.739742549670663330, -4.191711593333635300, -0.5197061503823270368 ) ) ;
#13904 = ORIENTED_EDGE ( 'NONE', *, *, #9928, .F. ) ;
#13905 = VERTEX_POINT ( 'NONE', #29762 ) ;
#13906 = CARTESIAN_POINT ( 'NONE',  ( 17.99999662536861678, -69.28203230275519786, -9.999999999999998224 ) ) ;
#13907 = EDGE_LOOP ( 'NONE', ( #20473, #10494, #32086, #20072, #17878 ) ) ;
#13908 = EDGE_CURVE ( 'NONE', #6626, #26576, #4754, .T. ) ;
#13909 = DIRECTION ( 'NONE',  ( -1.000000000000000000, 0.000000000000000000, -0.000000000000000000 ) ) ;
#13910 = VERTEX_POINT ( 'NONE', #6335 ) ;
#13911 = VERTEX_POINT ( 'NONE', #17583 ) ;
#13912 = VECTOR ( 'NONE', #35298, 1000.000000000000000 ) ;
#13913 = CIRCLE ( 'NONE', #23502, 95.00000000000001421 ) ;
#13914 = DIRECTION ( 'NONE',  ( 0.000000000000000000, 0.4999999999999953926, 0.8660254037844412611 ) ) ;
#13915 = CARTESIAN_POINT ( 'NONE',  ( -35.00000337463117717, -77.94228634059963667, -9.999999999999998224 ) ) ;
#13916 = ORIENTED_EDGE ( 'NONE', *, *, #2064, .T. ) ;
#13917 = ORIENTED_EDGE ( 'NONE', *, *, #25507, .F. ) ;
#13918 = LINE ( 'NONE', #10921, #8928 ) ;
#13919 = DIRECTION ( 'NONE',  ( 1.000000000000000000, 0.000000000000000000, 0.000000000000000000 ) ) ;
#13920 = ADVANCED_FACE ( 'NONE', ( #3545 ), #17774, .F. ) ;
#13921 = CARTESIAN_POINT ( 'NONE',  ( -2.000003374631327713, 86.60254037844397601, -5.000000000000000000 ) ) ;
#13922 = DIRECTION ( 'NONE',  ( 0.000000000000000000, 0.000000000000000000, 1.000000000000000000 ) ) ;
#13923 = VERTEX_POINT ( 'NONE', #21331 ) ;
#13924 = DIRECTION ( 'NONE',  ( -0.8660254037844449249, -0.4999999999999888978, 0.000000000000000000 ) ) ;
#13925 = VECTOR ( 'NONE', #34322, 1000.000000000000000 ) ;
#13926 = EDGE_CURVE ( 'NONE', #21384, #15883, #33498, .T. ) ;
#13927 = FACE_BOUND ( 'NONE', #25439, .T. ) ;
#13928 = DIRECTION ( 'NONE',  ( 0.000000000000000000, 0.000000000000000000, -1.000000000000000000 ) ) ;
#13929 = CARTESIAN_POINT ( 'NONE',  ( -6.216324218022825094E-15, 6.066067634115565710, -4.359491423763658169 ) ) ;
#13930 = DIRECTION ( 'NONE',  ( -1.000000000000000000, 0.000000000000000000, 0.000000000000000000 ) ) ;
#13931 = DIRECTION ( 'NONE',  ( 0.5000000000000038858, 0.8660254037844362651, 0.000000000000000000 ) ) ;
#13932 = CARTESIAN_POINT ( 'NONE',  ( -21.38228473677787278, 108.2013388413266739, 27.49998800000000188 ) ) ;
#13933 = FACE_OUTER_BOUND ( 'NONE', #8651, .T. ) ;
#13934 = ORIENTED_EDGE ( 'NONE', *, *, #10561, .F. ) ;
#13935 = CARTESIAN_POINT ( 'NONE',  ( -32.00000337463118427, 69.28203230275516944, -5.000000000000000000 ) ) ;
#13936 = ADVANCED_FACE ( 'NONE', ( #23417 ), #21146, .T. ) ;
#13937 = DIRECTION ( 'NONE',  ( 1.000000000000000000, 0.000000000000000000, 0.000000000000000000 ) ) ;
#13938 = FACE_OUTER_BOUND ( 'NONE', #33099, .T. ) ;
#13939 = ORIENTED_EDGE ( 'NONE', *, *, #5109, .F. ) ;
#13940 = VECTOR ( 'NONE', #16315, 1000.000000000000000 ) ;
#13941 = ORIENTED_EDGE ( 'NONE', *, *, #18751, .T. ) ;
#13942 = ORIENTED_EDGE ( 'NONE', *, *, #17790, .F. ) ;
#13943 = ADVANCED_FACE ( 'NONE', ( #6539 ), #12121, .F. ) ;
#13944 = LINE ( 'NONE', #5897, #31509 ) ;
#13945 = CARTESIAN_POINT ( 'NONE',  ( 46.99999662536851019, 77.94228634059959404, -9.999999999999998224 ) ) ;
#13946 = VERTEX_POINT ( 'NONE', #20769 ) ;
#13947 = DIRECTION ( 'NONE',  ( -0.000000000000000000, 0.000000000000000000, 1.000000000000000000 ) ) ;
#13948 = AXIS2_PLACEMENT_3D ( 'NONE', #1028, #3663, #15093 ) ;
#13949 = ORIENTED_EDGE ( 'NONE', *, *, #31388, .T. ) ;
#13950 = CARTESIAN_POINT ( 'NONE',  ( 17.74159560741759378, -112.6248466129485735, 32.50000000000000000 ) ) ;
#13951 = EDGE_LOOP ( 'NONE', ( #9899, #12038, #32192, #11471 ) ) ;
#13952 = DIRECTION ( 'NONE',  ( -0.5000000000000101030, -0.8660254037844328234, 0.000000000000000000 ) ) ;
#13953 = ORIENTED_EDGE ( 'NONE', *, *, #6102, .T. ) ;
#13954 = EDGE_CURVE ( 'NONE', #29027, #4235, #32295, .T. ) ;
#13955 = DIRECTION ( 'NONE',  ( -0.000000000000000000, 0.000000000000000000, -1.000000000000000000 ) ) ;
#13956 = DIRECTION ( 'NONE',  ( 0.000000000000000000, 0.000000000000000000, 1.000000000000000000 ) ) ;
#13957 = ORIENTED_EDGE ( 'NONE', *, *, #13231, .T. ) ;
#13958 = LINE ( 'NONE', #5368, #24893 ) ;
#13959 = CIRCLE ( 'NONE', #3176, 3.000000000000000000 ) ;
#13960 = ITEM_DEFINED_TRANSFORMATION ( 'NONE', 'NONE', #36934,  #21385 ) ;
#13961 = ADVANCED_FACE ( 'NONE', ( #15146 ), #36313, .F. ) ;
#13962 = LINE ( 'NONE', #25410, #17688 ) ;
#13963 = CARTESIAN_POINT ( 'NONE',  ( -101.4249800177810812, 31.43204461044035725, 32.50002500000000083 ) ) ;
#13964 = VERTEX_POINT ( 'NONE', #35784 ) ;
#13965 = CARTESIAN_POINT ( 'NONE',  ( -25.00000337463121980, -77.94228634059963667, -9.999999999999998224 ) ) ;
#13966 = LINE ( 'NONE', #10248, #14365 ) ;
#13968 = VERTEX_POINT ( 'NONE', #7278 ) ;
#13967 = EDGE_CURVE ( 'NONE', #27946, #25623, #36499, .T. ) ;
#13969 = DIRECTION ( 'NONE',  ( -0.000000000000000000, -0.000000000000000000, 1.000000000000000000 ) ) ;
#13970 = ADVANCED_FACE ( 'NONE', ( #29962 ), #21703, .F. ) ;
#13971 = DIRECTION ( 'NONE',  ( 0.000000000000000000, 0.4999999999999991118, -0.8660254037844391517 ) ) ;
#13972 = CARTESIAN_POINT ( 'NONE',  ( -5.236872748402766398, -8.269757189038523917E-14, -4.057689166958448723 ) ) ;
#13973 = DIRECTION ( 'NONE',  ( 0.000000000000000000, 0.000000000000000000, -1.000000000000000000 ) ) ;
#13974 = VECTOR ( 'NONE', #34238, 1000.000000000000000 ) ;
#13975 = ORIENTED_EDGE ( 'NONE', *, *, #20335, .F. ) ;
#13976 = CIRCLE ( 'NONE', #23559, 2.000000000000001776 ) ;
#13977 = ORIENTED_EDGE ( 'NONE', *, *, #24622, .T. ) ;
#13978 = CARTESIAN_POINT ( 'NONE',  ( 70.80619744049005249, 84.18124734178236679, 32.50000000000000000 ) ) ;
#13979 = CARTESIAN_POINT ( 'NONE',  ( -10.00000337463128730, 69.28203230275516944, -9.999999999999998224 ) ) ;
#13980 = AXIS2_PLACEMENT_3D ( 'NONE', #31599, #34073, #19984 ) ;
#13981 = VERTEX_POINT ( 'NONE', #36147 ) ;
#13982 = ORIENTED_EDGE ( 'NONE', *, *, #2930, .F. ) ;
#13983 = ADVANCED_FACE ( 'NONE', ( #27692 ), #21886, .F. ) ;
#13984 = CARTESIAN_POINT ( 'NONE',  ( -65.00000337463102085, 60.62177826491077326, 12.50000000000000000 ) ) ;
#13985 = CARTESIAN_POINT ( 'NONE',  ( 54.99999662536846046, -43.30127018922200222, 12.50000000000000000 ) ) ;
#13986 = DIRECTION ( 'NONE',  ( 0.000000000000000000, 0.000000000000000000, 1.000000000000000000 ) ) ;
#13987 = AXIS2_PLACEMENT_3D ( 'NONE', #990, #6434, #18225 ) ;
#13988 = ORIENTED_EDGE ( 'NONE', *, *, #24117, .F. ) ;
#13989 = EDGE_LOOP ( 'NONE', ( #3173, #19328 ) ) ;
#13990 = AXIS2_PLACEMENT_3D ( 'NONE', #32565, #6881, #1996 ) ;
#13991 = DIRECTION ( 'NONE',  ( 0.000000000000000000, 0.000000000000000000, 1.000000000000000000 ) ) ;
#13992 = CARTESIAN_POINT ( 'NONE',  ( -87.00000337463093558, 8.660254037844389075, -9.999999999999998224 ) ) ;
#13993 = VERTEX_POINT ( 'NONE', #7649 ) ;
#13994 = DIRECTION ( 'NONE',  ( 0.000000000000000000, 0.000000000000000000, 1.000000000000000000 ) ) ;
#13995 = VERTEX_POINT ( 'NONE', #19105 ) ;
#13996 = DIRECTION ( 'NONE',  ( 0.000000000000000000, 0.000000000000000000, 1.000000000000000000 ) ) ;
#13997 = ADVANCED_FACE ( 'NONE', ( #19274, #30529, #27524, #30131, #27875, #4848, #30690, #16278 ), #1650, .T. ) ;
#13998 = LINE ( 'NONE', #8398, #10743 ) ;
#13999 = MECHANICAL_DESIGN_GEOMETRIC_PRESENTATION_REPRESENTATION (  '', ( #28373 ), #6828 ) ;
#14000 = ADVANCED_FACE ( 'NONE', ( #10271 ), #33133, .F. ) ;
#14001 = VERTEX_POINT ( 'NONE', #1839 ) ;
#14002 = DIRECTION ( 'NONE',  ( 0.000000000000000000, 0.000000000000000000, 1.000000000000000000 ) ) ;
#14003 = DIRECTION ( 'NONE',  ( -1.000000000000000000, 0.000000000000000000, 0.000000000000000000 ) ) ;
#14004 = CARTESIAN_POINT ( 'NONE',  ( -37.50000000000000000, 103.4105893997321886, -19.99999999999999645 ) ) ;
#14005 = CARTESIAN_POINT ( 'NONE',  ( -3.499999999999991562, 55.00000000000000000, -5.000000000000000000 ) ) ;
#14006 = ORIENTED_EDGE ( 'NONE', *, *, #8278, .F. ) ;
#14007 = CARTESIAN_POINT ( 'NONE',  ( 49.99999662536846756, 51.96152422706637708, 12.50000000000000000 ) ) ;
#14008 = ADVANCED_FACE ( 'NONE', ( #13638 ), #24897, .F. ) ;
#14009 = CARTESIAN_POINT ( 'NONE',  ( 104.8061974404897683, -19.22934205795014151, 32.50000000000000000 ) ) ;
#14010 = DIRECTION ( 'NONE',  ( 0.000000000000000000, 0.000000000000000000, 1.000000000000000000 ) ) ;
#14011 = ORIENTED_EDGE ( 'NONE', *, *, #30968, .T. ) ;
#14012 = CIRCLE ( 'NONE', #34986, 2.000000000000001776 ) ;
#14013 = EDGE_LOOP ( 'NONE', ( #18163, #825 ) ) ;
#14014 = EDGE_LOOP ( 'NONE', ( #20090, #2731 ) ) ;
#14015 = DIRECTION ( 'NONE',  ( 0.000000000000000000, 0.000000000000000000, 1.000000000000000000 ) ) ;
#14016 = DIRECTION ( 'NONE',  ( 1.000000000000000000, 0.000000000000000000, 0.000000000000000000 ) ) ;
#14017 = EDGE_CURVE ( 'NONE', #4105, #21760, #28715, .T. ) ;
#14018 = VECTOR ( 'NONE', #24766, 1000.000000000000000 ) ;
#14019 = EDGE_CURVE ( 'NONE', #21235, #12727, #20314, .T. ) ;
#14020 = CARTESIAN_POINT ( 'NONE',  ( 71.99999662536839651, 17.32050807568879236, -9.999999999999998224 ) ) ;
#14021 = ADVANCED_FACE ( 'NONE', ( #10836 ), #32774, .F. ) ;
#14022 = AXIS2_PLACEMENT_3D ( 'NONE', #16896, #36771, #11073 ) ;
#14023 = ADVANCED_FACE ( 'NONE', ( #21530 ), #19641, .F. ) ;
#14024 = LINE ( 'NONE', #16855, #5683 ) ;
#14025 = CARTESIAN_POINT ( 'NONE',  ( 105.8340997644729953, -39.11257430625002485, 32.50000000000000000 ) ) ;
#14026 = CARTESIAN_POINT ( 'NONE',  ( -103.1654966073423481, -61.26087114250804433, 32.50000000000000000 ) ) ;
#14027 = DIRECTION ( 'NONE',  ( 0.000000000000000000, 0.4999999999999953926, 0.8660254037844412611 ) ) ;
#14028 = CYLINDRICAL_SURFACE ( 'NONE', #20842, 150.0000000000000284 ) ;
#14029 = ORIENTED_EDGE ( 'NONE', *, *, #29531, .F. ) ;
#14030 = EDGE_LOOP ( 'NONE', ( #9916, #8563, #35704, #21824, #822, #32360 ) ) ;
#14031 = CARTESIAN_POINT ( 'NONE',  ( -20.00000337463123756, -86.60254037844400443, 17.49999999999999645 ) ) ;
#14032 = CARTESIAN_POINT ( 'NONE',  ( 24.99999662536859546, -77.94228634059960825, -9.999999999999998224 ) ) ;
#14033 = DIRECTION ( 'NONE',  ( -0.000000000000000000, -0.000000000000000000, -1.000000000000000000 ) ) ;
#14034 = VECTOR ( 'NONE', #913, 1000.000000000000000 ) ;
#14035 = DIRECTION ( 'NONE',  ( 0.000000000000000000, -0.4999999999999996114, 0.8660254037844388186 ) ) ;
#14036 = VERTEX_POINT ( 'NONE', #8205 ) ;
#14037 = AXIS2_PLACEMENT_3D ( 'NONE', #17821, #32437, #29813 ) ;
#14038 = CARTESIAN_POINT ( 'NONE',  ( 74.99999662536836809, -8.660254037844401509, 17.49999999999999645 ) ) ;
#14039 = ORIENTED_EDGE ( 'NONE', *, *, #30749, .F. ) ;
#14040 = ORIENTED_EDGE ( 'NONE', *, *, #35022, .F. ) ;
#14041 = LINE ( 'NONE', #34138, #30977 ) ;
#14042 = VERTEX_POINT ( 'NONE', #31073 ) ;
#14043 =( NAMED_UNIT ( * ) SI_UNIT ( $, .STERADIAN. ) SOLID_ANGLE_UNIT ( ) );
#14044 = EDGE_CURVE ( 'NONE', #34700, #34695, #7156, .T. ) ;
#14045 = DIRECTION ( 'NONE',  ( 1.000000000000000000, 0.000000000000000000, 0.000000000000000000 ) ) ;
#14046 = AXIS2_PLACEMENT_3D ( 'NONE', #3170, #23799, #32408 ) ;
#14047 = CIRCLE ( 'NONE', #15855, 2.000000000000001776 ) ;
#14048 = FACE_OUTER_BOUND ( 'NONE', #28303, .T. ) ;
#14049 = CIRCLE ( 'NONE', #2685, 3.000000000000002665 ) ;
#14050 = CARTESIAN_POINT ( 'NONE',  ( 0.000000000000000000, 101.4832769781154127, 32.47964607176053420 ) ) ;
#14051 = VERTEX_POINT ( 'NONE', #14382 ) ;
#14052 = ORIENTED_EDGE ( 'NONE', *, *, #11932, .F. ) ;
#14053 = ORIENTED_EDGE ( 'NONE', *, *, #29637, .T. ) ;
#14054 = ORIENTED_EDGE ( 'NONE', *, *, #10352, .F. ) ;
#14055 = ORIENTED_EDGE ( 'NONE', *, *, #35550, .F. ) ;
#14057 = CARTESIAN_POINT ( 'NONE',  ( 77.99999662536833966, 34.64101615137759183, 12.50000000000000000 ) ) ;
#14056 = CIRCLE ( 'NONE', #20085, 5.000000000000000000 ) ;
#14058 = CARTESIAN_POINT ( 'NONE',  ( 39.99999662536853151, 69.28203230275518365, -5.000000000000000000 ) ) ;
#14059 = AXIS2_PLACEMENT_3D ( 'NONE', #28784, #5733, #34616 ) ;
#14060 = DIRECTION ( 'NONE',  ( 1.000000000000000000, 0.000000000000000000, 0.000000000000000000 ) ) ;
#14061 = FACE_OUTER_BOUND ( 'NONE', #17895, .T. ) ;
#14062 = CARTESIAN_POINT ( 'NONE',  ( -63.00000337463102085, 43.30127018922198801, -9.999999999999998224 ) ) ;
#14063 = VERTEX_POINT ( 'NONE', #2953 ) ;
#14064 = DIRECTION ( 'NONE',  ( -1.000000000000000000, -0.000000000000000000, -0.000000000000000000 ) ) ;
#14065 = CIRCLE ( 'NONE', #1511, 2.000000000000001776 ) ;
#14066 = DIRECTION ( 'NONE',  ( 0.000000000000000000, 0.000000000000000000, 1.000000000000000000 ) ) ;
#14067 = ADVANCED_FACE ( 'NONE', ( #11543 ), #19997, .F. ) ;
#14068 = DIRECTION ( 'NONE',  ( 0.000000000000000000, 0.000000000000000000, 1.000000000000000000 ) ) ;
#14069 = ORIENTED_EDGE ( 'NONE', *, *, #36634, .T. ) ;
#14070 = LINE ( 'NONE', #30957, #18474 ) ;
#14071 = CARTESIAN_POINT ( 'NONE',  ( 79.99999662536833966, -3.469446951953614189E-15, -9.999999999999998224 ) ) ;
#14072 = AXIS2_PLACEMENT_3D ( 'NONE', #4257, #15865, #33104 ) ;
#14073 = ORIENTED_EDGE ( 'NONE', *, *, #10709, .F. ) ;
#14074 = AXIS2_PLACEMENT_3D ( 'NONE', #9641, #6257, #32321 ) ;
#14075 = ORIENTED_EDGE ( 'NONE', *, *, #35614, .F. ) ;
#14076 = CARTESIAN_POINT ( 'NONE',  ( 106.7731239591682026, -98.28784258493070070, 32.55002500000000509 ) ) ;
#14077 = CARTESIAN_POINT ( 'NONE',  ( 0.03111943836865378732, 6.084399642271171693, -4.366192694417985187 ) ) ;
#14078 = DIRECTION ( 'NONE',  ( 1.000000000000000000, 0.000000000000000000, 0.000000000000000000 ) ) ;
#14079 = CARTESIAN_POINT ( 'NONE',  ( -55.27226924886181791, -77.26562141134519379, 32.50000000000000000 ) ) ;
#14080 = ORIENTED_EDGE ( 'NONE', *, *, #10131, .T. ) ;
#14081 = ORIENTED_EDGE ( 'NONE', *, *, #28772, .T. ) ;
#14082 = CARTESIAN_POINT ( 'NONE',  ( 34.99999662536855283, -60.62177826491080168, -9.999999999999998224 ) ) ;
#14083 = AXIS2_PLACEMENT_3D ( 'NONE', #27488, #4622, #33100 ) ;
#14084 = ORIENTED_EDGE ( 'NONE', *, *, #35075, .F. ) ;
#14085 = CIRCLE ( 'NONE', #24294, 3.500000000000003109 ) ;
#14086 = DIRECTION ( 'NONE',  ( 1.000000000000000000, 0.000000000000000000, -0.000000000000000000 ) ) ;
#14087 = ORIENTED_EDGE ( 'NONE', *, *, #8040, .F. ) ;
#14088 = EDGE_CURVE ( 'NONE', #13581, #22989, #17195, .T. ) ;
#14089 = AXIS2_PLACEMENT_3D ( 'NONE', #27690, #13433, #16641 ) ;
#14090 = ADVANCED_FACE ( 'NONE', ( #292 ), #25825, .T. ) ;
#14091 = ORIENTED_EDGE ( 'NONE', *, *, #19934, .F. ) ;
#14092 = AXIS2_PLACEMENT_3D ( 'NONE', #5935, #12072, #9486 ) ;
#14093 = DIRECTION ( 'NONE',  ( -0.000000000000000000, -0.8660254037844420383, -0.4999999999999941713 ) ) ;
#14094 = DIRECTION ( 'NONE',  ( 1.000000000000000000, 0.000000000000000000, 0.000000000000000000 ) ) ;
#14095 = FACE_BOUND ( 'NONE', #6627, .T. ) ;
#14096 = ORIENTED_EDGE ( 'NONE', *, *, #943, .T. ) ;
#14097 = ADVANCED_FACE ( 'NONE', ( #34439 ), #115, .F. ) ;
#14098 = EDGE_LOOP ( 'NONE', ( #14839, #7499 ) ) ;
#14099 = DIRECTION ( 'NONE',  ( 0.000000000000000000, 0.000000000000000000, -1.000000000000000000 ) ) ;
#14100 = CARTESIAN_POINT ( 'NONE',  ( 65.44550000000002399, 0.000000000000000000, 0.000000000000000000 ) ) ;
#14101 = AXIS2_PLACEMENT_3D ( 'NONE', #36843, #19246, #19608 ) ;
#14102 = CARTESIAN_POINT ( 'NONE',  ( -83.00000337463092137, -8.660254037844422825, 17.49999999999999645 ) ) ;
#14103 = AXIS2_PLACEMENT_3D ( 'NONE', #28059, #4832, #35964 ) ;
#14104 = CARTESIAN_POINT ( 'NONE',  ( 66.99999662536839651, 60.62177826491078747, -5.000000000000000000 ) ) ;
#14105 = ADVANCED_FACE ( 'NONE', ( #33703 ), #22997, .F. ) ;
#14106 = ORIENTED_EDGE ( 'NONE', *, *, #17558, .F. ) ;
#14107 = FACE_OUTER_BOUND ( 'NONE', #13626, .T. ) ;
#14108 = FACE_BOUND ( 'NONE', #4465, .T. ) ;
#14109 = DIRECTION ( 'NONE',  ( 0.000000000000000000, 0.000000000000000000, -1.000000000000000000 ) ) ;
#14110 = FACE_OUTER_BOUND ( 'NONE', #8109, .T. ) ;
#14111 = DIRECTION ( 'NONE',  ( 0.000000000000000000, 0.000000000000000000, 1.000000000000000000 ) ) ;
#14112 = DIRECTION ( 'NONE',  ( -1.000000000000000000, 0.000000000000000000, 0.000000000000000000 ) ) ;
#14113 = CARTESIAN_POINT ( 'NONE',  ( -2.000003374631327713, 86.60254037844397601, -9.999999999999998224 ) ) ;
#14114 = AXIS2_PLACEMENT_3D ( 'NONE', #36808, #31538, #2506 ) ;
#14115 = EDGE_CURVE ( 'NONE', #21277, #11692, #20187, .T. ) ;
#14116 = DIRECTION ( 'NONE',  ( -0.5000000000000006661, -0.8660254037844382635, 0.000000000000000000 ) ) ;
#14117 = ORIENTED_EDGE ( 'NONE', *, *, #10732, .T. ) ;
#14119 = CONICAL_SURFACE ( 'NONE', #18922, 6.726859516510129922, 1.221730476396047038 ) ;
#14118 = CARTESIAN_POINT ( 'NONE',  ( 74.99999662536835388, -43.30127018922199511, 12.50000000000000000 ) ) ;
#14120 = CYLINDRICAL_SURFACE ( 'NONE', #30295, 3.499999999999996003 ) ;
#14121 = FACE_OUTER_BOUND ( 'NONE', #33653, .T. ) ;
#14122 = CIRCLE ( 'NONE', #2756, 2.000000000000000000 ) ;
#14123 = AXIS2_PLACEMENT_3D ( 'NONE', #12170, #29263, #26831 ) ;
#14124 = ORIENTED_EDGE ( 'NONE', *, *, #8180, .T. ) ;
#14125 = CIRCLE ( 'NONE', #29695, 2.000000000000000000 ) ;
#14126 = ORIENTED_EDGE ( 'NONE', *, *, #16391, .F. ) ;
#14127 = AXIS2_PLACEMENT_3D ( 'NONE', #23208, #12102, #20388 ) ;
#14128 = VERTEX_POINT ( 'NONE', #11381 ) ;
#14129 = CARTESIAN_POINT ( 'NONE',  ( 70.47608876694671665, 59.13646009116074964, 12.49999999999999822 ) ) ;
#14130 = DIRECTION ( 'NONE',  ( 0.000000000000000000, 0.000000000000000000, -1.000000000000000000 ) ) ;
#14131 = VERTEX_POINT ( 'NONE', #22828 ) ;
#14132 = AXIS2_PLACEMENT_3D ( 'NONE', #25256, #27676, #30851 ) ;
#14133 = AXIS2_PLACEMENT_3D ( 'NONE', #9191, #36, #6036 ) ;
#14134 = DIRECTION ( 'NONE',  ( 0.000000000000000000, 0.000000000000000000, 1.000000000000000000 ) ) ;
#14135 = EDGE_LOOP ( 'NONE', ( #13501, #28157, #542, #34540 ) ) ;
#14136 = EDGE_CURVE ( 'NONE', #8997, #29480, #8009, .T. ) ;
#14137 = CARTESIAN_POINT ( 'NONE',  ( -4.242640687119282106, 4.242640687119296317, 32.50000000000000000 ) ) ;
#14138 = ORIENTED_EDGE ( 'NONE', *, *, #14171, .T. ) ;
#14139 = CARTESIAN_POINT ( 'NONE',  ( -85.00000337463092137, -8.660254037844422825, 17.49999999999999645 ) ) ;
#14140 = ORIENTED_EDGE ( 'NONE', *, *, #33593, .T. ) ;
#14141 = ORIENTED_EDGE ( 'NONE', *, *, #7039, .T. ) ;
#14142 = DIRECTION ( 'NONE',  ( 0.000000000000000000, 0.000000000000000000, 1.000000000000000000 ) ) ;
#14143 = CARTESIAN_POINT ( 'NONE',  ( 4.652319770550017886, -3.087484620012992398, -1.687189089856322655 ) ) ;
#14144 = AXIS2_PLACEMENT_3D ( 'NONE', #17655, #6609, #26655 ) ;
#14145 = ADVANCED_FACE ( 'NONE', ( #19448 ), #31613, .F. ) ;
#14146 = ORIENTED_EDGE ( 'NONE', *, *, #22910, .F. ) ;
#14147 = AXIS2_PLACEMENT_3D ( 'NONE', #5213, #16654, #33897 ) ;
#14148 = CYLINDRICAL_SURFACE ( 'NONE', #14672, 2.000000000000001776 ) ;
#14149 = VECTOR ( 'NONE', #36824, 1000.000000000000000 ) ;
#14150 = CIRCLE ( 'NONE', #16572, 2.000000000000001776 ) ;
#14151 = CONTEXT_DEPENDENT_SHAPE_REPRESENTATION ( #21417, #1104 ) ;
#14152 = VECTOR ( 'NONE', #35015, 1000.000000000000000 ) ;
#14153 = CIRCLE ( 'NONE', #29723, 2.999999999999999556 ) ;
#14154 = CARTESIAN_POINT ( 'NONE',  ( 71.99999662536841072, 51.96152422706640550, 12.50000000000000000 ) ) ;
#14155 = CARTESIAN_POINT ( 'NONE',  ( -35.00000337463116296, 60.62177826491077326, 12.50000000000000000 ) ) ;
#14156 = EDGE_CURVE ( 'NONE', #20671, #32894, #17381, .T. ) ;
#14157 = VERTEX_POINT ( 'NONE', #30870 ) ;
#14158 = DIRECTION ( 'NONE',  ( -1.000000000000000000, -0.000000000000000000, -0.000000000000000000 ) ) ;
#14159 = CARTESIAN_POINT ( 'NONE',  ( -83.47442710120355969, 31.09745072740822991, -4.999999999999997335 ) ) ;
#14160 = ORIENTED_EDGE ( 'NONE', *, *, #11737, .T. ) ;
#14161 = DIRECTION ( 'NONE',  ( 1.000000000000000000, 0.000000000000000000, 0.000000000000000000 ) ) ;
#14162 = DIRECTION ( 'NONE',  ( 1.000000000000000000, 0.000000000000000000, 0.000000000000000000 ) ) ;
#14163 = DIRECTION ( 'NONE',  ( -1.000000000000000000, 0.000000000000000000, 0.000000000000000000 ) ) ;
#14164 = DIRECTION ( 'NONE',  ( 0.000000000000000000, 0.000000000000000000, -1.000000000000000000 ) ) ;
#14165 = CIRCLE ( 'NONE', #29149, 2.000000000000001776 ) ;
#14166 = ORIENTED_EDGE ( 'NONE', *, *, #29935, .F. ) ;
#14167 = EDGE_LOOP ( 'NONE', ( #7741, #15233 ) ) ;
#14168 = FACE_OUTER_BOUND ( 'NONE', #1188, .T. ) ;
#14169 = CARTESIAN_POINT ( 'NONE',  ( -20.00000337463122690, 86.60254037844397601, 12.50000000000000000 ) ) ;
#14170 = CIRCLE ( 'NONE', #8766, 1.133333333332999793 ) ;
#14171 = EDGE_CURVE ( 'NONE', #35934, #33595, #23943, .T. ) ;
#14172 = EDGE_LOOP ( 'NONE', ( #28416, #11203, #14270, #20732 ) ) ;
#14173 = VERTEX_POINT ( 'NONE', #17002 ) ;
#14174 = AXIS2_PLACEMENT_3D ( 'NONE', #19473, #10856, #5427 ) ;
#14175 = CARTESIAN_POINT ( 'NONE',  ( 3.000000000000000000, 0.000000000000000000, 0.000000000000000000 ) ) ;
#14176 = DIRECTION ( 'NONE',  ( 1.000000000000000000, 0.000000000000000000, 0.000000000000000000 ) ) ;
#14177 = AXIS2_PLACEMENT_3D ( 'NONE', #8212, #16839, #19650 ) ;
#14178 = FACE_OUTER_BOUND ( 'NONE', #29218, .T. ) ;
#14179 = AXIS2_PLACEMENT_3D ( 'NONE', #9874, #4443, #32753 ) ;
#14180 = VERTEX_POINT ( 'NONE', #5206 ) ;
#14181 = EDGE_CURVE ( 'NONE', #4797, #10781, #13143, .T. ) ;
#14182 = ORIENTED_EDGE ( 'NONE', *, *, #16523, .F. ) ;
#14183 =( NAMED_UNIT ( * ) SI_UNIT ( $, .STERADIAN. ) SOLID_ANGLE_UNIT ( ) );
#14184 = AXIS2_PLACEMENT_3D ( 'NONE', #27113, #12856, #17954 ) ;
#14185 = CARTESIAN_POINT ( 'NONE',  ( -101.7384897088135887, 110.2237710830547286, 27.50000000000000000 ) ) ;
#14186 = ORIENTED_EDGE ( 'NONE', *, *, #19863, .F. ) ;
#14187 = EDGE_CURVE ( 'NONE', #5725, #31117, #13827, .T. ) ;
#14188 = DIRECTION ( 'NONE',  ( 0.000000000000000000, 0.000000000000000000, 1.000000000000000000 ) ) ;
#14189 = ORIENTED_EDGE ( 'NONE', *, *, #3696, .T. ) ;
#14190 = FACE_BOUND ( 'NONE', #25283, .T. ) ;
#14191 = AXIS2_PLACEMENT_3D ( 'NONE', #4332, #4515, #32447 ) ;
#14192 = CARTESIAN_POINT ( 'NONE',  ( -82.00000337463096400, -34.64101615137762025, -5.000000000000000000 ) ) ;
#14193 = CARTESIAN_POINT ( 'NONE',  ( -3.000000000000000888, 0.000000000000000000, -5.674599999999998090 ) ) ;
#14194 = VECTOR ( 'NONE', #21257, 1000.000000000000000 ) ;
#14195 = VERTEX_POINT ( 'NONE', #10996 ) ;
#14196 = AXIS2_PLACEMENT_3D ( 'NONE', #1440, #2190, #24528 ) ;
#14197 = DIRECTION ( 'NONE',  ( 1.000000000000000000, 0.000000000000000000, 0.000000000000000000 ) ) ;
#14198 = AXIS2_PLACEMENT_3D ( 'NONE', #10886, #22153, #19165 ) ;
#14199 = DIRECTION ( 'NONE',  ( -1.000000000000000000, 0.000000000000000000, 0.000000000000000000 ) ) ;
#14200 = EDGE_CURVE ( 'NONE', #15209, #19312, #31671, .T. ) ;
#14201 = AXIS2_PLACEMENT_3D ( 'NONE', #13212, #25218, #4786 ) ;
#14202 = DIRECTION ( 'NONE',  ( 0.000000000000000000, 0.000000000000000000, -1.000000000000000000 ) ) ;
#14203 = LINE ( 'NONE', #17211, #35891 ) ;
#14204 = VERTEX_POINT ( 'NONE', #29364 ) ;
#14205 = CARTESIAN_POINT ( 'NONE',  ( 64.99999662536839651, 60.62177826491078747, 12.50000000000000000 ) ) ;
#14206 = CYLINDRICAL_SURFACE ( 'NONE', #36226, 3.499999999999996003 ) ;
#14207 = CARTESIAN_POINT ( 'NONE',  ( 34.99999662536853862, 77.94228634059959404, -9.999999999999998224 ) ) ;
#14208 = DIRECTION ( 'NONE',  ( 1.000000000000000000, 0.000000000000000000, 0.000000000000000000 ) ) ;
#14209 = VECTOR ( 'NONE', #32535, 1000.000000000000000 ) ;
#14210 = VERTEX_POINT ( 'NONE', #34991 ) ;
#14211 = AXIS2_PLACEMENT_3D ( 'NONE', #32507, #6823, #23527 ) ;
#14212 = ORIENTED_EDGE ( 'NONE', *, *, #24723, .T. ) ;
#14213 = ORIENTED_EDGE ( 'NONE', *, *, #3410, .T. ) ;
#14214 = CARTESIAN_POINT ( 'NONE',  ( -63.00000337463102085, 25.98076211353317433, -9.999999999999998224 ) ) ;
#14215 = CIRCLE ( 'NONE', #26795, 2.000000000000001776 ) ;
#14216 = FACE_OUTER_BOUND ( 'NONE', #24253, .T. ) ;
#14217 = EDGE_CURVE ( 'NONE', #30663, #13265, #29716, .T. ) ;
#14218 = AXIS2_PLACEMENT_3D ( 'NONE', #6625, #27219, #12414 ) ;
#14219 = CARTESIAN_POINT ( 'NONE',  ( -52.00000337463109190, 51.96152422706637708, -9.999999999999998224 ) ) ;
#14220 = CARTESIAN_POINT ( 'NONE',  ( 78.56323661778957046, -72.23156435200252190, 32.50000000000000000 ) ) ;
#14221 = CYLINDRICAL_SURFACE ( 'NONE', #3165, 5.000000000000000000 ) ;
#14222 = EDGE_CURVE ( 'NONE', #35764, #22350, #23381, .T. ) ;
#14223 = LINE ( 'NONE', #29002, #36387 ) ;
#14224 = VECTOR ( 'NONE', #13629, 1000.000000000000000 ) ;
#14225 = AXIS2_PLACEMENT_3D ( 'NONE', #24258, #26901, #27247 ) ;
#14226 = LINE ( 'NONE', #3152, #35832 ) ;
#14227 = ORIENTED_EDGE ( 'NONE', *, *, #20197, .T. ) ;
#14228 = AXIS2_PLACEMENT_3D ( 'NONE', #24915, #6600, #27542 ) ;
#14229 = EDGE_CURVE ( 'NONE', #22833, #33342, #12537, .T. ) ;
#14230 = VERTEX_POINT ( 'NONE', #31955 ) ;
#14231 = CYLINDRICAL_SURFACE ( 'NONE', #27850, 2.000000000000001776 ) ;
#14232 = AXIS2_PLACEMENT_3D ( 'NONE', #20474, #32653, #35118 ) ;
#14233 = CARTESIAN_POINT ( 'NONE',  ( -56.56139351304917540, -61.87160258682602176, -5.000000000000000000 ) ) ;
#14234 = CARTESIAN_POINT ( 'NONE',  ( -2.000003374631334818, 69.28203230275516944, -9.999999999999998224 ) ) ;
#14235 = CARTESIAN_POINT ( 'NONE',  ( -50.00000337463109190, 51.96152422706637708, -9.999999999999998224 ) ) ;
#14236 = EDGE_CURVE ( 'NONE', #24803, #11966, #6557, .T. ) ;
#14237 = ORIENTED_EDGE ( 'NONE', *, *, #19104, .F. ) ;
#14238 = EDGE_CURVE ( 'NONE', #5952, #26437, #27514, .T. ) ;
#14239 = CIRCLE ( 'NONE', #13563, 2.000000000000001776 ) ;
#14240 = AXIS2_PLACEMENT_3D ( 'NONE', #24450, #16365, #30614 ) ;
#14241 = FACE_BOUND ( 'NONE', #6498, .T. ) ;
#14242 = ORIENTED_EDGE ( 'NONE', *, *, #11060, .T. ) ;
#14243 = VERTEX_POINT ( 'NONE', #20371 ) ;
#14244 = CARTESIAN_POINT ( 'NONE',  ( -63.00000337463106348, -60.62177826491083010, -9.999999999999998224 ) ) ;
#14245 = ORIENTED_EDGE ( 'NONE', *, *, #10561, .T. ) ;
#14246 = AXIS2_PLACEMENT_3D ( 'NONE', #31768, #23709, #15086 ) ;
#14247 = EDGE_CURVE ( 'NONE', #26162, #7932, #15526, .T. ) ;
#14248 =( NAMED_UNIT ( * ) PLANE_ANGLE_UNIT ( ) SI_UNIT ( $, .RADIAN. ) );
#14249 = CARTESIAN_POINT ( 'NONE',  ( 77.93337901593585570, 72.12093275448846441, 32.50001250000000397 ) ) ;
#14250 = EDGE_CURVE ( 'NONE', #35812, #16375, #34115, .T. ) ;
#14251 = CARTESIAN_POINT ( 'NONE',  ( 47.63139720814400846, -27.50000000000022737, -5.000000000000000888 ) ) ;
#14252 = EDGE_CURVE ( 'NONE', #13826, #36096, #33527, .T. ) ;
#14253 = CIRCLE ( 'NONE', #34632, 65.00000000000000000 ) ;
#14254 = DIRECTION ( 'NONE',  ( -1.000000000000000000, 0.000000000000000000, 0.000000000000000000 ) ) ;
#14255 = EDGE_CURVE ( 'NONE', #21994, #12226, #9553, .T. ) ;
#14256 = ORIENTED_EDGE ( 'NONE', *, *, #536, .T. ) ;
#14257 = EDGE_CURVE ( 'NONE', #32638, #33663, #20724, .T. ) ;
#14258 = ORIENTED_EDGE ( 'NONE', *, *, #6135, .T. ) ;
#14259 = AXIS2_PLACEMENT_3D ( 'NONE', #2882, #9043, #32075 ) ;
#14260 = EDGE_LOOP ( 'NONE', ( #30052, #24126 ) ) ;
#14261 = AXIS2_PLACEMENT_3D ( 'NONE', #20013, #2773, #16847 ) ;
#14262 = ORIENTED_EDGE ( 'NONE', *, *, #1951, .F. ) ;
#14263 = CIRCLE ( 'NONE', #10093, 3.500000000000003109 ) ;
#14264 = VERTEX_POINT ( 'NONE', #32362 ) ;
#14265 = LINE ( 'NONE', #17602, #19454 ) ;
#14266 = DIRECTION ( 'NONE',  ( 0.000000000000000000, 0.000000000000000000, 1.000000000000000000 ) ) ;
#14267 = CARTESIAN_POINT ( 'NONE',  ( -20.00000337463122690, 86.60254037844397601, -5.000000000000000000 ) ) ;
#14268 = CARTESIAN_POINT ( 'NONE',  ( 56.67878100130369035, -27.78182860042797131, 12.49999999999999822 ) ) ;
#14269 = CARTESIAN_POINT ( 'NONE',  ( 69.99999662536838230, -51.96152422706639840, -5.000000000000000000 ) ) ;
#14270 = ORIENTED_EDGE ( 'NONE', *, *, #34251, .F. ) ;
#14271 = DIRECTION ( 'NONE',  ( 0.000000000000000000, 0.000000000000000000, 1.000000000000000000 ) ) ;
#14272 = AXIS2_PLACEMENT_3D ( 'NONE', #33742, #5984, #5596 ) ;
#14273 = CARTESIAN_POINT ( 'NONE',  ( 74.30619744048946984, -84.18124734178287838, 27.50000000000000000 ) ) ;
#14274 = DIRECTION ( 'NONE',  ( 0.000000000000000000, 0.000000000000000000, 1.000000000000000000 ) ) ;
#14275 = ORIENTED_EDGE ( 'NONE', *, *, #26640, .T. ) ;
#14276 = DIRECTION ( 'NONE',  ( -0.8191520442889890230, 0.000000000000000000, -0.5735764363510501562 ) ) ;
#14277 = DIRECTION ( 'NONE',  ( -0.000000000000000000, -0.000000000000000000, 1.000000000000000000 ) ) ;
#14278 = AXIS2_PLACEMENT_3D ( 'NONE', #22655, #2585, #13840 ) ;
#14279 = ORIENTED_EDGE ( 'NONE', *, *, #12668, .F. ) ;
#14280 = VERTEX_POINT ( 'NONE', #34635 ) ;
#14281 = CARTESIAN_POINT ( 'NONE',  ( -85.00000337463092137, 8.660254037844389075, 12.50000000000000000 ) ) ;
#14282 = CIRCLE ( 'NONE', #33454, 2.000000000000001776 ) ;
#14283 = CARTESIAN_POINT ( 'NONE',  ( -85.00000337463092137, 25.98076211353317433, -5.000000000000000000 ) ) ;
#14284 = DIRECTION ( 'NONE',  ( 1.000000000000000000, 0.000000000000000000, -0.000000000000000000 ) ) ;
#14285 = CARTESIAN_POINT ( 'NONE',  ( -5.000000000000000888, -2.886751345948162406, -3.984345921091775100 ) ) ;
#14286 = ORIENTED_EDGE ( 'NONE', *, *, #31089, .F. ) ;
#14287 = VERTEX_POINT ( 'NONE', #17545 ) ;
#14288 = CIRCLE ( 'NONE', #31616, 2.000000000000001776 ) ;
#14289 = AXIS2_PLACEMENT_3D ( 'NONE', #5928, #8912, #11896 ) ;
#14290 = CARTESIAN_POINT ( 'NONE',  ( -6.000000000000000000, 0.000000000000000000, 32.50000000000000000 ) ) ;
#14291 = DIRECTION ( 'NONE',  ( 0.000000000000000000, 0.000000000000000000, 1.000000000000000000 ) ) ;
#14292 = VECTOR ( 'NONE', #35629, 1000.000000000000000 ) ;
#14293 = ORIENTED_EDGE ( 'NONE', *, *, #34418, .F. ) ;
#14294 = DIRECTION ( 'NONE',  ( 0.000000000000000000, 0.000000000000000000, 1.000000000000000000 ) ) ;
#14295 = ORIENTED_EDGE ( 'NONE', *, *, #5015, .T. ) ;
#14296 = CARTESIAN_POINT ( 'NONE',  ( 64.99999662536841072, 25.98076211353318854, 17.49999999999999645 ) ) ;
#14297 = AXIS2_PLACEMENT_3D ( 'NONE', #22922, #13922, #34550 ) ;
#14298 = DIRECTION ( 'NONE',  ( 0.000000000000000000, 0.000000000000000000, 1.000000000000000000 ) ) ;
#14299 = DIRECTION ( 'NONE',  ( 0.000000000000000000, -0.5000000000000013323, -0.8660254037844379305 ) ) ;
#14300 = CARTESIAN_POINT ( 'NONE',  ( 9.999996625368655856, -86.60254037844400443, -5.000000000000000000 ) ) ;
#14301 = EDGE_CURVE ( 'NONE', #20440, #33271, #30521, .T. ) ;
#14302 = ORIENTED_EDGE ( 'NONE', *, *, #9133, .T. ) ;
#14303 = ORIENTED_EDGE ( 'NONE', *, *, #34183, .T. ) ;
#14304 = FACE_OUTER_BOUND ( 'NONE', #21835, .T. ) ;
#14305 = DIRECTION ( 'NONE',  ( 0.000000000000000000, 0.000000000000000000, 1.000000000000000000 ) ) ;
#14306 = CARTESIAN_POINT ( 'NONE',  ( 54.99999662536844625, 60.62177826491077326, 12.50000000000000000 ) ) ;
#14307 = CARTESIAN_POINT ( 'NONE',  ( 2.930059260563441015, 4.081832189068400396, -3.399990250278760378E-15 ) ) ;
#14308 = EDGE_LOOP ( 'NONE', ( #2764, #1530 ) ) ;
#14309 = LINE ( 'NONE', #25759, #35145 ) ;
#14310 = VECTOR ( 'NONE', #13448, 1000.000000000000114 ) ;
#14311 = FACE_BOUND ( 'NONE', #12641, .T. ) ;
#14312 = AXIS2_PLACEMENT_3D ( 'NONE', #503, #28975, #29369 ) ;
#14313 = CYLINDRICAL_SURFACE ( 'NONE', #20225, 3.499999999999996003 ) ;
#14314 = LINE ( 'NONE', #19927, #26473 ) ;
#14315 = CARTESIAN_POINT ( 'NONE',  ( -5.000003374631307729, 77.94228634059957983, 12.50000000000000000 ) ) ;
#14316 = DIRECTION ( 'NONE',  ( 0.000000000000000000, 0.000000000000000000, -1.000000000000000000 ) ) ;
#14317 = DIRECTION ( 'NONE',  ( 1.000000000000000000, 0.000000000000000000, 0.000000000000000000 ) ) ;
#14318 = CIRCLE ( 'NONE', #2727, 2.000000000000001776 ) ;
#14319 = DIRECTION ( 'NONE',  ( -0.000000000000000000, -0.000000000000000000, 1.000000000000000000 ) ) ;
#14320 = VERTEX_POINT ( 'NONE', #14735 ) ;
#14321 = CARTESIAN_POINT ( 'NONE',  ( -53.00000337463110611, -43.30127018922202353, 12.50000000000000000 ) ) ;
#14322 = CARTESIAN_POINT ( 'NONE',  ( -5.000000000000000888, -2.886751345948150860, -0.5999999999999998668 ) ) ;
#14323 = CARTESIAN_POINT ( 'NONE',  ( 19.31922176934805435, 76.99660315353983719, 27.49999999999999645 ) ) ;
#14324 = CIRCLE ( 'NONE', #17908, 33.00000000000001421 ) ;
#14325 = ADVANCED_FACE ( 'NONE', ( #12087 ), #9289, .F. ) ;
#14326 = VERTEX_POINT ( 'NONE', #32160 ) ;
#14327 = ORIENTED_EDGE ( 'NONE', *, *, #32650, .F. ) ;
#14328 = AXIS2_PLACEMENT_3D ( 'NONE', #31252, #25828, #14555 ) ;
#14329 = ORIENTED_EDGE ( 'NONE', *, *, #21996, .F. ) ;
#14330 = CARTESIAN_POINT ( 'NONE',  ( -85.00000337463092137, 25.98076211353317433, 17.49999999999999645 ) ) ;
#14331 = CARTESIAN_POINT ( 'NONE',  ( -27.00000337463121625, -77.94228634059963667, 17.49999999999999645 ) ) ;
#14332 = CIRCLE ( 'NONE', #22123, 2.000000000000001776 ) ;
#14333 = DIRECTION ( 'NONE',  ( 0.000000000000000000, 0.000000000000000000, 1.000000000000000000 ) ) ;
#14334 = VERTEX_POINT ( 'NONE', #17933 ) ;
#14335 = LINE ( 'NONE', #20486, #20282 ) ;
#14336 = AXIS2_PLACEMENT_3D ( 'NONE', #21501, #26938, #1251 ) ;
#14337 = ORIENTED_EDGE ( 'NONE', *, *, #3506, .F. ) ;
#14338 = CARTESIAN_POINT ( 'NONE',  ( 69.99999662536838230, -51.96152422706639840, 12.50000000000000000 ) ) ;
#14339 = ORIENTED_EDGE ( 'NONE', *, *, #329, .T. ) ;
#14340 = AXIS2_PLACEMENT_3D ( 'NONE', #35253, #11971, #32010 ) ;
#14341 = CARTESIAN_POINT ( 'NONE',  ( 69.99999662536839651, -3.469446951953614189E-15, -9.999999999999998224 ) ) ;
#14342 = ORIENTED_EDGE ( 'NONE', *, *, #26290, .F. ) ;
#14343 = ORIENTED_EDGE ( 'NONE', *, *, #27737, .F. ) ;
#14344 = CYLINDRICAL_SURFACE ( 'NONE', #34561, 27.00000000000001066 ) ;
#14345 = CARTESIAN_POINT ( 'NONE',  ( -37.00000337463116296, -60.62177826491080168, 12.50000000000000000 ) ) ;
#14346 = CARTESIAN_POINT ( 'NONE',  ( 0.000000000000000000, 0.000000000000000000, 12.49999999999999822 ) ) ;
#14347 = EDGE_CURVE ( 'NONE', #10807, #30623, #6678, .T. ) ;
#14348 = ORIENTED_EDGE ( 'NONE', *, *, #1988, .F. ) ;
#14349 = CARTESIAN_POINT ( 'NONE',  ( 0.000000000000000000, 0.000000000000000000, 17.49999999999999645 ) ) ;
#14350 = ITEM_DEFINED_TRANSFORMATION ( 'NONE', 'NONE', #14147,  #21385 ) ;
#14351 = AXIS2_PLACEMENT_3D ( 'NONE', #15492, #14939, #6294 ) ;
#14352 = CARTESIAN_POINT ( 'NONE',  ( 0.3000000000000016542, 5.755839955992559655E-16, -4.700000000000000178 ) ) ;
#14353 = CARTESIAN_POINT ( 'NONE',  ( -8.000003374631281972, 86.60254037844397601, -9.999999999999998224 ) ) ;
#14354 = AXIS2_PLACEMENT_3D ( 'NONE', #16054, #32930, #30099 ) ;
#14355 = VERTEX_POINT ( 'NONE', #29527 ) ;
#14356 = DIRECTION ( 'NONE',  ( 0.8660254037844415942, 0.4999999999999949485, 0.000000000000000000 ) ) ;
#14357 = CARTESIAN_POINT ( 'NONE',  ( 3.000000000000000000, -2.629050547790028157E-15, -2.541999999999999815 ) ) ;
#14358 = ORIENTED_EDGE ( 'NONE', *, *, #33872, .F. ) ;
#14359 = CARTESIAN_POINT ( 'NONE',  ( 36.99999662536853862, 77.94228634059959404, -5.000000000000000000 ) ) ;
#14360 = CARTESIAN_POINT ( 'NONE',  ( 29.99999662536856349, 69.28203230275518365, 12.50000000000000000 ) ) ;
#14361 = AXIS2_PLACEMENT_3D ( 'NONE', #16719, #13509, #13325 ) ;
#14362 = DIRECTION ( 'NONE',  ( 0.000000000000000000, 0.000000000000000000, 1.000000000000000000 ) ) ;
#14363 = DIRECTION ( 'NONE',  ( 1.000000000000000000, 0.000000000000000000, 0.000000000000000000 ) ) ;
#14364 = EDGE_LOOP ( 'NONE', ( #5597, #25420, #852, #34766 ) ) ;
#14365 = VECTOR ( 'NONE', #21677, 1000.000000000000000 ) ;
#14366 = ADVANCED_FACE ( 'NONE', ( #3679 ), #15108, .F. ) ;
#14367 = ORIENTED_EDGE ( 'NONE', *, *, #7818, .F. ) ;
#14368 = CIRCLE ( 'NONE', #15543, 27.00000000000001421 ) ;
#14369 = DIRECTION ( 'NONE',  ( 0.000000000000000000, 0.000000000000000000, -1.000000000000000000 ) ) ;
#14370 = CARTESIAN_POINT ( 'NONE',  ( 1.301042606982605321E-15, 5.773502691896264416, -5.553418012614792509 ) ) ;
#14371 = EDGE_CURVE ( 'NONE', #1473, #10472, #12266, .T. ) ;
#14372 = ORIENTED_EDGE ( 'NONE', *, *, #13830, .F. ) ;
#14373 = ORIENTED_EDGE ( 'NONE', *, *, #8558, .T. ) ;
#14374 = CARTESIAN_POINT ( 'NONE',  ( -5.000000000000000000, 30.00000000000000355, 15.00000000000000000 ) ) ;
#14375 = ADVANCED_FACE ( 'NONE', ( #32529 ), #6846, .T. ) ;
#14376 = LINE ( 'NONE', #28797, #8674 ) ;
#14377 = CIRCLE ( 'NONE', #28127, 1.999999999999998224 ) ;
#14378 = EDGE_LOOP ( 'NONE', ( #35144, #25906 ) ) ;
#14379 = EDGE_CURVE ( 'NONE', #9986, #1659, #27477, .T. ) ;
#14380 = DIRECTION ( 'NONE',  ( 0.000000000000000000, 0.000000000000000000, 1.000000000000000000 ) ) ;
#14381 = ORIENTED_EDGE ( 'NONE', *, *, #30366, .T. ) ;
#14382 = CARTESIAN_POINT ( 'NONE',  ( 66.86787810013036903, -2.778182860042780700, -4.999999999999997335 ) ) ;
#14383 = ORIENTED_EDGE ( 'NONE', *, *, #24907, .T. ) ;
#14385 = AXIS2_PLACEMENT_3D ( 'NONE', #34874, #20055, #20596 ) ;
#14384 = PLANE ( 'NONE',  #36314 ) ;
#14386 = CARTESIAN_POINT ( 'NONE',  ( 9.999996625368618552, 69.28203230275516944, -9.999999999999998224 ) ) ;
#14387 = AXIS2_PLACEMENT_3D ( 'NONE', #23971, #12510, #35418 ) ;
#14388 = DIRECTION ( 'NONE',  ( 1.000000000000000000, 0.000000000000000000, 0.000000000000000000 ) ) ;
#14389 = EDGE_LOOP ( 'NONE', ( #33959, #26503 ) ) ;
#14390 = CARTESIAN_POINT ( 'NONE',  ( 70.80619744048955511, -84.18124734178292101, -26.00000000000000000 ) ) ;
#14391 = DIRECTION ( 'NONE',  ( 0.000000000000000000, 0.000000000000000000, -1.000000000000000000 ) ) ;
#14392 = EDGE_CURVE ( 'NONE', #20758, #34308, #16179, .T. ) ;
#14393 = DIRECTION ( 'NONE',  ( 0.000000000000000000, 0.000000000000000000, 1.000000000000000000 ) ) ;
#14394 = CARTESIAN_POINT ( 'NONE',  ( 57.99999662536844625, 34.64101615137759893, -9.999999999999998224 ) ) ;
#14395 = VERTEX_POINT ( 'NONE', #32924 ) ;
#14396 = CIRCLE ( 'NONE', #4241, 2.000000000000001776 ) ;
#14397 = DIRECTION ( 'NONE',  ( 1.000000000000000000, 0.000000000000000000, 0.000000000000000000 ) ) ;
#14398 = DIRECTION ( 'NONE',  ( 0.000000000000000000, 0.000000000000000000, -1.000000000000000000 ) ) ;
#14399 = DIRECTION ( 'NONE',  ( -1.000000000000000000, 0.000000000000000000, 0.000000000000000000 ) ) ;
#14400 = EDGE_CURVE ( 'NONE', #33302, #20878, #25152, .T. ) ;
#14401 = ORIENTED_EDGE ( 'NONE', *, *, #11211, .T. ) ;
#14402 = ORIENTED_EDGE ( 'NONE', *, *, #22616, .T. ) ;
#14403 = EDGE_CURVE ( 'NONE', #807, #24141, #29919, .T. ) ;
#14404 = AXIS2_PLACEMENT_3D ( 'NONE', #10130, #21564, #32994 ) ;
#14405 = ORIENTED_EDGE ( 'NONE', *, *, #5724, .F. ) ;
#14406 = AXIS2_PLACEMENT_3D ( 'NONE', #1944, #26905, #33074 ) ;
#14407 = CARTESIAN_POINT ( 'NONE',  ( 0.000000000000000000, 0.000000000000000000, 15.00000000000000000 ) ) ;
#14408 = CARTESIAN_POINT ( 'NONE',  ( 0.000000000000000000, 0.000000000000000000, 27.50000000000000000 ) ) ;
#14409 = FACE_OUTER_BOUND ( 'NONE', #11229, .T. ) ;
#14410 = CARTESIAN_POINT ( 'NONE',  ( 0.000000000000000000, 0.000000000000000000, 27.50000000000000000 ) ) ;
#14411 = DIRECTION ( 'NONE',  ( 0.000000000000000000, 0.000000000000000000, 1.000000000000000000 ) ) ;
#14412 = CARTESIAN_POINT ( 'NONE',  ( -5.000000000000000888, 3.130594094869389554, -4.027781427241076351 ) ) ;
#14413 = ORIENTED_EDGE ( 'NONE', *, *, #36266, .F. ) ;
#14414 = VERTEX_POINT ( 'NONE', #7240 ) ;
#14415 = DIRECTION ( 'NONE',  ( 0.000000000000000000, 0.000000000000000000, -1.000000000000000000 ) ) ;
#14416 = ADVANCED_FACE ( 'NONE', ( #33487 ), #12833, .F. ) ;
#14417 = DIRECTION ( 'NONE',  ( 0.000000000000000000, 0.000000000000000000, 1.000000000000000000 ) ) ;
#14418 = CARTESIAN_POINT ( 'NONE',  ( 14.99999662536863632, -77.94228634059960825, -5.000000000000000000 ) ) ;
#14419 = CARTESIAN_POINT ( 'NONE',  ( 69.99999662536839651, -3.469446951953614189E-15, -9.999999999999998224 ) ) ;
#14420 = ORIENTED_EDGE ( 'NONE', *, *, #9196, .F. ) ;
#14421 = PRODUCT_DEFINITION_CONTEXT ( 'detailed design', #20687, 'design' ) ;
#14422 = CARTESIAN_POINT ( 'NONE',  ( -90.00000337463090716, -1.040834085586084257E-14, -9.999999999999998224 ) ) ;
#14423 = VERTEX_POINT ( 'NONE', #4417 ) ;
#14424 = ORIENTED_EDGE ( 'NONE', *, *, #1222, .T. ) ;
#14425 = AXIS2_PLACEMENT_3D ( 'NONE', #24574, #32605, #18374 ) ;
#14426 = CARTESIAN_POINT ( 'NONE',  ( 1.653121499799246719, -4.819072548984012272, -5.948595712916168843 ) ) ;
#14427 = ORIENTED_EDGE ( 'NONE', *, *, #23854, .F. ) ;
#14428 = CARTESIAN_POINT ( 'NONE',  ( 69.99999662536839651, -17.32050807568879947, 17.49999999999999645 ) ) ;
#14429 = ADVANCED_FACE ( 'NONE', ( #35557, #7794, #27095, #22041, #13227, #10237, #7414, #21665, #32723, #30649, #36106, #21840, #10049, #21284 ), #33093, .F. ) ;
#14430 = FACE_BOUND ( 'NONE', #31366, .T. ) ;
#14431 = ORIENTED_EDGE ( 'NONE', *, *, #33084, .T. ) ;
#14432 = EDGE_CURVE ( 'NONE', #31374, #24444, #7050, .T. ) ;
#14433 = ORIENTED_EDGE ( 'NONE', *, *, #261, .T. ) ;
#14434 = ORIENTED_EDGE ( 'NONE', *, *, #33989, .F. ) ;
#14435 = EDGE_CURVE ( 'NONE', #3388, #5117, #31726, .T. ) ;
#14436 = ORIENTED_EDGE ( 'NONE', *, *, #8180, .F. ) ;
#14437 = ORIENTED_EDGE ( 'NONE', *, *, #22430, .F. ) ;
#14438 = DIRECTION ( 'NONE',  ( 0.000000000000000000, 0.000000000000000000, -1.000000000000000000 ) ) ;
#14439 = ADVANCED_FACE ( 'NONE', ( #1239 ), #12656, .F. ) ;
#14440 = DIRECTION ( 'NONE',  ( 0.000000000000000000, 0.000000000000000000, 1.000000000000000000 ) ) ;
#14441 = EDGE_CURVE ( 'NONE', #25326, #10648, #582, .T. ) ;
#14442 = AXIS2_PLACEMENT_3D ( 'NONE', #12928, #1493, #4705 ) ;
#14443 = DIRECTION ( 'NONE',  ( 0.000000000000000000, 0.4999999999999991118, -0.8660254037844391517 ) ) ;
#14444 = FACE_OUTER_BOUND ( 'NONE', #4211, .T. ) ;
#14445 = CARTESIAN_POINT ( 'NONE',  ( 68.17080445151383117, -51.15278694518232072, -5.000000000000000000 ) ) ;
#14446 = EDGE_CURVE ( 'NONE', #15915, #34006, #36290, .T. ) ;
#14447 = EDGE_LOOP ( 'NONE', ( #3999, #13391 ) ) ;
#14448 = DIRECTION ( 'NONE',  ( 1.000000000000000000, 0.000000000000000000, 0.000000000000000000 ) ) ;
#14449 = CARTESIAN_POINT ( 'NONE',  ( -44.13139720814380951, 27.50000000000055422, -10.00000000000000000 ) ) ;
#14450 = CARTESIAN_POINT ( 'NONE',  ( 49.99999662536846756, 69.28203230275516944, -9.999999999999998224 ) ) ;
#14451 = ORIENTED_EDGE ( 'NONE', *, *, #4561, .T. ) ;
#14452 = CARTESIAN_POINT ( 'NONE',  ( -40.00000337463113453, -69.28203230275519786, -9.999999999999998224 ) ) ;
#14453 = FACE_OUTER_BOUND ( 'NONE', #32127, .T. ) ;
#14454 = ADVANCED_FACE ( 'NONE', ( #16236 ), #1966, .F. ) ;
#14455 = ORIENTED_EDGE ( 'NONE', *, *, #23004, .F. ) ;
#14456 = EDGE_CURVE ( 'NONE', #30623, #9129, #34140, .T. ) ;
#14457 = ORIENTED_EDGE ( 'NONE', *, *, #4042, .T. ) ;
#14458 = DIRECTION ( 'NONE',  ( 1.000000000000000000, 0.000000000000000000, 0.000000000000000000 ) ) ;
#14459 = ADVANCED_FACE ( 'NONE', ( #28211 ), #8696, .F. ) ;
#14460 = CARTESIAN_POINT ( 'NONE',  ( -70.00000337463099243, 17.32050807568877460, -9.999999999999998224 ) ) ;
#14461 = DIRECTION ( 'NONE',  ( -0.000000000000000000, -0.000000000000000000, 1.000000000000000000 ) ) ;
#14462 =( REPRESENTATION_RELATIONSHIP ('NONE','NONE', #15268, #34443 ) REPRESENTATION_RELATIONSHIP_WITH_TRANSFORMATION ( #7976 )SHAPE_REPRESENTATION_RELATIONSHIP( ) );
#14463 = CARTESIAN_POINT ( 'NONE',  ( 64.99999662536841072, 25.98076211353318854, -5.000000000000000000 ) ) ;
#14464 = VERTEX_POINT ( 'NONE', #28574 ) ;
#14465 = ORIENTED_EDGE ( 'NONE', *, *, #11129, .T. ) ;
#14466 = LINE ( 'NONE', #14290, #29051 ) ;
#14467 = CYLINDRICAL_SURFACE ( 'NONE', #2788, 5.000000000000000888 ) ;
#14468 = DIRECTION ( 'NONE',  ( 1.000000000000000000, 0.000000000000000000, 0.000000000000000000 ) ) ;
#14469 = ORIENTED_EDGE ( 'NONE', *, *, #19168, .F. ) ;
#14470 = TOROIDAL_SURFACE ( 'NONE', #27037, 3.250000000000001332, 0.2500000000000000000 ) ;
#14471 = AXIS2_PLACEMENT_3D ( 'NONE', #11621, #23075, #8832 ) ;
#14472 = VERTEX_POINT ( 'NONE', #2355 ) ;
#14473 = VERTEX_POINT ( 'NONE', #36658 ) ;
#14474 = DIRECTION ( 'NONE',  ( 1.000000000000000000, 0.000000000000000000, 0.000000000000000000 ) ) ;
#14475 = EDGE_CURVE ( 'NONE', #21781, #807, #14377, .T. ) ;
#14476 = DIRECTION ( 'NONE',  ( 0.000000000000000000, 0.000000000000000000, 1.000000000000000000 ) ) ;
#14477 = ORIENTED_EDGE ( 'NONE', *, *, #29136, .T. ) ;
#14478 = ADVANCED_FACE ( 'NONE', ( #11337 ), #2703, .F. ) ;
#14479 = ORIENTED_EDGE ( 'NONE', *, *, #5104, .F. ) ;
#14480 = DIRECTION ( 'NONE',  ( -0.000000000000000000, -0.000000000000000000, 1.000000000000000000 ) ) ;
#14481 = CARTESIAN_POINT ( 'NONE',  ( -70.00000337463102085, -51.96152422706641971, -9.999999999999998224 ) ) ;
#14482 = DIRECTION ( 'NONE',  ( -1.000000000000000000, 0.000000000000000000, 0.000000000000000000 ) ) ;
#14483 = VERTEX_POINT ( 'NONE', #19952 ) ;
#14484 = DIRECTION ( 'NONE',  ( -1.000000000000000000, -0.000000000000000000, -0.000000000000000000 ) ) ;
#14485 = FACE_BOUND ( 'NONE', #7081, .T. ) ;
#14486 = ADVANCED_FACE ( 'NONE', ( #17145 ), #16955, .F. ) ;
#14487 = CARTESIAN_POINT ( 'NONE',  ( 4.279621169095998212, -62.97617850287780072, 12.49999999999999822 ) ) ;
#14488 = CARTESIAN_POINT ( 'NONE',  ( -31.09745072740852123, -83.47442710120344600, -5.000000000000011546 ) ) ;
#14489 = DIRECTION ( 'NONE',  ( 0.000000000000000000, 0.000000000000000000, 1.000000000000000000 ) ) ;
#14490 = DIRECTION ( 'NONE',  ( 0.000000000000000000, 0.000000000000000000, 1.000000000000000000 ) ) ;
#14491 = DIRECTION ( 'NONE',  ( 0.000000000000000000, 0.000000000000000000, -1.000000000000000000 ) ) ;
#14492 = CIRCLE ( 'NONE', #2533, 2.000000000000000000 ) ;
#14493 = DIRECTION ( 'NONE',  ( 1.000000000000000000, 0.000000000000000000, 0.000000000000000000 ) ) ;
#14494 = ORIENTED_EDGE ( 'NONE', *, *, #18888, .F. ) ;
#14495 = CARTESIAN_POINT ( 'NONE',  ( -47.00000337463111322, -77.94228634059960825, 17.49999999999999645 ) ) ;
#14496 = CARTESIAN_POINT ( 'NONE',  ( -0.4318028594007664034, 5.811705888748974758, -4.266911319714222550 ) ) ;
#14497 = DIRECTION ( 'NONE',  ( 1.000000000000000000, 0.000000000000000000, 0.000000000000000000 ) ) ;
#14498 = EDGE_CURVE ( 'NONE', #12006, #16632, #8964, .T. ) ;
#14499 = ORIENTED_EDGE ( 'NONE', *, *, #4652, .F. ) ;
#14500 = ADVANCED_FACE ( 'NONE', ( #5905 ), #22789, .F. ) ;
#14501 = EDGE_LOOP ( 'NONE', ( #10228, #21332, #11974, #24966 ) ) ;
#14502 = ORIENTED_EDGE ( 'NONE', *, *, #11020, .T. ) ;
#14503 = EDGE_CURVE ( 'NONE', #30697, #12872, #24560, .T. ) ;
#14504 = EDGE_CURVE ( 'NONE', #35512, #23824, #25786, .T. ) ;
#14505 = DIRECTION ( 'NONE',  ( 0.000000000000000000, 0.000000000000000000, -1.000000000000000000 ) ) ;
#14506 = DIRECTION ( 'NONE',  ( 1.000000000000000000, 0.000000000000000000, 0.000000000000000000 ) ) ;
#14507 = CARTESIAN_POINT ( 'NONE',  ( -87.00000337463093558, 8.660254037844389075, -5.000000000000000000 ) ) ;
#14508 = ORIENTED_EDGE ( 'NONE', *, *, #2880, .T. ) ;
#14509 = CARTESIAN_POINT ( 'NONE',  ( 35.19434990244975126, -52.39915983220758022, -49.22241343995298024 ) ) ;
#14510 = CIRCLE ( 'NONE', #14534, 2.000000000000001776 ) ;
#14511 = ORIENTED_EDGE ( 'NONE', *, *, #21585, .T. ) ;
#14512 = CARTESIAN_POINT ( 'NONE',  ( -22.49962511848374902, -105.9192538511173041, 32.50000000000000711 ) ) ;
#14513 = VERTEX_POINT ( 'NONE', #27827 ) ;
#14514 = CARTESIAN_POINT ( 'NONE',  ( -2.374207310413330682E-13, -68.00000000000000000, -49.86348611802629449 ) ) ;
#14515 = ORIENTED_EDGE ( 'NONE', *, *, #4924, .T. ) ;
#14516 = ORIENTED_EDGE ( 'NONE', *, *, #11837, .T. ) ;
#14517 = CARTESIAN_POINT ( 'NONE',  ( -56.52018970185234537, 35.83991598322119643, -49.22241343995295892 ) ) ;
#14518 = DIRECTION ( 'NONE',  ( 0.000000000000000000, 0.4999999999999959477, -0.8660254037844409281 ) ) ;
#14519 = VECTOR ( 'NONE', #25713, 1000.000000000000000 ) ;
#14520 = DIRECTION ( 'NONE',  ( -0.000000000000000000, -0.000000000000000000, 1.000000000000000000 ) ) ;
#14521 = ORIENTED_EDGE ( 'NONE', *, *, #33976, .F. ) ;
#14522 = DIRECTION ( 'NONE',  ( 0.000000000000000000, 0.000000000000000000, 1.000000000000000000 ) ) ;
#14523 = EDGE_CURVE ( 'NONE', #36951, #12099, #20338, .T. ) ;
#14524 = CARTESIAN_POINT ( 'NONE',  ( 37.50000000000000000, 103.4105893997321743, -19.99999999999999645 ) ) ;
#14525 = FACE_OUTER_BOUND ( 'NONE', #23691, .T. ) ;
#14526 = VERTEX_POINT ( 'NONE', #10954 ) ;
#14527 = DIRECTION ( 'NONE',  ( 0.000000000000000000, 0.000000000000000000, 1.000000000000000000 ) ) ;
#14528 = CARTESIAN_POINT ( 'NONE',  ( -32.50000000000025580, -56.29165124598836201, 12.49999999999999822 ) ) ;
#14529 = VERTEX_POINT ( 'NONE', #5360 ) ;
#14530 = LINE ( 'NONE', #34611, #21420 ) ;
#14531 = DIRECTION ( 'NONE',  ( 0.000000000000000000, 0.000000000000000000, 1.000000000000000000 ) ) ;
#14532 = LINE ( 'NONE', #20350, #4017 ) ;
#14533 = CARTESIAN_POINT ( 'NONE',  ( 35.99999999999999289, 0.000000000000000000, 0.000000000000000000 ) ) ;
#14534 = AXIS2_PLACEMENT_3D ( 'NONE', #3629, #31740, #17874 ) ;
#14535 = CARTESIAN_POINT ( 'NONE',  ( -35.00000337463116296, 60.62177826491077326, -9.999999999999998224 ) ) ;
#14536 = ORIENTED_EDGE ( 'NONE', *, *, #31220, .F. ) ;
#14537 = CYLINDRICAL_SURFACE ( 'NONE', #11733, 2.000000000000001776 ) ;
#14538 = DIRECTION ( 'NONE',  ( 1.000000000000000000, 0.000000000000000000, 0.000000000000000000 ) ) ;
#14539 = ORIENTED_EDGE ( 'NONE', *, *, #10722, .T. ) ;
#14540 = ORIENTED_EDGE ( 'NONE', *, *, #3671, .T. ) ;
#14541 = VERTEX_POINT ( 'NONE', #36484 ) ;
#14542 = CIRCLE ( 'NONE', #25337, 2.000000000000001776 ) ;
#14543 = EDGE_CURVE ( 'NONE', #13993, #21238, #9584, .T. ) ;
#14544 = DIRECTION ( 'NONE',  ( 1.000000000000000000, 0.000000000000000000, 0.000000000000000000 ) ) ;
#14545 = AXIS2_PLACEMENT_3D ( 'NONE', #28559, #8338, #26114 ) ;
#14546 = DIRECTION ( 'NONE',  ( 1.000000000000000000, 0.000000000000000000, 0.000000000000000000 ) ) ;
#14547 = PRODUCT_DEFINITION_SHAPE ( 'NONE', 'NONE',  #6997 ) ;
#14548 = CARTESIAN_POINT ( 'NONE',  ( -77.93343913441597692, 72.12058696850911588, 32.50002500000000083 ) ) ;
#14549 = ORIENTED_EDGE ( 'NONE', *, *, #10351, .F. ) ;
#14550 = DIRECTION ( 'NONE',  ( 0.000000000000000000, 0.000000000000000000, 1.000000000000000000 ) ) ;
#14551 = ORIENTED_EDGE ( 'NONE', *, *, #7392, .T. ) ;
#14552 = FACE_BOUND ( 'NONE', #18526, .T. ) ;
#14553 = AXIS2_PLACEMENT_3D ( 'NONE', #6790, #32477, #18052 ) ;
#14554 = CIRCLE ( 'NONE', #33106, 2.000000000000001776 ) ;
#14555 = DIRECTION ( 'NONE',  ( -1.000000000000000000, 0.000000000000000000, 0.000000000000000000 ) ) ;
#14556 = DIRECTION ( 'NONE',  ( 0.000000000000000000, 0.000000000000000000, 1.000000000000000000 ) ) ;
#14557 = DIRECTION ( 'NONE',  ( 1.000000000000000000, 0.000000000000000000, 0.000000000000000000 ) ) ;
#14558 = EDGE_CURVE ( 'NONE', #6052, #2614, #11138, .T. ) ;
#14559 = CARTESIAN_POINT ( 'NONE',  ( 3.851086116668511750E-13, -54.99999999999999289, -16.00000000000000000 ) ) ;
#14560 = CARTESIAN_POINT ( 'NONE',  ( -8.000003374631287301, 69.28203230275516944, 17.49999999999999645 ) ) ;
#14561 = CIRCLE ( 'NONE', #34355, 2.000000000000001776 ) ;
#14562 = DIRECTION ( 'NONE',  ( 1.000000000000000000, 0.000000000000000000, 0.000000000000000000 ) ) ;
#14563 = LINE ( 'NONE', #17557, #7167 ) ;
#14564 = VERTEX_POINT ( 'NONE', #37033 ) ;
#14565 = DIRECTION ( 'NONE',  ( -1.000000000000000000, 0.000000000000000000, -0.000000000000000000 ) ) ;
#14566 = EDGE_CURVE ( 'NONE', #6228, #10748, #26661, .T. ) ;
#14567 = CARTESIAN_POINT ( 'NONE',  ( -38.00000337463113453, -69.28203230275519786, 17.49999999999999645 ) ) ;
#14568 = LINE ( 'NONE', #31802, #27911 ) ;
#14569 = VERTEX_POINT ( 'NONE', #34774 ) ;
#14570 = EDGE_CURVE ( 'NONE', #34992, #18360, #2394, .T. ) ;
#14571 = EDGE_LOOP ( 'NONE', ( #3554, #1197, #36895, #34108 ) ) ;
#14572 = VERTEX_POINT ( 'NONE', #20327 ) ;
#14573 = AXIS2_PLACEMENT_3D ( 'NONE', #21227, #6987, #30603 ) ;
#14574 = AXIS2_PLACEMENT_3D ( 'NONE', #29397, #1091, #23976 ) ;
#14575 = CYLINDRICAL_SURFACE ( 'NONE', #22818, 2.000000000000001776 ) ;
#14576 = EDGE_CURVE ( 'NONE', #22036, #17723, #7797, .T. ) ;
#14577 = DIRECTION ( 'NONE',  ( -1.000000000000000000, 0.000000000000000000, 0.000000000000000000 ) ) ;
#14578 = DIRECTION ( 'NONE',  ( 1.000000000000000000, 0.000000000000000000, 0.000000000000000000 ) ) ;
#14579 = CARTESIAN_POINT ( 'NONE',  ( 0.000000000000000000, 0.000000000000000000, -10.00000000000000000 ) ) ;
#14580 = CARTESIAN_POINT ( 'NONE',  ( 32.16008401677996886, 61.25926521283068382, 12.49999999999999645 ) ) ;
#14581 = ORIENTED_EDGE ( 'NONE', *, *, #32367, .F. ) ;
#14582 = AXIS2_PLACEMENT_3D ( 'NONE', #34738, #28887, #3409 ) ;
#14583 = EDGE_LOOP ( 'NONE', ( #19347, #1311, #3059, #28096 ) ) ;
#14584 = DIRECTION ( 'NONE',  ( 0.000000000000000000, 0.000000000000000000, 1.000000000000000000 ) ) ;
#14585 = AXIS2_PLACEMENT_3D ( 'NONE', #2472, #36967, #6023 ) ;
#14586 = CARTESIAN_POINT ( 'NONE',  ( -82.00000337463094979, 17.32050807568878525, -9.999999999999998224 ) ) ;
#14587 = CARTESIAN_POINT ( 'NONE',  ( -45.00000337463112743, -60.62177826491080168, 12.50000000000000000 ) ) ;
#14588 = ORIENTED_EDGE ( 'NONE', *, *, #11218, .T. ) ;
#14589 = CIRCLE ( 'NONE', #8602, 27.00000000000001421 ) ;
#14590 = ADVANCED_FACE ( 'NONE', ( #23891 ), #29313, .F. ) ;
#14591 = FACE_BOUND ( 'NONE', #22829, .T. ) ;
#14592 = EDGE_LOOP ( 'NONE', ( #24001, #9910, #22654, #17504 ) ) ;
#14593 = VERTEX_POINT ( 'NONE', #20879 ) ;
#14594 = EDGE_CURVE ( 'NONE', #23996, #16004, #1206, .T. ) ;
#14595 = CARTESIAN_POINT ( 'NONE',  ( -25.00000337463120914, 77.94228634059957983, 12.50000000000000000 ) ) ;
#14596 = EDGE_LOOP ( 'NONE', ( #4338, #34626, #25003 ) ) ;
#14597 = EDGE_CURVE ( 'NONE', #5465, #19466, #26337, .T. ) ;
#14598 = AXIS2_PLACEMENT_3D ( 'NONE', #26017, #26214, #34469 ) ;
#14599 = CARTESIAN_POINT ( 'NONE',  ( -80.00000337463094979, -2.428612866367529932E-14, 12.50000000000000000 ) ) ;
#14600 = DIRECTION ( 'NONE',  ( 1.000000000000000000, 0.000000000000000000, -0.000000000000000000 ) ) ;
#14601 = ORIENTED_EDGE ( 'NONE', *, *, #6854, .T. ) ;
#14602 = ORIENTED_EDGE ( 'NONE', *, *, #13764, .T. ) ;
#14603 = EDGE_CURVE ( 'NONE', #3447, #3051, #8387, .T. ) ;
#14604 = ORIENTED_EDGE ( 'NONE', *, *, #9391, .T. ) ;
#14605 = VECTOR ( 'NONE', #7333, 1000.000000000000000 ) ;
#14606 = VERTEX_POINT ( 'NONE', #31912 ) ;
#14607 = ADVANCED_FACE ( 'NONE', ( #999 ), #26326, .F. ) ;
#14608 = ORIENTED_EDGE ( 'NONE', *, *, #14703, .F. ) ;
#14609 = LINE ( 'NONE', #23437, #16453 ) ;
#14610 = CIRCLE ( 'NONE', #26603, 24.99999999999999289 ) ;
#14611 = DIRECTION ( 'NONE',  ( 0.000000000000000000, 0.000000000000000000, 1.000000000000000000 ) ) ;
#14612 = DIRECTION ( 'NONE',  ( -0.000000000000000000, -0.000000000000000000, 1.000000000000000000 ) ) ;
#14613 = CYLINDRICAL_SURFACE ( 'NONE', #36101, 2.000000000000001776 ) ;
#14614 = CARTESIAN_POINT ( 'NONE',  ( -70.00000337463099243, -2.428612866367529932E-14, 12.50000000000000000 ) ) ;
#14615 = ORIENTED_EDGE ( 'NONE', *, *, #9099, .T. ) ;
#14616 = CARTESIAN_POINT ( 'NONE',  ( -74.30619744048887299, 84.18124734178336155, 32.50000000000000000 ) ) ;
#14617 = DIRECTION ( 'NONE',  ( 0.000000000000000000, 0.000000000000000000, -1.000000000000000000 ) ) ;
#14618 = PLANE ( 'NONE',  #6239 ) ;
#14619 = ORIENTED_EDGE ( 'NONE', *, *, #11287, .F. ) ;
#14620 = DIRECTION ( 'NONE',  ( 1.000000000000000000, 0.000000000000000000, 0.000000000000000000 ) ) ;
#14621 = DIRECTION ( 'NONE',  ( 1.000000000000000000, 0.000000000000000000, 0.000000000000000000 ) ) ;
#14622 = ORIENTED_EDGE ( 'NONE', *, *, #6710, .F. ) ;
#14623 = CIRCLE ( 'NONE', #17592, 3.000000000000002665 ) ;
#14624 = ORIENTED_EDGE ( 'NONE', *, *, #27065, .T. ) ;
#14625 = ADVANCED_FACE ( 'NONE', ( #29118 ), #634, .F. ) ;
#14626 = CARTESIAN_POINT ( 'NONE',  ( -4.220252828340121276, -79.78402168683115292, 12.50000000000000000 ) ) ;
#14627 = CARTESIAN_POINT ( 'NONE',  ( 0.000000000000000000, 0.000000000000000000, -5.000000000000000000 ) ) ;
#14628 = CARTESIAN_POINT ( 'NONE',  ( 74.30619744048946984, -84.18124734178287838, 32.50000000000000000 ) ) ;
#14629 = FACE_OUTER_BOUND ( 'NONE', #30597, .T. ) ;
#14630 = ORIENTED_EDGE ( 'NONE', *, *, #8054, .T. ) ;
#14631 = CIRCLE ( 'NONE', #18857, 2.000000000000001776 ) ;
#14632 = CARTESIAN_POINT ( 'NONE',  ( 69.99999662536839651, -3.469446951953614189E-15, -9.999999999999998224 ) ) ;
#14633 = ADVANCED_FACE ( 'NONE', ( #34944 ), #32107, .T. ) ;
#14634 = DIRECTION ( 'NONE',  ( 0.000000000000000000, 0.000000000000000000, 1.000000000000000000 ) ) ;
#14635 = VECTOR ( 'NONE', #1658, 1000.000000000000000 ) ;
#14636 = CARTESIAN_POINT ( 'NONE',  ( -74.30619744048887299, 84.18124734178336155, 27.50000000000000000 ) ) ;
#14637 = CIRCLE ( 'NONE', #31985, 2.000000000000001776 ) ;
#14638 = ORIENTED_EDGE ( 'NONE', *, *, #17223, .T. ) ;
#14639 = EDGE_CURVE ( 'NONE', #12147, #6042, #35141, .T. ) ;
#14640 = CARTESIAN_POINT ( 'NONE',  ( 3.000000000000000000, 2.935248768560057453, -3.903127820947815962E-15 ) ) ;
#14641 = ORIENTED_EDGE ( 'NONE', *, *, #8729, .F. ) ;
#14642 = DIRECTION ( 'NONE',  ( -1.000000000000000000, 0.000000000000000000, 0.000000000000000000 ) ) ;
#14643 = DIRECTION ( 'NONE',  ( -0.000000000000000000, -0.000000000000000000, 1.000000000000000000 ) ) ;
#14644 = CIRCLE ( 'NONE', #2068, 2.000000000000001776 ) ;
#14645 = LINE ( 'NONE', #764, #1674 ) ;
#14646 = ORIENTED_EDGE ( 'NONE', *, *, #536, .F. ) ;
#14647 = CIRCLE ( 'NONE', #31971, 2.000000000000001776 ) ;
#14648 = ORIENTED_EDGE ( 'NONE', *, *, #22469, .T. ) ;
#14649 = DIRECTION ( 'NONE',  ( -1.000000000000000000, 0.000000000000000000, 0.000000000000000000 ) ) ;
#14650 = DIRECTION ( 'NONE',  ( 1.000000000000000000, 0.000000000000000000, 0.000000000000000000 ) ) ;
#14651 = DIRECTION ( 'NONE',  ( 0.000000000000000000, 0.000000000000000000, -1.000000000000000000 ) ) ;
#14652 = CIRCLE ( 'NONE', #872, 2.000000000000001776 ) ;
#14653 = EDGE_CURVE ( 'NONE', #8095, #6666, #4513, .T. ) ;
#14654 = ORIENTED_EDGE ( 'NONE', *, *, #4506, .F. ) ;
#14655 = DIRECTION ( 'NONE',  ( 1.000000000000000000, 0.000000000000000000, 0.000000000000000000 ) ) ;
#14656 = FACE_BOUND ( 'NONE', #1466, .T. ) ;
#14657 = FACE_OUTER_BOUND ( 'NONE', #25871, .T. ) ;
#14658 = DIRECTION ( 'NONE',  ( 1.000000000000000000, 0.000000000000000000, 0.000000000000000000 ) ) ;
#14659 = CARTESIAN_POINT ( 'NONE',  ( -30.00000337463119848, -69.28203230275522628, -9.999999999999998224 ) ) ;
#14660 = DIRECTION ( 'NONE',  ( 1.000000000000000000, 0.000000000000000000, 0.000000000000000000 ) ) ;
#14661 = AXIS2_PLACEMENT_3D ( 'NONE', #36349, #10659, #22102 ) ;
#14662 = AXIS2_PLACEMENT_3D ( 'NONE', #25792, #86, #5913 ) ;
#14663 = CARTESIAN_POINT ( 'NONE',  ( 74.30619744049005249, 84.18124734178236679, 32.50000000000000000 ) ) ;
#14664 = EDGE_LOOP ( 'NONE', ( #16407, #26182, #20410, #22311 ) ) ;
#14665 = CARTESIAN_POINT ( 'NONE',  ( 74.99999662536835388, -43.30127018922199511, 17.49999999999999645 ) ) ;
#14666 = CARTESIAN_POINT ( 'NONE',  ( 42.97377950131529190, 96.90768712682505281, 27.49999999999999645 ) ) ;
#14667 = CARTESIAN_POINT ( 'NONE',  ( -10.00000337463128197, 86.60254037844397601, -5.000000000000000000 ) ) ;
#14668 = ORIENTED_EDGE ( 'NONE', *, *, #27072, .F. ) ;
#14669 = ORIENTED_EDGE ( 'NONE', *, *, #4373, .T. ) ;
#14670 = ADVANCED_FACE ( 'NONE', ( #19319 ), #18761, .F. ) ;
#14671 = VERTEX_POINT ( 'NONE', #7700 ) ;
#14672 = AXIS2_PLACEMENT_3D ( 'NONE', #33849, #8161, #33257 ) ;
#14673 = DIRECTION ( 'NONE',  ( -0.000000000000000000, -0.000000000000000000, 1.000000000000000000 ) ) ;
#14674 = DIRECTION ( 'NONE',  ( 1.000000000000000000, 0.000000000000000000, 0.000000000000000000 ) ) ;
#14675 = EDGE_CURVE ( 'NONE', #18489, #15126, #7208, .T. ) ;
#14676 = AXIS2_PLACEMENT_3D ( 'NONE', #30071, #4781, #9823 ) ;
#14677 = DIRECTION ( 'NONE',  ( 1.000000000000000000, 0.000000000000000000, 0.000000000000000000 ) ) ;
#14678 = EDGE_LOOP ( 'NONE', ( #5108, #8187, #13339, #31520, #3077 ) ) ;
#14679 = AXIS2_PLACEMENT_3D ( 'NONE', #22995, #11725, #2749 ) ;
#14680 = EDGE_CURVE ( 'NONE', #28024, #13152, #2976, .T. ) ;
#14681 = AXIS2_PLACEMENT_3D ( 'NONE', #30000, #10306, #1695 ) ;
#14682 = DIRECTION ( 'NONE',  ( 0.000000000000000000, 0.000000000000000000, -1.000000000000000000 ) ) ;
#14683 = ORIENTED_EDGE ( 'NONE', *, *, #21755, .T. ) ;
#14684 = CARTESIAN_POINT ( 'NONE',  ( -5.703708899247954101, -119.5207621440044790, 32.50000000000001421 ) ) ;
#14686 = EDGE_CURVE ( 'NONE', #10648, #25326, #10207, .T. ) ;
#14685 = EDGE_LOOP ( 'NONE', ( #31834, #3485, #9339, #15589 ) ) ;
#14687 = DIRECTION ( 'NONE',  ( -0.000000000000000000, -0.000000000000000000, 1.000000000000000000 ) ) ;
#14688 = AXIS2_PLACEMENT_3D ( 'NONE', #29522, #14930, #17541 ) ;
#14689 = VERTEX_POINT ( 'NONE', #19151 ) ;
#14690 = ADVANCED_FACE ( 'NONE', ( #13139 ), #2255, .F. ) ;
#14691 = CIRCLE ( 'NONE', #29049, 2.000000000000000000 ) ;
#14692 = ORIENTED_EDGE ( 'NONE', *, *, #36365, .F. ) ;
#14693 = VECTOR ( 'NONE', #17626, 1000.000000000000000 ) ;
#14694 =( NAMED_UNIT ( * ) PLANE_ANGLE_UNIT ( ) SI_UNIT ( $, .RADIAN. ) );
#14695 = CARTESIAN_POINT ( 'NONE',  ( 31.99999662536856704, 69.28203230275518365, 12.50000000000000000 ) ) ;
#14696 = CARTESIAN_POINT ( 'NONE',  ( 27.78182860042856461, 56.67878100130339902, 12.49999999999999822 ) ) ;
#14697 = VERTEX_POINT ( 'NONE', #22488 ) ;
#14698 = CARTESIAN_POINT ( 'NONE',  ( 34.00000000000000000, 103.4105893997321743, 32.50000000000000000 ) ) ;
#14699 = ADVANCED_FACE ( 'NONE', ( #13689 ), #33582, .F. ) ;
#14700 = CYLINDRICAL_SURFACE ( 'NONE', #11102, 3.500000000000003109 ) ;
#14701 = ADVANCED_FACE ( 'NONE', ( #4891 ), #24593, .F. ) ;
#14702 = CARTESIAN_POINT ( 'NONE',  ( -70.47608876694631874, -59.13646009116124702, -4.999999999999997335 ) ) ;
#14703 = EDGE_CURVE ( 'NONE', #23803, #953, #28156, .T. ) ;
#14704 = VECTOR ( 'NONE', #24041, 1000.000000000000000 ) ;
#14705 = ORIENTED_EDGE ( 'NONE', *, *, #15078, .T. ) ;
#14706 = DIRECTION ( 'NONE',  ( 1.000000000000000000, 0.000000000000000000, 0.000000000000000000 ) ) ;
#14707 = CARTESIAN_POINT ( 'NONE',  ( 61.99999662536843914, -34.64101615137759893, -9.999999999999998224 ) ) ;
#14708 = ADVANCED_FACE ( 'NONE', ( #11043 ), #7504, .F. ) ;
#14709 = ORIENTED_EDGE ( 'NONE', *, *, #2375, .F. ) ;
#14710 = DIRECTION ( 'NONE',  ( 1.000000000000000000, 0.000000000000000000, 0.000000000000000000 ) ) ;
#14711 = VECTOR ( 'NONE', #20304, 1000.000000000000000 ) ;
#14712 = LINE ( 'NONE', #1022, #14194 ) ;
#14713 = CARTESIAN_POINT ( 'NONE',  ( -2.000003374631289521, -69.28203230275519786, -9.999999999999998224 ) ) ;
#14714 = CIRCLE ( 'NONE', #6327, 2.000000000000001776 ) ;
#14715 = AXIS2_PLACEMENT_3D ( 'NONE', #11290, #6201, #5483 ) ;
#14716 = VECTOR ( 'NONE', #29916, 1000.000000000000000 ) ;
#14717 = DIRECTION ( 'NONE',  ( 0.000000000000000000, 0.000000000000000000, 1.000000000000000000 ) ) ;
#14718 = AXIS2_PLACEMENT_3D ( 'NONE', #28421, #2568, #36695 ) ;
#14719 = DIRECTION ( 'NONE',  ( 0.000000000000000000, 0.000000000000000000, -1.000000000000000000 ) ) ;
#14720 = VERTEX_POINT ( 'NONE', #2445 ) ;
#14721 = DIRECTION ( 'NONE',  ( 0.000000000000000000, 0.000000000000000000, 1.000000000000000000 ) ) ;
#14722 = CARTESIAN_POINT ( 'NONE',  ( 2.176667689905595005, 4.790324513057870881, -4.057749648769098272 ) ) ;
#14723 = CARTESIAN_POINT ( 'NONE',  ( 0.8179331680532997417, 5.301268757141563981, -5.826062401966623838 ) ) ;
#14724 = ORIENTED_EDGE ( 'NONE', *, *, #8819, .F. ) ;
#14725 = AXIS2_PLACEMENT_3D ( 'NONE', #35740, #1797, #4419 ) ;
#14726 = ORIENTED_EDGE ( 'NONE', *, *, #3219, .F. ) ;
#14727 = ORIENTED_EDGE ( 'NONE', *, *, #28455, .T. ) ;
#14728 = CARTESIAN_POINT ( 'NONE',  ( 4.468131147118817364E-15, -5.914770570062455768, -4.281776566113625115 ) ) ;
#14729 = DIRECTION ( 'NONE',  ( 1.000000000000000000, 0.000000000000000000, 0.000000000000000000 ) ) ;
#14730 = CARTESIAN_POINT ( 'NONE',  ( -40.00000337463113453, 69.28203230275516944, -9.999999999999998224 ) ) ;
#14731 = VECTOR ( 'NONE', #24823, 1000.000000000000000 ) ;
#14732 = VECTOR ( 'NONE', #24212, 1000.000000000000000 ) ;
#14733 = LINE ( 'NONE', #12084, #6896 ) ;
#14734 = ORIENTED_EDGE ( 'NONE', *, *, #10802, .T. ) ;
#14735 = CARTESIAN_POINT ( 'NONE',  ( -57.00000337463107059, 43.30127018922197379, 12.50000000000000000 ) ) ;
#14736 = EDGE_LOOP ( 'NONE', ( #25870, #24314 ) ) ;
#14737 = PRESENTATION_LAYER_ASSIGNMENT (  '', '', ( #27994 ) ) ;
#14738 = FACE_BOUND ( 'NONE', #29095, .T. ) ;
#14739 = VECTOR ( 'NONE', #12862, 1000.000000000000000 ) ;
#14740 = AXIS2_PLACEMENT_3D ( 'NONE', #1075, #699, #23405 ) ;
#14741 = CIRCLE ( 'NONE', #24334, 3.500000000000003109 ) ;
#14742 = VECTOR ( 'NONE', #11013, 1000.000000000000000 ) ;
#14743 = DIRECTION ( 'NONE',  ( 0.000000000000000000, 0.000000000000000000, 1.000000000000000000 ) ) ;
#14744 = DIRECTION ( 'NONE',  ( 0.000000000000000000, 0.000000000000000000, 1.000000000000000000 ) ) ;
#14745 = VERTEX_POINT ( 'NONE', #24952 ) ;
#14746 = CARTESIAN_POINT ( 'NONE',  ( 5.236872748402764621, 8.442024233997350580E-14, -4.057689166958447835 ) ) ;
#14747 =( NAMED_UNIT ( * ) SI_UNIT ( $, .STERADIAN. ) SOLID_ANGLE_UNIT ( ) );
#14748 = AXIS2_PLACEMENT_3D ( 'NONE', #21236, #24237, #16000 ) ;
#14749 = CARTESIAN_POINT ( 'NONE',  ( 58.48108235278871803, 36.97203788308964079, -4.999999999999997335 ) ) ;
#14750 = DIRECTION ( 'NONE',  ( 0.000000000000000000, 0.000000000000000000, 1.000000000000000000 ) ) ;
#14751 = DIRECTION ( 'NONE',  ( -1.000000000000000000, 0.000000000000000000, 0.000000000000000000 ) ) ;
#14752 = EDGE_CURVE ( 'NONE', #14801, #2589, #29947, .T. ) ;
#14753 = VERTEX_POINT ( 'NONE', #10871 ) ;
#14754 = DIRECTION ( 'NONE',  ( 1.000000000000000000, -9.251858538542971828E-16, 0.000000000000000000 ) ) ;
#14755 = CARTESIAN_POINT ( 'NONE',  ( -65.00000337463102085, 25.98076211353317433, 12.50000000000000000 ) ) ;
#14756 = DIRECTION ( 'NONE',  ( 0.000000000000000000, 0.000000000000000000, 1.000000000000000000 ) ) ;
#14757 = AXIS2_PLACEMENT_3D ( 'NONE', #13004, #24646, #7019 ) ;
#14758 = ORIENTED_EDGE ( 'NONE', *, *, #26266, .T. ) ;
#14759 = ORIENTED_EDGE ( 'NONE', *, *, #25869, .T. ) ;
#14760 = CIRCLE ( 'NONE', #24351, 33.00000000000001421 ) ;
#14761 = ORIENTED_EDGE ( 'NONE', *, *, #3837, .F. ) ;
#14762 = AXIS2_PLACEMENT_3D ( 'NONE', #25999, #31964, #34647 ) ;
#14763 = FACE_OUTER_BOUND ( 'NONE', #32453, .T. ) ;
#14764 = AXIS2_PLACEMENT_3D ( 'NONE', #15253, #18071, #29496 ) ;
#14765 = CIRCLE ( 'NONE', #11180, 27.00000000000001066 ) ;
#14766 = AXIS2_PLACEMENT_3D ( 'NONE', #22168, #10730, #25341 ) ;
#14767 = FACE_BOUND ( 'NONE', #18439, .T. ) ;
#14768 = VECTOR ( 'NONE', #9697, 1000.000000000000000 ) ;
#14769 = DIRECTION ( 'NONE',  ( 1.000000000000000000, 0.000000000000000000, 0.000000000000000000 ) ) ;
#14770 = DIRECTION ( 'NONE',  ( -0.000000000000000000, -0.000000000000000000, 1.000000000000000000 ) ) ;
#14771 = CYLINDRICAL_SURFACE ( 'NONE', #8252, 45.00000000000000711 ) ;
#14772 = ADVANCED_FACE ( 'NONE', ( #22310 ), #33751, .F. ) ;
#14773 = DIRECTION ( 'NONE',  ( -0.7650473262243665529, 0.6439740589782693148, 0.000000000000000000 ) ) ;
#14774 = EDGE_CURVE ( 'NONE', #26082, #2567, #611, .T. ) ;
#14775 = EDGE_LOOP ( 'NONE', ( #28623, #11778, #15447, #29956 ) ) ;
#14776 = CIRCLE ( 'NONE', #24372, 2.000000000000001776 ) ;
#14777 = ORIENTED_EDGE ( 'NONE', *, *, #13468, .T. ) ;
#14778 = CARTESIAN_POINT ( 'NONE',  ( 17.99999662536858125, 86.60254037844397601, -9.999999999999998224 ) ) ;
#14779 = CARTESIAN_POINT ( 'NONE',  ( -20.00000337463122690, 86.60254037844397601, -5.000000000000000000 ) ) ;
#14780 = CYLINDRICAL_SURFACE ( 'NONE', #27489, 2.000000000000001776 ) ;
#14781 = ORIENTED_EDGE ( 'NONE', *, *, #23863, .F. ) ;
#14782 = VECTOR ( 'NONE', #21404, 999.9999999999998863 ) ;
#14783 = EDGE_CURVE ( 'NONE', #30183, #4131, #20365, .T. ) ;
#14784 = AXIS2_PLACEMENT_3D ( 'NONE', #16853, #28273, #14016 ) ;
#14785 = FACE_BOUND ( 'NONE', #27085, .T. ) ;
#14786 = ORIENTED_EDGE ( 'NONE', *, *, #28820, .T. ) ;
#14787 = ORIENTED_EDGE ( 'NONE', *, *, #12252, .F. ) ;
#14788 = CIRCLE ( 'NONE', #33972, 2.000000000000001776 ) ;
#14789 = ORIENTED_EDGE ( 'NONE', *, *, #21711, .T. ) ;
#14790 = CARTESIAN_POINT ( 'NONE',  ( 1.443735181952766844, -4.939961795957303003, -5.918341802876224911 ) ) ;
#14791 = VERTEX_POINT ( 'NONE', #5806 ) ;
#14792 = AXIS2_PLACEMENT_3D ( 'NONE', #1485, #36182, #2432 ) ;
#14793 = PLANE ( 'NONE',  #33817 ) ;
#14794 = VECTOR ( 'NONE', #8260, 1000.000000000000000 ) ;
#14795 = CIRCLE ( 'NONE', #35188, 30.00000000000000000 ) ;
#14796 = CARTESIAN_POINT ( 'NONE',  ( -20.00000337463123756, -86.60254037844400443, 17.49999999999999645 ) ) ;
#14797 = ADVANCED_FACE ( 'NONE', ( #11965 ), #15385, .F. ) ;
#14798 = ORIENTED_EDGE ( 'NONE', *, *, #4870, .F. ) ;
#14799 = ORIENTED_EDGE ( 'NONE', *, *, #26117, .T. ) ;
#14800 = AXIS2_PLACEMENT_3D ( 'NONE', #27669, #1428, #24690 ) ;
#14801 = VERTEX_POINT ( 'NONE', #8983 ) ;
#14802 = VECTOR ( 'NONE', #8059, 1000.000000000000000 ) ;
#14803 = EDGE_LOOP ( 'NONE', ( #15727, #11431, #3873, #18274 ) ) ;
#14804 = EDGE_LOOP ( 'NONE', ( #13200, #4812 ) ) ;
#14805 = CARTESIAN_POINT ( 'NONE',  ( -52.39915983220772233, -35.19434990244957362, 12.49999999999999822 ) ) ;
#14806 = DIRECTION ( 'NONE',  ( 0.000000000000000000, 0.000000000000000000, 1.000000000000000000 ) ) ;
#14807 = ORIENTED_EDGE ( 'NONE', *, *, #7609, .T. ) ;
#14809 = CIRCLE ( 'NONE', #11795, 2.000000000000000000 ) ;
#14808 = DIRECTION ( 'NONE',  ( 0.000000000000000000, 0.000000000000000000, 1.000000000000000000 ) ) ;
#14810 = DIRECTION ( 'NONE',  ( -1.000000000000000000, 0.000000000000000000, 0.000000000000000000 ) ) ;
#14811 = DIRECTION ( 'NONE',  ( 0.000000000000000000, 0.000000000000000000, 1.000000000000000000 ) ) ;
#14812 = ORIENTED_EDGE ( 'NONE', *, *, #13082, .T. ) ;
#14813 = DIRECTION ( 'NONE',  ( 0.000000000000000000, 0.000000000000000000, 1.000000000000000000 ) ) ;
#14814 = VECTOR ( 'NONE', #13452, 1000.000000000000000 ) ;
#14815 = DIRECTION ( 'NONE',  ( 1.000000000000000000, 0.000000000000000000, 0.000000000000000000 ) ) ;
#14816 = AXIS2_PLACEMENT_3D ( 'NONE', #15221, #29853, #32088 ) ;
#14817 = EDGE_CURVE ( 'NONE', #20602, #8231, #2370, .T. ) ;
#14818 = CARTESIAN_POINT ( 'NONE',  ( 0.000000000000000000, 0.000000000000000000, 0.000000000000000000 ) ) ;
#14819 = ORIENTED_EDGE ( 'NONE', *, *, #19696, .F. ) ;
#14820 = FACE_OUTER_BOUND ( 'NONE', #20866, .T. ) ;
#14821 = CARTESIAN_POINT ( 'NONE',  ( -10.00000337463125000, -86.60254037844400443, -9.999999999999998224 ) ) ;
#14822 = ADVANCED_FACE ( 'NONE', ( #22865, #31824, #14241, #22686, #14591, #26032, #5996, #338, #17420, #5445, #2808, #26230, #6155, #23036, #25490, #17246, #17042, #3000, #11772, #28670, #25691, #25861, #31287, #33939, #34301, #17586, #5607, #28474, #11241, #8254, #8604, #20037, #31465, #16871, #151, #29014, #3347, #2612, #36931, #14785, #19688, #28836, #34135, #8436, #20236, #31659, #26584, #714, #20575, #29966, #12125, #7101, #21148, #3722, #20775, #4103, #32000, #32578, #18546, #27138, #4285, #17780, #9715, #32401, #29402, #15716, #1452, #9338, #15149, #9897, #24149, #9540, #6339, #9146, #898, #14982, #23419, #12698, #29217, #12318, #3547, #32212, #34853, #23791, #21336, #6543, #17977, #23590, #26411, #35242, #20973, #6716 ), #35033, .F. ) ;
#14823 = VERTEX_POINT ( 'NONE', #18147 ) ;
#14824 = CIRCLE ( 'NONE', #7045, 2.000000000000001776 ) ;
#14825 = ORIENTED_EDGE ( 'NONE', *, *, #30883, .T. ) ;
#14826 = LINE ( 'NONE', #20818, #3871 ) ;
#14827 = PRODUCT_DEFINITION ( 'UNKNOWN', '', #8193, #22309 ) ;
#14828 = CARTESIAN_POINT ( 'NONE',  ( -50.00000337463110611, -69.28203230275519786, -9.999999999999998224 ) ) ;
#14829 = FACE_OUTER_BOUND ( 'NONE', #15877, .T. ) ;
#14830 = CARTESIAN_POINT ( 'NONE',  ( -4.242640687119340726, -4.242640687119236809, 32.50000000000000000 ) ) ;
#14831 = EDGE_CURVE ( 'NONE', #30141, #10592, #29570, .T. ) ;
#14832 = VERTEX_POINT ( 'NONE', #15338 ) ;
#14833 = AXIS2_PLACEMENT_3D ( 'NONE', #30840, #13409, #31046 ) ;
#14834 = DIRECTION ( 'NONE',  ( 0.000000000000000000, 0.000000000000000000, 1.000000000000000000 ) ) ;
#14835 = PLANE ( 'NONE',  #9950 ) ;
#14836 = DIRECTION ( 'NONE',  ( 1.000000000000000000, 0.000000000000000000, 0.000000000000000000 ) ) ;
#14837 = EDGE_CURVE ( 'NONE', #6533, #7296, #32876, .T. ) ;
#14838 = CIRCLE ( 'NONE', #10056, 3.499999999999991562 ) ;
#14839 = ORIENTED_EDGE ( 'NONE', *, *, #11263, .F. ) ;
#14840 = AXIS2_PLACEMENT_3D ( 'NONE', #35185, #35385, #13028 ) ;
#14841 = AXIS2_PLACEMENT_3D ( 'NONE', #15603, #18779, #32850 ) ;
#14842 = DIRECTION ( 'NONE',  ( -1.000000000000000000, 0.000000000000000000, 0.000000000000000000 ) ) ;
#14843 = VERTEX_POINT ( 'NONE', #35427 ) ;
#14844 = CARTESIAN_POINT ( 'NONE',  ( -62.97617850287781494, -4.279621169095772615, -4.999999999999997335 ) ) ;
#14845 = DIRECTION ( 'NONE',  ( -0.000000000000000000, -0.000000000000000000, 1.000000000000000000 ) ) ;
#14846 = AXIS2_PLACEMENT_3D ( 'NONE', #31360, #3074, #5686 ) ;
#14847 = DIRECTION ( 'NONE',  ( 0.000000000000000000, 0.000000000000000000, -1.000000000000000000 ) ) ;
#14848 = ORIENTED_EDGE ( 'NONE', *, *, #15713, .T. ) ;
#14849 = ORIENTED_EDGE ( 'NONE', *, *, #5637, .F. ) ;
#14850 = CARTESIAN_POINT ( 'NONE',  ( 0.000000000000000000, 85.61789592134881843, -27.49999999999990408 ) ) ;
#14851 = DIRECTION ( 'NONE',  ( 0.000000000000000000, 0.000000000000000000, -1.000000000000000000 ) ) ;
#14852 = CARTESIAN_POINT ( 'NONE',  ( 84.99999662536831124, -25.98076211353319565, 17.49999999999999645 ) ) ;
#14853 = EDGE_CURVE ( 'NONE', #7448, #24238, #34699, .T. ) ;
#14854 = VERTEX_POINT ( 'NONE', #26967 ) ;
#14855 = CARTESIAN_POINT ( 'NONE',  ( -38.00000337463113453, 69.28203230275516944, -9.999999999999998224 ) ) ;
#14856 = FACE_BOUND ( 'NONE', #17088, .T. ) ;
#14857 = DIRECTION ( 'NONE',  ( 0.000000000000000000, 0.000000000000000000, 1.000000000000000000 ) ) ;
#14858 = CARTESIAN_POINT ( 'NONE',  ( 0.8333333333333268200, 5.292377467571581562, -3.818275046351166768 ) ) ;
#14859 = CIRCLE ( 'NONE', #3498, 33.00000000000001421 ) ;
#14860 = DIRECTION ( 'NONE',  ( 1.000000000000000000, 0.000000000000000000, 0.000000000000000000 ) ) ;
#14861 = CARTESIAN_POINT ( 'NONE',  ( -47.00000337463111322, 77.94228634059959404, 17.49999999999999645 ) ) ;
#14862 = EDGE_CURVE ( 'NONE', #26322, #31694, #20317, .T. ) ;
#14863 = CARTESIAN_POINT ( 'NONE',  ( -30.00000337463119848, -69.28203230275522628, 12.50000000000000000 ) ) ;
#14864 = AXIS2_PLACEMENT_3D ( 'NONE', #27056, #7203, #4377 ) ;
#14865 = EDGE_CURVE ( 'NONE', #2856, #10704, #16132, .T. ) ;
#14866 = DIRECTION ( 'NONE',  ( 0.000000000000000000, -0.4999999999999996114, 0.8660254037844388186 ) ) ;
#14867 = ORIENTED_EDGE ( 'NONE', *, *, #32370, .F. ) ;
#14868 = CARTESIAN_POINT ( 'NONE',  ( -12.00000337463127842, -69.28203230275519786, -5.000000000000000000 ) ) ;
#14869 = AXIS2_PLACEMENT_3D ( 'NONE', #21169, #6923, #3739 ) ;
#14870 = CARTESIAN_POINT ( 'NONE',  ( 84.99999662536831124, -8.660254037844397956, 17.49999999999999645 ) ) ;
#14871 = DIRECTION ( 'NONE',  ( 0.000000000000000000, 0.000000000000000000, 1.000000000000000000 ) ) ;
#14872 = AXIS2_PLACEMENT_3D ( 'NONE', #271, #23161, #34614 ) ;
#14873 = EDGE_LOOP ( 'NONE', ( #23555, #32106, #28690, #11243 ) ) ;
#14874 = ORIENTED_EDGE ( 'NONE', *, *, #32287, .F. ) ;
#14875 = VERTEX_POINT ( 'NONE', #30877 ) ;
#14876 = AXIS2_PLACEMENT_3D ( 'NONE', #1911, #35866, #10528 ) ;
#14877 = CARTESIAN_POINT ( 'NONE',  ( 3.567687560464448904, -3.713697318477654274, -0.1121614189353552921 ) ) ;
#14878 = CARTESIAN_POINT ( 'NONE',  ( -3.000000000000000000, 3.673940397442059868E-16, -25.03750572909317285 ) ) ;
#14879 = LINE ( 'NONE', #11672, #17228 ) ;
#14880 = ORIENTED_EDGE ( 'NONE', *, *, #5467, .T. ) ;
#14881 = ORIENTED_EDGE ( 'NONE', *, *, #8478, .T. ) ;
#14882 = AXIS2_PLACEMENT_3D ( 'NONE', #13686, #13482, #24945 ) ;
#14883 = CIRCLE ( 'NONE', #37058, 2.000000000000001776 ) ;
#14884 = DIRECTION ( 'NONE',  ( 1.000000000000000000, 0.000000000000000000, 0.000000000000000000 ) ) ;
#14885 = EDGE_CURVE ( 'NONE', #29836, #8231, #27529, .T. ) ;
#14886 = ORIENTED_EDGE ( 'NONE', *, *, #36392, .F. ) ;
#14887 = CARTESIAN_POINT ( 'NONE',  ( 84.99999662536832545, 25.98076211353319565, 12.50000000000000000 ) ) ;
#14888 = ORIENTED_EDGE ( 'NONE', *, *, #3019, .T. ) ;
#14889 = CYLINDRICAL_SURFACE ( 'NONE', #11166, 2.000000000000001776 ) ;
#14890 = ORIENTED_EDGE ( 'NONE', *, *, #14675, .F. ) ;
#14891 = EDGE_LOOP ( 'NONE', ( #31018, #35029 ) ) ;
#14892 = CYLINDRICAL_SURFACE ( 'NONE', #20208, 2.000000000000001776 ) ;
#14893 = CARTESIAN_POINT ( 'NONE',  ( -1.084202172485504434E-14, -5.773502691896260863, -2.080000000000000071 ) ) ;
#14894 = AXIS2_PLACEMENT_3D ( 'NONE', #5617, #13874, #5454 ) ;
#14895 = FACE_OUTER_BOUND ( 'NONE', #27478, .T. ) ;
#14896 = EDGE_LOOP ( 'NONE', ( #12710, #27184, #4828, #11750 ) ) ;
#14897 = LINE ( 'NONE', #6088, #23277 ) ;
#14898 = AXIS2_PLACEMENT_3D ( 'NONE', #12227, #6459, #34405 ) ;
#14899 = FACE_OUTER_BOUND ( 'NONE', #6277, .T. ) ;
#14900 = DIRECTION ( 'NONE',  ( 0.000000000000000000, 0.000000000000000000, 1.000000000000000000 ) ) ;
#14901 = EDGE_CURVE ( 'NONE', #19348, #22787, #36150, .T. ) ;
#14902 = EDGE_LOOP ( 'NONE', ( #22785, #22324, #19713, #16900 ) ) ;
#14903 = DIRECTION ( 'NONE',  ( 0.000000000000000000, 0.000000000000000000, 1.000000000000000000 ) ) ;
#14904 = DIRECTION ( 'NONE',  ( 1.000000000000000000, 0.000000000000000000, 0.000000000000000000 ) ) ;
#14905 = VECTOR ( 'NONE', #20323, 1000.000000000000000 ) ;
#14906 = ORIENTED_EDGE ( 'NONE', *, *, #28480, .F. ) ;
#14907 = EDGE_CURVE ( 'NONE', #10548, #27983, #23320, .T. ) ;
#14908 = CARTESIAN_POINT ( 'NONE',  ( -102.5304832720481869, 102.5304832720506596, 32.50000000000000000 ) ) ;
#14909 = DIRECTION ( 'NONE',  ( 0.000000000000000000, 0.000000000000000000, 1.000000000000000000 ) ) ;
#14910 = CARTESIAN_POINT ( 'NONE',  ( 34.99999662536853862, 77.94228634059959404, -5.000000000000000000 ) ) ;
#14911 = CIRCLE ( 'NONE', #1150, 2.000000000000001776 ) ;
#14912 = DIRECTION ( 'NONE',  ( 0.000000000000000000, 0.000000000000000000, -1.000000000000000000 ) ) ;
#14913 = EDGE_CURVE ( 'NONE', #9742, #32864, #5682, .T. ) ;
#14914 = VECTOR ( 'NONE', #8941, 1000.000000000000000 ) ;
#14915 = LINE ( 'NONE', #26351, #32273 ) ;
#14916 = CARTESIAN_POINT ( 'NONE',  ( 0.000000000000000000, 0.000000000000000000, -5.000000000000000000 ) ) ;
#14917 = EDGE_LOOP ( 'NONE', ( #13110, #10551, #29234, #10272 ) ) ;
#14918 = DIRECTION ( 'NONE',  ( 1.000000000000000000, 0.000000000000000000, 0.000000000000000000 ) ) ;
#14919 = EDGE_CURVE ( 'NONE', #23244, #33319, #27492, .T. ) ;
#14920 = CYLINDRICAL_SURFACE ( 'NONE', #26679, 2.000000000000001776 ) ;
#14921 = DIRECTION ( 'NONE',  ( 1.000000000000000000, 0.000000000000000000, 0.000000000000000000 ) ) ;
#14922 = ADVANCED_FACE ( 'NONE', ( #18717, #10656 ), #2013, .T. ) ;
#14923 = ORIENTED_EDGE ( 'NONE', *, *, #36839, .T. ) ;
#14924 = EDGE_LOOP ( 'NONE', ( #16642, #37034, #25494, #32474 ) ) ;
#14925 = ORIENTED_EDGE ( 'NONE', *, *, #3531, .T. ) ;
#14926 = AXIS2_PLACEMENT_3D ( 'NONE', #28438, #34455, #9303 ) ;
#14927 = CARTESIAN_POINT ( 'NONE',  ( 0.000000000000000000, 0.000000000000000000, 3.400000000000000355 ) ) ;
#14928 = CARTESIAN_POINT ( 'NONE',  ( -5.000000000000000000, 30.00000000000000355, 15.00000000000000000 ) ) ;
#14929 = AXIS2_PLACEMENT_3D ( 'NONE', #7663, #18909, #33550 ) ;
#14930 = DIRECTION ( 'NONE',  ( 0.000000000000000000, 0.000000000000000000, 1.000000000000000000 ) ) ;
#14931 = ADVANCED_FACE ( 'NONE', ( #4464 ), #15900, .F. ) ;
#14932 = EDGE_CURVE ( 'NONE', #15986, #22847, #24903, .T. ) ;
#14933 = EDGE_CURVE ( 'NONE', #37029, #25787, #29272, .T. ) ;
#14934 = LINE ( 'NONE', #23378, #301 ) ;
#14936 = EDGE_CURVE ( 'NONE', #23602, #9228, #28105, .T. ) ;
#14935 = ORIENTED_EDGE ( 'NONE', *, *, #3345, .F. ) ;
#14937 = CIRCLE ( 'NONE', #18527, 33.00000000000001421 ) ;
#14938 = EDGE_CURVE ( 'NONE', #7360, #32425, #19706, .T. ) ;
#14939 = DIRECTION ( 'NONE',  ( 0.000000000000000000, 0.000000000000000000, -1.000000000000000000 ) ) ;
#14940 = ORIENTED_EDGE ( 'NONE', *, *, #17840, .T. ) ;
#14941 = FACE_BOUND ( 'NONE', #26413, .T. ) ;
#14942 = AXIS2_PLACEMENT_3D ( 'NONE', #24713, #36532, #27134 ) ;
#14943 = AXIS2_PLACEMENT_3D ( 'NONE', #16411, #36110, #36295 ) ;
#14944 = PLANE ( 'NONE',  #27519 ) ;
#14945 = DIRECTION ( 'NONE',  ( 0.000000000000000000, 0.000000000000000000, 1.000000000000000000 ) ) ;
#14946 = CIRCLE ( 'NONE', #35914, 27.00000000000001066 ) ;
#14947 = VERTEX_POINT ( 'NONE', #13090 ) ;
#14948 = CARTESIAN_POINT ( 'NONE',  ( 5.999999999999998224, 0.000000000000000000, 0.000000000000000000 ) ) ;
#14949 = APPLICATION_PROTOCOL_DEFINITION ( 'draft international standard', 'automotive_design', 1998, #30999 ) ;
#14950 = CARTESIAN_POINT ( 'NONE',  ( -93.36492675454779544, -17.14523346298311779, 12.49999999999999822 ) ) ;
#14951 = CIRCLE ( 'NONE', #28114, 95.00000000000001421 ) ;
#14952 = DIRECTION ( 'NONE',  ( 0.000000000000000000, 0.000000000000000000, 1.000000000000000000 ) ) ;
#14953 = DIRECTION ( 'NONE',  ( 1.000000000000000000, 0.000000000000000000, 0.000000000000000000 ) ) ;
#14954 = ORIENTED_EDGE ( 'NONE', *, *, #3861, .F. ) ;
#14955 = CARTESIAN_POINT ( 'NONE',  ( 19.99999662536861678, -86.60254037844400443, 12.50000000000000000 ) ) ;
#14956 = AXIS2_PLACEMENT_3D ( 'NONE', #1062, #23756, #32545 ) ;
#14957 = CARTESIAN_POINT ( 'NONE',  ( 47.99999662536846756, 51.96152422706637708, 17.49999999999999645 ) ) ;
#14958 = CARTESIAN_POINT ( 'NONE',  ( -38.00000337463113453, 69.28203230275516944, -5.000000000000000000 ) ) ;
#14959 = ORIENTED_EDGE ( 'NONE', *, *, #3802, .F. ) ;
#14960 = VERTEX_POINT ( 'NONE', #7656 ) ;
#14961 = VERTEX_POINT ( 'NONE', #12887 ) ;
#14962 = DIRECTION ( 'NONE',  ( 1.000000000000000000, 0.000000000000000000, 0.000000000000000000 ) ) ;
#14963 = AXIS2_PLACEMENT_3D ( 'NONE', #14887, #17684, #28929 ) ;
#14964 = DIRECTION ( 'NONE',  ( 1.000000000000000000, 0.000000000000000000, 0.000000000000000000 ) ) ;
#14965 = AXIS2_PLACEMENT_3D ( 'NONE', #12166, #18016, #15756 ) ;
#14966 = DIRECTION ( 'NONE',  ( 0.000000000000000000, 0.000000000000000000, 1.000000000000000000 ) ) ;
#14967 = CYLINDRICAL_SURFACE ( 'NONE', #15923, 3.500000000000003109 ) ;
#14968 = CARTESIAN_POINT ( 'NONE',  ( -8.000003374631281972, 86.60254037844397601, 17.49999999999999645 ) ) ;
#14969 = AXIS2_PLACEMENT_3D ( 'NONE', #3774, #29638, #18778 ) ;
#14970 = DIRECTION ( 'NONE',  ( 0.000000000000000000, 0.000000000000000000, 1.000000000000000000 ) ) ;
#14971 = ORIENTED_EDGE ( 'NONE', *, *, #17630, .F. ) ;
#14973 = ORIENTED_EDGE ( 'NONE', *, *, #7147, .T. ) ;
#14972 = EDGE_CURVE ( 'NONE', #9610, #33654, #26285, .T. ) ;
#14974 = DIRECTION ( 'NONE',  ( 0.000000000000000000, 0.000000000000000000, 1.000000000000000000 ) ) ;
#14975 = ADVANCED_FACE ( 'NONE', ( #22270 ), #33708, .F. ) ;
#14976 = CIRCLE ( 'NONE', #11961, 3.500000000000000888 ) ;
#14977 = CARTESIAN_POINT ( 'NONE',  ( 59.99999662536843914, -34.64101615137759893, 17.49999999999999645 ) ) ;
#14978 = EDGE_CURVE ( 'NONE', #21597, #17068, #6535, .T. ) ;
#14979 = DIRECTION ( 'NONE',  ( 0.000000000000000000, 0.000000000000000000, 1.000000000000000000 ) ) ;
#14980 = ORIENTED_EDGE ( 'NONE', *, *, #29456, .T. ) ;
#14981 = AXIS2_PLACEMENT_3D ( 'NONE', #13406, #36307, #4434 ) ;
#14982 = FACE_BOUND ( 'NONE', #29652, .T. ) ;
#14983 = ORIENTED_EDGE ( 'NONE', *, *, #24, .T. ) ;
#14984 = ORIENTED_EDGE ( 'NONE', *, *, #5939, .T. ) ;
#14985 = FACE_OUTER_BOUND ( 'NONE', #14775, .T. ) ;
#14986 = VERTEX_POINT ( 'NONE', #18902 ) ;
#14987 = AXIS2_PLACEMENT_3D ( 'NONE', #539, #8792, #34685 ) ;
#14988 = SHAPE_REPRESENTATION_RELATIONSHIP ( 'NONE' , 'NONE' ,  #33015, #17512 ) ;
#14989 = CARTESIAN_POINT ( 'NONE',  ( -60.00000337463104216, 51.96152422706639129, -5.000000000000000000 ) ) ;
#14990 = CARTESIAN_POINT ( 'NONE',  ( -83.00000337463092137, 25.98076211353317433, -9.999999999999998224 ) ) ;
#14991 = DIRECTION ( 'NONE',  ( 0.000000000000000000, 0.000000000000000000, 1.000000000000000000 ) ) ;
#14992 = CIRCLE ( 'NONE', #25185, 2.000000000000001776 ) ;
#14993 = ORIENTED_EDGE ( 'NONE', *, *, #27050, .T. ) ;
#14994 = ORIENTED_EDGE ( 'NONE', *, *, #30271, .T. ) ;
#14995 = AXIS2_PLACEMENT_3D ( 'NONE', #11793, #28496, #2830 ) ;
#14996 = ORIENTED_EDGE ( 'NONE', *, *, #5384, .F. ) ;
#14997 = EDGE_CURVE ( 'NONE', #18549, #5127, #11327, .T. ) ;
#14998 = VERTEX_POINT ( 'NONE', #13269 ) ;
#14999 = ORIENTED_EDGE ( 'NONE', *, *, #26266, .F. ) ;
#15000 = DIRECTION ( 'NONE',  ( -0.000000000000000000, -0.000000000000000000, 1.000000000000000000 ) ) ;
#15001 = CARTESIAN_POINT ( 'NONE',  ( -3.374631334790434423E-06, 69.28203230275516944, 12.50000000000000000 ) ) ;
#15002 = EDGE_LOOP ( 'NONE', ( #29274, #10779, #6712, #13247 ) ) ;
#15003 = CARTESIAN_POINT ( 'NONE',  ( -38.00000337463113453, -69.28203230275519786, 12.50000000000000000 ) ) ;
#15004 = DIRECTION ( 'NONE',  ( 0.000000000000000000, 0.000000000000000000, -1.000000000000000000 ) ) ;
#15005 = CARTESIAN_POINT ( 'NONE',  ( -145.0000000000000000, 6.000000000001517009, 32.55002500000000509 ) ) ;
#15006 = ORIENTED_EDGE ( 'NONE', *, *, #3108, .F. ) ;
#15007 = LINE ( 'NONE', #741, #29007 ) ;
#15008 = LINE ( 'NONE', #6371, #13201 ) ;
#15009 = CARTESIAN_POINT ( 'NONE',  ( 82.27241335952179213, 47.49999999999982236, 27.50000000000000000 ) ) ;
#15010 = VERTEX_POINT ( 'NONE', #16837 ) ;
#15011 = DIRECTION ( 'NONE',  ( 1.000000000000000000, 0.000000000000000000, 0.000000000000000000 ) ) ;
#15012 = DIRECTION ( 'NONE',  ( 0.000000000000000000, 0.000000000000000000, 1.000000000000000000 ) ) ;
#15013 = ORIENTED_EDGE ( 'NONE', *, *, #16130, .T. ) ;
#15014 = EDGE_LOOP ( 'NONE', ( #37023, #26033, #30863, #1309, #22704 ) ) ;
#15015 = CARTESIAN_POINT ( 'NONE',  ( -20.00000337463123756, -69.28203230275522628, 12.50000000000000000 ) ) ;
#15016 = DIRECTION ( 'NONE',  ( -0.000000000000000000, 0.000000000000000000, -1.000000000000000000 ) ) ;
#15017 = AXIS2_PLACEMENT_3D ( 'NONE', #33164, #4693, #5038 ) ;
#15018 = ADVANCED_FACE ( 'NONE', ( #25995 ), #34643, .F. ) ;
#15019 = DIRECTION ( 'NONE',  ( 0.000000000000000000, 0.000000000000000000, 1.000000000000000000 ) ) ;
#15020 = CARTESIAN_POINT ( 'NONE',  ( -5.000000000000000000, 2.886751345948126879, -2.079999999999992077 ) ) ;
#15021 = ORIENTED_EDGE ( 'NONE', *, *, #27063, .F. ) ;
#15022 = CARTESIAN_POINT ( 'NONE',  ( -5.000000000000000888, 1.231908430319606618, -0.1119772403577100062 ) ) ;
#15023 = DIRECTION ( 'NONE',  ( 0.000000000000000000, 0.000000000000000000, 1.000000000000000000 ) ) ;
#15024 = ORIENTED_EDGE ( 'NONE', *, *, #16057, .T. ) ;
#15025 = CARTESIAN_POINT ( 'NONE',  ( 1.999996625368665182, 69.28203230275516944, -9.999999999999998224 ) ) ;
#15026 = ORIENTED_EDGE ( 'NONE', *, *, #1173, .F. ) ;
#15027 = DIRECTION ( 'NONE',  ( 1.000000000000000000, 0.000000000000000000, 0.000000000000000000 ) ) ;
#15028 = CARTESIAN_POINT ( 'NONE',  ( -3.374631289687624047E-06, -69.28203230275519786, 17.49999999999999645 ) ) ;
#15029 = EDGE_CURVE ( 'NONE', #5584, #2344, #2959, .T. ) ;
#15030 = DIRECTION ( 'NONE',  ( 0.000000000000000000, 0.000000000000000000, 1.000000000000000000 ) ) ;
#15031 = ORIENTED_EDGE ( 'NONE', *, *, #24319, .F. ) ;
#15032 = EDGE_LOOP ( 'NONE', ( #20975, #36001, #12621, #11335, #21480, #21624 ) ) ;
#15033 = CARTESIAN_POINT ( 'NONE',  ( 71.99999662536839651, -3.469446951953614189E-15, 17.49999999999999645 ) ) ;
#15034 = ADVANCED_FACE ( 'NONE', ( #20375 ), #6120, .F. ) ;
#15035 = CARTESIAN_POINT ( 'NONE',  ( -105.2709382882094218, 37.58034962363107923, 32.50000000000000711 ) ) ;
#15036 = DIRECTION ( 'NONE',  ( 0.000000000000000000, 0.000000000000000000, -1.000000000000000000 ) ) ;
#15037 = ORIENTED_EDGE ( 'NONE', *, *, #16072, .T. ) ;
#15038 = CARTESIAN_POINT ( 'NONE',  ( 45.00000000000000000, 5.510910596163089556E-15, 15.00000000000000000 ) ) ;
#15039 = FACE_BOUND ( 'NONE', #4486, .T. ) ;
#15040 = EDGE_CURVE ( 'NONE', #36323, #31133, #13998, .T. ) ;
#15041 = LINE ( 'NONE', #34919, #29203 ) ;
#15042 = CYLINDRICAL_SURFACE ( 'NONE', #12682, 2.000000000000001776 ) ;
#15043 = CARTESIAN_POINT ( 'NONE',  ( 31.83425564451589196, 89.42901512340320380, 12.49999999999999822 ) ) ;
#15044 = ORIENTED_EDGE ( 'NONE', *, *, #21655, .T. ) ;
#15045 = DIRECTION ( 'NONE',  ( 1.000000000000000000, 0.000000000000000000, 0.000000000000000000 ) ) ;
#15046 = FACE_OUTER_BOUND ( 'NONE', #15806, .T. ) ;
#15047 = EDGE_CURVE ( 'NONE', #21277, #5475, #11901, .T. ) ;
#15048 = ORIENTED_EDGE ( 'NONE', *, *, #28585, .T. ) ;
#15049 = DIRECTION ( 'NONE',  ( 0.000000000000000000, -1.034244904716769672E-15, -1.000000000000000000 ) ) ;
#15050 = FACE_BOUND ( 'NONE', #14013, .T. ) ;
#15051 = FACE_OUTER_BOUND ( 'NONE', #2704, .T. ) ;
#15052 = ORIENTED_EDGE ( 'NONE', *, *, #23717, .F. ) ;
#15053 = ORIENTED_EDGE ( 'NONE', *, *, #10157, .F. ) ;
#15054 = ORIENTED_EDGE ( 'NONE', *, *, #20614, .T. ) ;
#15055 = DIRECTION ( 'NONE',  ( 1.000000000000000000, 0.000000000000000000, 0.000000000000000000 ) ) ;
#15056 = EDGE_CURVE ( 'NONE', #8634, #33684, #37083, .T. ) ;
#15057 = CARTESIAN_POINT ( 'NONE',  ( 54.99999662536844625, 60.62177826491077326, -9.999999999999998224 ) ) ;
#15058 = CARTESIAN_POINT ( 'NONE',  ( 9.999996625368625658, 86.60254037844397601, 17.49999999999999645 ) ) ;
#15059 = ORIENTED_EDGE ( 'NONE', *, *, #17714, .F. ) ;
#15060 = CIRCLE ( 'NONE', #24035, 2.000000000000001776 ) ;
#15061 = VERTEX_POINT ( 'NONE', #14192 ) ;
#15062 = EDGE_LOOP ( 'NONE', ( #32817, #31288 ) ) ;
#15063 = CARTESIAN_POINT ( 'NONE',  ( 102.5304832720496080, 102.5304832720492527, 32.55002500000000509 ) ) ;
#15064 = ORIENTED_EDGE ( 'NONE', *, *, #18233, .T. ) ;
#15065 = CARTESIAN_POINT ( 'NONE',  ( -14.38831834687553446, -115.5694366505189237, 32.50000000000000000 ) ) ;
#15066 = ORIENTED_EDGE ( 'NONE', *, *, #9426, .T. ) ;
#15067 = DIRECTION ( 'NONE',  ( 0.000000000000000000, 0.000000000000000000, 1.000000000000000000 ) ) ;
#15068 = ORIENTED_EDGE ( 'NONE', *, *, #26296, .T. ) ;
#15069 = ORIENTED_EDGE ( 'NONE', *, *, #34579, .F. ) ;
#15070 = ADVANCED_FACE ( 'NONE', ( #11735 ), #19648, .F. ) ;
#15071 = CARTESIAN_POINT ( 'NONE',  ( 69.99999662536838230, -51.96152422706639840, 17.49999999999999645 ) ) ;
#15072 = CARTESIAN_POINT ( 'NONE',  ( 4.088737910769899564, -3.412868758467433317, -1.160540885688329249 ) ) ;
#15073 = ADVANCED_FACE ( 'NONE', ( #17200 ), #28256, .F. ) ;
#15074 = CARTESIAN_POINT ( 'NONE',  ( 20.00000000000001066, 89.94802294027088863, -19.99999999999999645 ) ) ;
#15075 = ORIENTED_EDGE ( 'NONE', *, *, #28204, .F. ) ;
#15076 = ORIENTED_EDGE ( 'NONE', *, *, #9265, .T. ) ;
#15077 = CARTESIAN_POINT ( 'NONE',  ( 67.30619744049005249, 84.18124734178236679, 27.50000000000000000 ) ) ;
#15078 = EDGE_CURVE ( 'NONE', #31695, #25696, #20912, .T. ) ;
#15079 = PLANE ( 'NONE',  #6314 ) ;
#15080 = DIRECTION ( 'NONE',  ( 0.000000000000000000, 0.000000000000000000, -1.000000000000000000 ) ) ;
#15081 = EDGE_LOOP ( 'NONE', ( #25415, #30657, #15085, #9189 ) ) ;
#15082 = CARTESIAN_POINT ( 'NONE',  ( -4.279621169095561228, 62.97617850287782915, 12.49999999999999822 ) ) ;
#15083 = LINE ( 'NONE', #9650, #21565 ) ;
#15084 = AXIS2_PLACEMENT_3D ( 'NONE', #9254, #20691, #4215 ) ;
#15085 = ORIENTED_EDGE ( 'NONE', *, *, #32287, .T. ) ;
#15086 = DIRECTION ( 'NONE',  ( -1.000000000000000000, 0.000000000000000000, 0.000000000000000000 ) ) ;
#15087 = EDGE_CURVE ( 'NONE', #35287, #14947, #25706, .T. ) ;
#15088 = DIRECTION ( 'NONE',  ( 0.000000000000000000, 0.000000000000000000, 1.000000000000000000 ) ) ;
#15089 = DIRECTION ( 'NONE',  ( 0.000000000000000000, 0.000000000000000000, 1.000000000000000000 ) ) ;
#15090 = CARTESIAN_POINT ( 'NONE',  ( -20.00000337463124112, 69.28203230275516944, -5.000000000000000000 ) ) ;
#15091 = FACE_OUTER_BOUND ( 'NONE', #33906, .T. ) ;
#15092 = EDGE_CURVE ( 'NONE', #32017, #598, #30493, .T. ) ;
#15093 = DIRECTION ( 'NONE',  ( 1.000000000000000000, 0.000000000000000000, 0.000000000000000000 ) ) ;
#15094 = ORIENTED_EDGE ( 'NONE', *, *, #9161, .T. ) ;
#15095 = DIRECTION ( 'NONE',  ( 0.000000000000000000, 0.000000000000000000, 1.000000000000000000 ) ) ;
#15096 = CARTESIAN_POINT ( 'NONE',  ( 0.8665032349992052296, 5.555903485205155867, -4.190643565754943900 ) ) ;
#15097 = DIRECTION ( 'NONE',  ( 0.000000000000000000, 0.000000000000000000, 1.000000000000000000 ) ) ;
#15098 = ORIENTED_EDGE ( 'NONE', *, *, #28842, .T. ) ;
#15099 = EDGE_LOOP ( 'NONE', ( #20794, #18093 ) ) ;
#15100 = ORIENTED_EDGE ( 'NONE', *, *, #32489, .F. ) ;
#15101 = CARTESIAN_POINT ( 'NONE',  ( 0.000000000000000000, 0.000000000000000000, -6.000000000000000000 ) ) ;
#15102 = DIRECTION ( 'NONE',  ( 0.000000000000000000, 0.000000000000000000, -1.000000000000000000 ) ) ;
#15103 = CARTESIAN_POINT ( 'NONE',  ( -73.00000337463097821, 25.98076211353318854, 12.50000000000000000 ) ) ;
#15104 = EDGE_CURVE ( 'NONE', #7234, #11585, #33895, .T. ) ;
#15105 = CIRCLE ( 'NONE', #15700, 2.000000000000000000 ) ;
#15106 = DIRECTION ( 'NONE',  ( 1.000000000000000000, 0.000000000000000000, 0.000000000000000000 ) ) ;
#15107 = ORIENTED_EDGE ( 'NONE', *, *, #15567, .T. ) ;
#15108 = CYLINDRICAL_SURFACE ( 'NONE', #27544, 2.000000000000001776 ) ;
#15109 = VERTEX_POINT ( 'NONE', #2577 ) ;
#15110 = FACE_BOUND ( 'NONE', #1608, .T. ) ;
#15111 = EDGE_CURVE ( 'NONE', #18148, #24065, #28628, .T. ) ;
#15112 = DIRECTION ( 'NONE',  ( 0.000000000000000000, 0.000000000000000000, 1.000000000000000000 ) ) ;
#15113 = EDGE_CURVE ( 'NONE', #33091, #5840, #23919, .T. ) ;
#15114 = DIRECTION ( 'NONE',  ( 0.000000000000000000, 0.000000000000000000, 1.000000000000000000 ) ) ;
#15115 = ADVANCED_FACE ( 'NONE', ( #8568 ), #20002, .F. ) ;
#15116 = EDGE_LOOP ( 'NONE', ( #29943, #3910, #36281, #31832, #16982 ) ) ;
#15117 = DIRECTION ( 'NONE',  ( 0.000000000000000000, 0.000000000000000000, 1.000000000000000000 ) ) ;
#15118 = DIRECTION ( 'NONE',  ( 0.000000000000000000, 0.000000000000000000, -1.000000000000000000 ) ) ;
#15119 = AXIS2_PLACEMENT_3D ( 'NONE', #24625, #21782, #27419 ) ;
#15120 = CARTESIAN_POINT ( 'NONE',  ( -68.00000337463102085, -51.96152422706641971, 17.49999999999999645 ) ) ;
#15121 = CARTESIAN_POINT ( 'NONE',  ( -31.00000000000027356, -58.88972745734168512, 12.49999999999999822 ) ) ;
#15122 = EDGE_LOOP ( 'NONE', ( #10259, #23034, #2929, #12161 ) ) ;
#15123 = CYLINDRICAL_SURFACE ( 'NONE', #10640, 2.000000000000001776 ) ;
#15124 = CARTESIAN_POINT ( 'NONE',  ( -37.00000337463116296, 77.94228634059957983, 12.50000000000000000 ) ) ;
#15125 = CARTESIAN_POINT ( 'NONE',  ( 7.999996625368656744, -86.60254037844400443, -9.999999999999998224 ) ) ;
#15126 = VERTEX_POINT ( 'NONE', #23001 ) ;
#15127 = VERTEX_POINT ( 'NONE', #34445 ) ;
#15128 = EDGE_CURVE ( 'NONE', #36148, #4050, #19734, .T. ) ;
#15129 = CIRCLE ( 'NONE', #22899, 2.000000000000001776 ) ;
#15130 = ORIENTED_EDGE ( 'NONE', *, *, #11736, .F. ) ;
#15131 = CIRCLE ( 'NONE', #6752, 95.00000000000001421 ) ;
#15132 = DIRECTION ( 'NONE',  ( 0.000000000000000000, 0.000000000000000000, 1.000000000000000000 ) ) ;
#15133 = DIRECTION ( 'NONE',  ( 0.000000000000000000, 0.000000000000000000, 1.000000000000000000 ) ) ;
#15134 = DIRECTION ( 'NONE',  ( -1.000000000000000000, 0.000000000000000000, 0.000000000000000000 ) ) ;
#15135 = DIRECTION ( 'NONE',  ( 0.000000000000000000, 0.000000000000000000, -1.000000000000000000 ) ) ;
#15136 = CARTESIAN_POINT ( 'NONE',  ( 91.99999662536828282, 0.000000000000000000, -9.999999999999998224 ) ) ;
#15137 = FACE_OUTER_BOUND ( 'NONE', #20577, .T. ) ;
#15138 = EDGE_LOOP ( 'NONE', ( #6024, #14433, #20591, #29805 ) ) ;
#15139 = ORIENTED_EDGE ( 'NONE', *, *, #31979, .F. ) ;
#15140 = AXIS2_PLACEMENT_3D ( 'NONE', #27002, #6749, #24585 ) ;
#15141 = DIRECTION ( 'NONE',  ( 1.000000000000000000, 0.000000000000000000, 0.000000000000000000 ) ) ;
#15142 = EDGE_CURVE ( 'NONE', #20452, #27221, #16771, .T. ) ;
#15143 = DIRECTION ( 'NONE',  ( -0.000000000000000000, -0.000000000000000000, 1.000000000000000000 ) ) ;
#15144 = ORIENTED_EDGE ( 'NONE', *, *, #21138, .T. ) ;
#15145 = EDGE_CURVE ( 'NONE', #5554, #4400, #26314, .T. ) ;
#15146 = FACE_OUTER_BOUND ( 'NONE', #36664, .T. ) ;
#15147 = EDGE_LOOP ( 'NONE', ( #14709, #23, #28139, #6489 ) ) ;
#15148 = EDGE_CURVE ( 'NONE', #37066, #31753, #29533, .T. ) ;
#15149 = FACE_BOUND ( 'NONE', #26947, .T. ) ;
#15150 = ORIENTED_EDGE ( 'NONE', *, *, #14222, .T. ) ;
#15151 = AXIS2_PLACEMENT_3D ( 'NONE', #19472, #33913, #9270 ) ;
#15152 = ORIENTED_EDGE ( 'NONE', *, *, #22780, .T. ) ;
#15153 = EDGE_CURVE ( 'NONE', #8725, #25751, #29923, .T. ) ;
#15154 = CARTESIAN_POINT ( 'NONE',  ( -65.63757354697304436, -58.72612421542294925, 12.50000000000000000 ) ) ;
#15155 = VERTEX_POINT ( 'NONE', #21289 ) ;
#15156 = EDGE_CURVE ( 'NONE', #18023, #30464, #7183, .T. ) ;
#15157 = CARTESIAN_POINT ( 'NONE',  ( -53.72397537678465085, -62.16182779291699489, -5.000000000000000000 ) ) ;
#15158 = DIRECTION ( 'NONE',  ( 1.000000000000000000, 0.000000000000000000, 0.000000000000000000 ) ) ;
#15159 = CARTESIAN_POINT ( 'NONE',  ( -5.000000000000000888, -2.886751345948162406, -3.984345921091775100 ) ) ;
#15160 = ORIENTED_EDGE ( 'NONE', *, *, #1840, .F. ) ;
#15161 = ORIENTED_EDGE ( 'NONE', *, *, #31933, .F. ) ;
#15162 = CIRCLE ( 'NONE', #787, 2.000000000000001776 ) ;
#15163 = EDGE_CURVE ( 'NONE', #1946, #29329, #32732, .T. ) ;
#15164 = EDGE_LOOP ( 'NONE', ( #16873, #21633, #19541, #36821 ) ) ;
#15165 = EDGE_CURVE ( 'NONE', #8516, #8626, #9683, .T. ) ;
#15166 = ORIENTED_EDGE ( 'NONE', *, *, #27848, .F. ) ;
#15167 = CIRCLE ( 'NONE', #28917, 2.000000000000001776 ) ;
#15168 = VERTEX_POINT ( 'NONE', #32368 ) ;
#15169 = ADVANCED_FACE ( 'NONE', ( #15498 ), #9292, .F. ) ;
#15170 = DIRECTION ( 'NONE',  ( 1.000000000000000000, 0.000000000000000000, 0.000000000000000000 ) ) ;
#15171 = EDGE_CURVE ( 'NONE', #20878, #9729, #32166, .T. ) ;
#15172 = DIRECTION ( 'NONE',  ( 0.000000000000000000, 0.000000000000000000, 1.000000000000000000 ) ) ;
#15173 = ORIENTED_EDGE ( 'NONE', *, *, #16134, .F. ) ;
#15174 = DIRECTION ( 'NONE',  ( 0.000000000000000000, -0.5000000000000013323, -0.8660254037844379305 ) ) ;
#15175 = CARTESIAN_POINT ( 'NONE',  ( 102.6344459086133298, 62.23183214669949592, 32.50000000000000711 ) ) ;
#15176 = DIRECTION ( 'NONE',  ( 1.000000000000000000, 0.000000000000000000, 0.000000000000000000 ) ) ;
#15177 = ORIENTED_EDGE ( 'NONE', *, *, #28307, .F. ) ;
#15178 = DIRECTION ( 'NONE',  ( 0.000000000000000000, 0.000000000000000000, 1.000000000000000000 ) ) ;
#15179 = VECTOR ( 'NONE', #11347, 1000.000000000000000 ) ;
#15180 = CARTESIAN_POINT ( 'NONE',  ( -56.67878100130369035, 27.78182860042797131, -4.999999999999997335 ) ) ;
#15181 = VECTOR ( 'NONE', #35668, 1000.000000000000000 ) ;
#15182 = CYLINDRICAL_SURFACE ( 'NONE', #18837, 2.000000000000001776 ) ;
#15183 = ORIENTED_EDGE ( 'NONE', *, *, #20159, .T. ) ;
#15184 = DIRECTION ( 'NONE',  ( 0.000000000000000000, 0.000000000000000000, 1.000000000000000000 ) ) ;
#15185 = DIRECTION ( 'NONE',  ( -1.000000000000000000, 0.000000000000000000, 0.000000000000000000 ) ) ;
#15186 = AXIS2_PLACEMENT_3D ( 'NONE', #18479, #7033, #15476 ) ;
#15187 = EDGE_LOOP ( 'NONE', ( #4956, #7090, #32577, #8043 ) ) ;
#15188 = ORIENTED_EDGE ( 'NONE', *, *, #16743, .F. ) ;
#15189 = CARTESIAN_POINT ( 'NONE',  ( -20.00000337463123756, -86.60254037844400443, -9.999999999999998224 ) ) ;
#15190 = CARTESIAN_POINT ( 'NONE',  ( -83.49774789488644444, 24.66044833507834610, 12.50000000000000000 ) ) ;
#15191 = DIRECTION ( 'NONE',  ( -0.000000000000000000, -0.000000000000000000, 1.000000000000000000 ) ) ;
#15192 = CARTESIAN_POINT ( 'NONE',  ( -5.000000000000000000, 1.352381405509855972, -0.8629530094790016648 ) ) ;
#15193 = EDGE_LOOP ( 'NONE', ( #19118, #13814, #24917, #1029, #3091 ) ) ;
#15194 = ADVANCED_FACE ( 'NONE', ( #32536 ), #6852, .F. ) ;
#15195 = CARTESIAN_POINT ( 'NONE',  ( 32.99999662536855283, 60.62177826491078747, 12.50000000000000000 ) ) ;
#15196 = LINE ( 'NONE', #4151, #3362 ) ;
#15197 = VECTOR ( 'NONE', #13423, 1000.000000000000000 ) ;
#15198 = ORIENTED_EDGE ( 'NONE', *, *, #19956, .T. ) ;
#15199 = DIRECTION ( 'NONE',  ( 1.000000000000000000, 0.000000000000000000, 0.000000000000000000 ) ) ;
#15200 = EDGE_LOOP ( 'NONE', ( #21294, #37002, #10197, #13934 ) ) ;
#15201 = CARTESIAN_POINT ( 'NONE',  ( -12.00000337463128197, 86.60254037844397601, 17.49999999999999645 ) ) ;
#15202 = CIRCLE ( 'NONE', #32570, 2.000000000000001776 ) ;
#15203 = CARTESIAN_POINT ( 'NONE',  ( -47.63139720814438505, -27.49999999999955591, -5.000000000000000000 ) ) ;
#15204 = AXIS2_PLACEMENT_3D ( 'NONE', #33034, #19177, #22335 ) ;
#15205 = CYLINDRICAL_SURFACE ( 'NONE', #32830, 2.000000000000001776 ) ;
#15206 = EDGE_LOOP ( 'NONE', ( #1073, #2821, #1749, #23792, #4455, #8206 ) ) ;
#15207 = EDGE_LOOP ( 'NONE', ( #25661, #34379 ) ) ;
#15208 = DIRECTION ( 'NONE',  ( 0.000000000000000000, 0.000000000000000000, 1.000000000000000000 ) ) ;
#15209 = VERTEX_POINT ( 'NONE', #23386 ) ;
#15210 = CARTESIAN_POINT ( 'NONE',  ( 0.000000000000000000, 0.000000000000000000, 12.49999999999999822 ) ) ;
#15211 = EDGE_CURVE ( 'NONE', #18995, #14204, #33534, .T. ) ;
#15212 = CARTESIAN_POINT ( 'NONE',  ( 102.5304832720488832, -102.5304832720499633, 32.50000000000000000 ) ) ;
#15213 = CYLINDRICAL_SURFACE ( 'NONE', #4689, 2.000000000000001776 ) ;
#15214 = FACE_OUTER_BOUND ( 'NONE', #32479, .T. ) ;
#15215 = DIRECTION ( 'NONE',  ( 0.000000000000000000, -0.8660254037844418162, 0.4999999999999945044 ) ) ;
#15216 = ORIENTED_EDGE ( 'NONE', *, *, #12974, .F. ) ;
#15217 = LINE ( 'NONE', #17483, #12909 ) ;
#15218 = AXIS2_PLACEMENT_3D ( 'NONE', #27088, #13525, #30087 ) ;
#15219 = CARTESIAN_POINT ( 'NONE',  ( 35.44550000000001688, 3.673940397442061840E-16, -3.000000000000001776 ) ) ;
#15220 = ORIENTED_EDGE ( 'NONE', *, *, #26211, .T. ) ;
#15221 = CARTESIAN_POINT ( 'NONE',  ( 70.47608876694671665, 59.13646009116074964, -4.999999999999997335 ) ) ;
#15222 = CARTESIAN_POINT ( 'NONE',  ( -72.77422209630324801, -61.06482292022084124, 12.49999999999999822 ) ) ;
#15223 = LINE ( 'NONE', #23490, #31152 ) ;
#15224 = CIRCLE ( 'NONE', #6233, 2.000000000000001776 ) ;
#15225 = ORIENTED_EDGE ( 'NONE', *, *, #2827, .F. ) ;
#15226 = ORIENTED_EDGE ( 'NONE', *, *, #6750, .F. ) ;
#15227 = CIRCLE ( 'NONE', #21198, 27.00000000000001066 ) ;
#15228 = DIRECTION ( 'NONE',  ( 1.000000000000000000, 0.000000000000000000, 0.000000000000000000 ) ) ;
#15229 = CARTESIAN_POINT ( 'NONE',  ( -57.00000337463109901, -60.62177826491083010, -5.000000000000000000 ) ) ;
#15230 = CARTESIAN_POINT ( 'NONE',  ( -2.008727693139930270, -4.613763217533273675, -0.5592653008974395323 ) ) ;
#15231 = ORIENTED_EDGE ( 'NONE', *, *, #12405, .T. ) ;
#15232 = ORIENTED_EDGE ( 'NONE', *, *, #33991, .T. ) ;
#15233 = ORIENTED_EDGE ( 'NONE', *, *, #35132, .T. ) ;
#15234 = EDGE_CURVE ( 'NONE', #10851, #36497, #31102, .T. ) ;
#15235 = ADVANCED_FACE ( 'NONE', ( #18106 ), #34818, .F. ) ;
#15236 = DIRECTION ( 'NONE',  ( 0.000000000000000000, 0.000000000000000000, 1.000000000000000000 ) ) ;
#15237 = CIRCLE ( 'NONE', #11119, 2.000000000000001776 ) ;
#15238 = VERTEX_POINT ( 'NONE', #856 ) ;
#15239 = DIRECTION ( 'NONE',  ( 1.000000000000000000, 0.000000000000000000, 0.000000000000000000 ) ) ;
#15240 = CIRCLE ( 'NONE', #20033, 3.000000000000002665 ) ;
#15241 = ORIENTED_EDGE ( 'NONE', *, *, #16507, .F. ) ;
#15242 = DIRECTION ( 'NONE',  ( 0.000000000000000000, 0.000000000000000000, -1.000000000000000000 ) ) ;
#15243 = ORIENTED_EDGE ( 'NONE', *, *, #732, .F. ) ;
#15244 = ORIENTED_EDGE ( 'NONE', *, *, #19858, .F. ) ;
#15245 = CIRCLE ( 'NONE', #10459, 2.000000000000001776 ) ;
#15246 = EDGE_CURVE ( 'NONE', #14320, #26696, #22741, .T. ) ;
#15247 =( NAMED_UNIT ( * ) PLANE_ANGLE_UNIT ( ) SI_UNIT ( $, .RADIAN. ) );
#15248 = CARTESIAN_POINT ( 'NONE',  ( -75.00000337463097821, -8.660254037844422825, -9.999999999999998224 ) ) ;
#15249 = CARTESIAN_POINT ( 'NONE',  ( 6.078523336270777024E-16, 5.773502691896261751, -6.000000000000000000 ) ) ;
#15250 = ORIENTED_EDGE ( 'NONE', *, *, #4924, .F. ) ;
#15251 = ORIENTED_EDGE ( 'NONE', *, *, #4592, .T. ) ;
#15252 = DIRECTION ( 'NONE',  ( 1.000000000000000000, 0.000000000000000000, 0.000000000000000000 ) ) ;
#15253 = CARTESIAN_POINT ( 'NONE',  ( -65.00000337463102085, 43.30127018922198801, -5.000000000000000000 ) ) ;
#15254 = CONTEXT_DEPENDENT_SHAPE_REPRESENTATION ( #2977, #29848 ) ;
#15255 = AXIS2_PLACEMENT_3D ( 'NONE', #34491, #28841, #8800 ) ;
#15256 = CARTESIAN_POINT ( 'NONE',  ( 7.999996625368656744, -69.28203230275519786, -9.999999999999998224 ) ) ;
#15257 = DIRECTION ( 'NONE',  ( -1.000000000000000000, 0.000000000000000000, 0.000000000000000000 ) ) ;
#15258 = CIRCLE ( 'NONE', #20045, 2.000000000000001776 ) ;
#15259 = ORIENTED_EDGE ( 'NONE', *, *, #27551, .T. ) ;
#15260 = DIRECTION ( 'NONE',  ( 0.000000000000000000, 0.000000000000000000, 1.000000000000000000 ) ) ;
#15261 = CARTESIAN_POINT ( 'NONE',  ( 0.000000000000000000, 0.000000000000000000, -5.000000000000000000 ) ) ;
#15262 = ORIENTED_EDGE ( 'NONE', *, *, #4007, .T. ) ;
#15263 = ADVANCED_FACE ( 'NONE', ( #680, #1244 ), #14944, .F. ) ;
#15264 = CARTESIAN_POINT ( 'NONE',  ( 71.99999662536841072, 51.96152422706640550, -5.000000000000000000 ) ) ;
#15265 = DIRECTION ( 'NONE',  ( 1.000000000000000000, 0.000000000000000000, 0.000000000000000000 ) ) ;
#15266 = DIRECTION ( 'NONE',  ( 1.000000000000000000, 0.000000000000000000, 0.000000000000000000 ) ) ;
#15267 = CARTESIAN_POINT ( 'NONE',  ( -15.00000337463125710, -77.94228634059960825, -9.999999999999998224 ) ) ;
#15268 = SHAPE_REPRESENTATION ( 'BR-596', ( #24356, #1599, #6385, #13560, #35119, #23743, #32119, #9974, #3979, #11753, #28516, #27345, #3394, #5781, #9383, #15983, #382, #17157, #32726, #30925, #8771, #14147, #14177, #18953, #34526, #2784, #19568, #36934, #18358, #16569, #14762 ), #26732 ) ;
#15269 = CARTESIAN_POINT ( 'NONE',  ( 70.47608876694671665, 59.13646009116074964, -4.999999999999997335 ) ) ;
#15270 = AXIS2_PLACEMENT_3D ( 'NONE', #1055, #3307, #6685 ) ;
#15271 = CARTESIAN_POINT ( 'NONE',  ( 34.99999662536855283, -77.94228634059960825, -5.000000000000000000 ) ) ;
#15272 = ORIENTED_EDGE ( 'NONE', *, *, #30184, .T. ) ;
#15274 = AXIS2_PLACEMENT_3D ( 'NONE', #2381, #28602, #8177 ) ;
#15273 = DIRECTION ( 'NONE',  ( 1.000000000000000000, 0.000000000000000000, 0.000000000000000000 ) ) ;
#15275 = FACE_OUTER_BOUND ( 'NONE', #1086, .T. ) ;
#15276 = CARTESIAN_POINT ( 'NONE',  ( -106.7731239591695669, -98.28784258492920856, 27.50000000000000000 ) ) ;
#15277 = CIRCLE ( 'NONE', #33268, 2.000000000000000000 ) ;
#15278 = ORIENTED_EDGE ( 'NONE', *, *, #11420, .F. ) ;
#15279 = CIRCLE ( 'NONE', #36245, 2.000000000000001776 ) ;
#15280 = EDGE_LOOP ( 'NONE', ( #21561, #24811 ) ) ;
#15281 = ORIENTED_EDGE ( 'NONE', *, *, #6602, .T. ) ;
#15282 = EDGE_CURVE ( 'NONE', #18446, #36954, #32901, .T. ) ;
#15283 = CARTESIAN_POINT ( 'NONE',  ( 0.000000000000000000, 0.000000000000000000, -5.000000000000000000 ) ) ;
#15284 = CARTESIAN_POINT ( 'NONE',  ( 49.99999662536846756, 69.28203230275516944, 12.50000000000000000 ) ) ;
#15285 = DIRECTION ( 'NONE',  ( 0.000000000000000000, 0.000000000000000000, 1.000000000000000000 ) ) ;
#15286 = AXIS2_PLACEMENT_3D ( 'NONE', #10367, #26886, #35892 ) ;
#15287 = DIRECTION ( 'NONE',  ( 0.000000000000000000, 0.000000000000000000, 1.000000000000000000 ) ) ;
#15288 = CARTESIAN_POINT ( 'NONE',  ( -67.00000337463102085, 25.98076211353317433, 17.49999999999999645 ) ) ;
#15289 = ORIENTED_EDGE ( 'NONE', *, *, #18598, .T. ) ;
#15290 = DIRECTION ( 'NONE',  ( -0.000000000000000000, -0.000000000000000000, -1.000000000000000000 ) ) ;
#15291 = EDGE_CURVE ( 'NONE', #27517, #2978, #26375, .T. ) ;
#15292 = ORIENTED_EDGE ( 'NONE', *, *, #34193, .F. ) ;
#15293 = FACE_BOUND ( 'NONE', #30606, .T. ) ;
#15294 = EDGE_CURVE ( 'NONE', #21781, #16030, #31959, .T. ) ;
#15295 = CARTESIAN_POINT ( 'NONE',  ( -5.000003374631269537, -77.94228634059960825, -9.999999999999998224 ) ) ;
#15296 = CIRCLE ( 'NONE', #20664, 2.000000000000001776 ) ;
#15297 = CARTESIAN_POINT ( 'NONE',  ( 94.55012560584674475, -9.234378588654731601, 32.50000000000000000 ) ) ;
#15298 = AXIS2_PLACEMENT_3D ( 'NONE', #29090, #3428, #26303 ) ;
#15299 = ORIENTED_EDGE ( 'NONE', *, *, #16304, .T. ) ;
#15300 = CYLINDRICAL_SURFACE ( 'NONE', #1481, 2.000000000000001776 ) ;
#15301 = CIRCLE ( 'NONE', #9921, 1.999999999999998224 ) ;
#15302 = DIRECTION ( 'NONE',  ( 0.9311380786261209686, 0.3646668048129080852, 0.000000000000000000 ) ) ;
#15303 = FACE_OUTER_BOUND ( 'NONE', #22523, .T. ) ;
#15304 = CARTESIAN_POINT ( 'NONE',  ( 3.000000000000000000, 2.201436576420042535, 1.270999999999998353 ) ) ;
#15305 = CARTESIAN_POINT ( 'NONE',  ( 0.000000000000000000, 1.467624384280024730, -2.542000000000001592 ) ) ;
#15306 = ORIENTED_EDGE ( 'NONE', *, *, #30353, .F. ) ;
#15307 = DIRECTION ( 'NONE',  ( 1.000000000000000000, 0.000000000000000000, 0.000000000000000000 ) ) ;
#15308 = DIRECTION ( 'NONE',  ( 1.000000000000000000, 0.000000000000000000, 0.000000000000000000 ) ) ;
#15309 = CARTESIAN_POINT ( 'NONE',  ( 9.999996625368625658, 86.60254037844397601, -9.999999999999998224 ) ) ;
#15310 = AXIS2_PLACEMENT_3D ( 'NONE', #13066, #22252, #33119 ) ;
#15311 = VERTEX_POINT ( 'NONE', #12839 ) ;
#15312 = EDGE_CURVE ( 'NONE', #29261, #35651, #16157, .T. ) ;
#15313 = VERTEX_POINT ( 'NONE', #19057 ) ;
#15314 = EDGE_LOOP ( 'NONE', ( #2216, #363 ) ) ;
#15315 = CARTESIAN_POINT ( 'NONE',  ( -35.00000337463116296, -60.62177826491080168, 12.50000000000000000 ) ) ;
#15316 = DIRECTION ( 'NONE',  ( 0.000000000000000000, 0.000000000000000000, 1.000000000000000000 ) ) ;
#15317 = ADVANCED_FACE ( 'NONE', ( #27483 ), #16241, .F. ) ;
#15318 = CARTESIAN_POINT ( 'NONE',  ( 52.99999662536846046, -43.30127018922200222, -5.000000000000000000 ) ) ;
#15319 = AXIS2_PLACEMENT_3D ( 'NONE', #26301, #31890, #32461 ) ;
#15320 = EDGE_CURVE ( 'NONE', #10671, #4910, #16745, .T. ) ;
#15321 = DIRECTION ( 'NONE',  ( 1.000000000000000000, 0.000000000000000000, 0.000000000000000000 ) ) ;
#15322 = CARTESIAN_POINT ( 'NONE',  ( 52.39915983220795681, 35.19434990244919703, 12.49999999999999822 ) ) ;
#15323 = AXIS2_PLACEMENT_3D ( 'NONE', #36768, #16345, #2078 ) ;
#15324 = AXIS2_PLACEMENT_3D ( 'NONE', #35766, #15316, #18698 ) ;
#15325 = FACE_OUTER_BOUND ( 'NONE', #16829, .T. ) ;
#15326 = AXIS2_PLACEMENT_3D ( 'NONE', #4710, #3944, #26830 ) ;
#15327 = ORIENTED_EDGE ( 'NONE', *, *, #10884, .T. ) ;
#15328 = CIRCLE ( 'NONE', #32095, 2.000000000000001776 ) ;
#15329 = ORIENTED_EDGE ( 'NONE', *, *, #30448, .F. ) ;
#15330 = FACE_OUTER_BOUND ( 'NONE', #5623, .T. ) ;
#15331 = CIRCLE ( 'NONE', #34501, 2.000000000000000000 ) ;
#15332 = FACE_OUTER_BOUND ( 'NONE', #4514, .T. ) ;
#15333 = VERTEX_POINT ( 'NONE', #13599 ) ;
#15334 = CARTESIAN_POINT ( 'NONE',  ( -3.417629563432035500, -3.800333343458386359, -3.719399823475301847 ) ) ;
#15335 = ORIENTED_EDGE ( 'NONE', *, *, #3685, .T. ) ;
#15336 = AXIS2_PLACEMENT_3D ( 'NONE', #16450, #10449, #7846 ) ;
#15337 = ADVANCED_FACE ( 'NONE', ( #4808 ), #7244, .F. ) ;
#15338 = CARTESIAN_POINT ( 'NONE',  ( 77.99999662536833966, 34.64101615137759183, -5.000000000000000000 ) ) ;
#15339 = VERTEX_POINT ( 'NONE', #29925 ) ;
#15340 = ORIENTED_EDGE ( 'NONE', *, *, #6003, .F. ) ;
#15341 = FACE_OUTER_BOUND ( 'NONE', #22336, .T. ) ;
#15342 = EDGE_LOOP ( 'NONE', ( #35098, #29837, #10584, #18338, #36926 ) ) ;
#15343 = AXIS2_PLACEMENT_3D ( 'NONE', #26895, #33251, #33066 ) ;
#15344 = CARTESIAN_POINT ( 'NONE',  ( -67.00000337463102085, 60.62177826491077326, 17.49999999999999645 ) ) ;
#15345 = AXIS2_PLACEMENT_3D ( 'NONE', #14269, #28696, #5082 ) ;
#15346 = DIRECTION ( 'NONE',  ( 0.000000000000000000, 0.000000000000000000, -1.000000000000000000 ) ) ;
#15347 = CARTESIAN_POINT ( 'NONE',  ( 59.99999662536845335, 34.64101615137759893, -5.000000000000000000 ) ) ;
#15348 = ORIENTED_EDGE ( 'NONE', *, *, #20207, .T. ) ;
#15349 = ORIENTED_EDGE ( 'NONE', *, *, #30503, .T. ) ;
#15350 = VERTEX_POINT ( 'NONE', #23695 ) ;
#15351 = AXIS2_PLACEMENT_3D ( 'NONE', #31903, #23128, #15228 ) ;
#15352 = CIRCLE ( 'NONE', #36330, 95.00000000000001421 ) ;
#15353 = ORIENTED_EDGE ( 'NONE', *, *, #32263, .F. ) ;
#15354 = AXIS2_PLACEMENT_3D ( 'NONE', #584, #32442, #11627 ) ;
#15355 = VECTOR ( 'NONE', #19532, 1000.000000000000114 ) ;
#15356 = ORIENTED_EDGE ( 'NONE', *, *, #19200, .F. ) ;
#15357 = AXIS2_PLACEMENT_3D ( 'NONE', #6516, #29546, #32551 ) ;
#15358 = EDGE_CURVE ( 'NONE', #34185, #18257, #23243, .T. ) ;
#15359 = EDGE_LOOP ( 'NONE', ( #3909, #21880, #1190, #28404, #21052, #34875, #27840, #30152 ) ) ;
#15360 = DIRECTION ( 'NONE',  ( -0.000000000000000000, -0.000000000000000000, -1.000000000000000000 ) ) ;
#15361 = DIRECTION ( 'NONE',  ( 1.000000000000000000, 0.000000000000000000, 0.000000000000000000 ) ) ;
#15362 = EDGE_CURVE ( 'NONE', #11631, #17956, #13763, .T. ) ;
#15363 = ORIENTED_EDGE ( 'NONE', *, *, #13498, .T. ) ;
#15364 = CYLINDRICAL_SURFACE ( 'NONE', #498, 3.000000000000002665 ) ;
#15365 = CARTESIAN_POINT ( 'NONE',  ( 91.99999662536828282, 0.000000000000000000, -9.999999999999998224 ) ) ;
#15366 = DIRECTION ( 'NONE',  ( 1.000000000000000000, 0.000000000000000000, 0.000000000000000000 ) ) ;
#15367 = EDGE_LOOP ( 'NONE', ( #27349, #18826 ) ) ;
#15368 = CARTESIAN_POINT ( 'NONE',  ( 0.000000000000000000, 3.750000000000001776, 3.400000000000000355 ) ) ;
#15369 = AXIS2_PLACEMENT_3D ( 'NONE', #14341, #19954, #22396 ) ;
#15370 = EDGE_CURVE ( 'NONE', #23192, #28818, #21494, .T. ) ;
#15371 = DIRECTION ( 'NONE',  ( 1.000000000000000000, 0.000000000000000000, 0.000000000000000000 ) ) ;
#15372 = DIRECTION ( 'NONE',  ( -1.000000000000000000, 0.000000000000000000, 0.000000000000000000 ) ) ;
#15373 = ORIENTED_EDGE ( 'NONE', *, *, #17442, .T. ) ;
#15374 = DIRECTION ( 'NONE',  ( -1.000000000000000000, 0.000000000000000000, 0.000000000000000000 ) ) ;
#15375 = EDGE_CURVE ( 'NONE', #11435, #17617, #34729, .T. ) ;
#15376 = DIRECTION ( 'NONE',  ( -1.000000000000000000, -0.000000000000000000, -0.000000000000000000 ) ) ;
#15377 = EDGE_CURVE ( 'NONE', #14541, #8770, #22228, .T. ) ;
#15378 = ORIENTED_EDGE ( 'NONE', *, *, #16584, .F. ) ;
#15379 = CIRCLE ( 'NONE', #31528, 33.00000000000001421 ) ;
#15380 = EDGE_LOOP ( 'NONE', ( #20706, #17889, #7851, #15053, #19636, #22313, #23795 ) ) ;
#15381 = DIRECTION ( 'NONE',  ( -0.000000000000000000, -0.000000000000000000, 1.000000000000000000 ) ) ;
#15382 = CARTESIAN_POINT ( 'NONE',  ( -28.00000337463118427, 69.28203230275516944, -9.999999999999998224 ) ) ;
#15383 = CARTESIAN_POINT ( 'NONE',  ( 62.97617850287784336, 4.279621169095339184, -4.999999999999997335 ) ) ;
#15384 = CARTESIAN_POINT ( 'NONE',  ( -5.000000000000000000, -4.846777557549235459E-18, -0.5080592402122449114 ) ) ;
#15385 = CYLINDRICAL_SURFACE ( 'NONE', #4158, 2.000000000000001776 ) ;
#15386 = VERTEX_POINT ( 'NONE', #10241 ) ;
#15387 = ADVANCED_FACE ( 'NONE', ( #1800 ), #33492, .F. ) ;
#15388 = AXIS2_PLACEMENT_3D ( 'NONE', #12478, #26927, #13041 ) ;
#15390 = AXIS2_PLACEMENT_3D ( 'NONE', #1308, #4496, #12921 ) ;
#15389 = CARTESIAN_POINT ( 'NONE',  ( -78.00000337463094979, -2.428612866367529932E-14, -9.999999999999998224 ) ) ;
#15391 = EDGE_CURVE ( 'NONE', #8516, #14843, #10770, .T. ) ;
#15392 = CARTESIAN_POINT ( 'NONE',  ( 3.351853367131008454, -3.838309248099023296, -6.000000000000000000 ) ) ;
#15393 = CIRCLE ( 'NONE', #36362, 2.000000000000001776 ) ;
#15394 = AXIS2_PLACEMENT_3D ( 'NONE', #29507, #656, #12066 ) ;
#15395 = EDGE_CURVE ( 'NONE', #28847, #26778, #13233, .T. ) ;
#15396 = ORIENTED_EDGE ( 'NONE', *, *, #35294, .F. ) ;
#15397 = EDGE_CURVE ( 'NONE', #13357, #19811, #2982, .T. ) ;
#15398 = ADVANCED_FACE ( 'NONE', ( #33288 ), #7800, .F. ) ;
#15399 = DIRECTION ( 'NONE',  ( -1.000000000000000000, 0.000000000000000000, -0.000000000000000000 ) ) ;
#15400 = ORIENTED_EDGE ( 'NONE', *, *, #21330, .T. ) ;
#15401 = CARTESIAN_POINT ( 'NONE',  ( -73.00000337463099243, -25.98076211353322051, -9.999999999999998224 ) ) ;
#15402 = AXIS2_PLACEMENT_3D ( 'NONE', #20831, #14294, #5857 ) ;
#15403 = DIRECTION ( 'NONE',  ( 1.000000000000000000, 0.000000000000000000, 0.000000000000000000 ) ) ;
#15404 = CARTESIAN_POINT ( 'NONE',  ( 4.828573329308747830, 2.985724580418001928, -1.878862934774779836 ) ) ;
#15405 = ORIENTED_EDGE ( 'NONE', *, *, #27520, .T. ) ;
#15406 = ORIENTED_EDGE ( 'NONE', *, *, #31846, .T. ) ;
#15407 = AXIS2_PLACEMENT_3D ( 'NONE', #31001, #7571, #2677 ) ;
#15408 = CIRCLE ( 'NONE', #1623, 3.000000000000002665 ) ;
#15409 = CIRCLE ( 'NONE', #28571, 27.00000000000001421 ) ;
#15410 = ORIENTED_EDGE ( 'NONE', *, *, #29339, .F. ) ;
#15411 = LINE ( 'NONE', #1164, #14782 ) ;
#15412 = LINE ( 'NONE', #24208, #5983 ) ;
#15413 = CARTESIAN_POINT ( 'NONE',  ( -90.00000337463090716, -1.040834085586084257E-14, -5.000000000000000000 ) ) ;
#15414 = DIRECTION ( 'NONE',  ( 0.000000000000000000, 0.000000000000000000, -1.000000000000000000 ) ) ;
#15415 = FACE_OUTER_BOUND ( 'NONE', #9166, .T. ) ;
#15416 = CIRCLE ( 'NONE', #36386, 2.000000000000001776 ) ;
#15417 = VERTEX_POINT ( 'NONE', #253 ) ;
#15418 = DIRECTION ( 'NONE',  ( 1.000000000000000000, 0.000000000000000000, 0.000000000000000000 ) ) ;
#15419 = AXIS2_PLACEMENT_3D ( 'NONE', #10037, #4238, #36283 ) ;
#15420 = CIRCLE ( 'NONE', #32184, 2.000000000000001776 ) ;
#15421 = FACE_OUTER_BOUND ( 'NONE', #20049, .T. ) ;
#15422 = FACE_OUTER_BOUND ( 'NONE', #10701, .T. ) ;
#15423 = EDGE_LOOP ( 'NONE', ( #20402, #28021, #25070, #34420 ) ) ;
#15424 = CARTESIAN_POINT ( 'NONE',  ( -55.00000337463107059, 60.62177826491078747, -9.999999999999998224 ) ) ;
#15425 = DIRECTION ( 'NONE',  ( 1.000000000000000000, 0.000000000000000000, 0.000000000000000000 ) ) ;
#15426 = DIRECTION ( 'NONE',  ( 0.000000000000000000, 0.000000000000000000, -1.000000000000000000 ) ) ;
#15427 = VECTOR ( 'NONE', #27498, 1000.000000000000000 ) ;
#15428 = VERTEX_POINT ( 'NONE', #5163 ) ;
#15429 = ORIENTED_EDGE ( 'NONE', *, *, #27225, .F. ) ;
#15430 = AXIS2_PLACEMENT_3D ( 'NONE', #30040, #3794, #4361 ) ;
#15431 = DIRECTION ( 'NONE',  ( -0.8660254037844380415, 0.5000000000000009992, 0.000000000000000000 ) ) ;
#15432 = DIRECTION ( 'NONE',  ( -0.000000000000000000, -0.000000000000000000, -1.000000000000000000 ) ) ;
#15433 = CARTESIAN_POINT ( 'NONE',  ( -45.00000337463111322, 77.94228634059959404, -9.999999999999998224 ) ) ;
#15434 = VERTEX_POINT ( 'NONE', #16604 ) ;
#15435 = ORIENTED_EDGE ( 'NONE', *, *, #18774, .F. ) ;
#15436 = CIRCLE ( 'NONE', #32802, 2.000000000000001776 ) ;
#15437 = CIRCLE ( 'NONE', #14841, 2.000000000000001776 ) ;
#15438 = VERTEX_POINT ( 'NONE', #14345 ) ;
#15439 = AXIS2_PLACEMENT_3D ( 'NONE', #402, #14851, #17475 ) ;
#15440 = DIRECTION ( 'NONE',  ( 0.000000000000000000, 0.000000000000000000, 1.000000000000000000 ) ) ;
#15441 = AXIS2_PLACEMENT_3D ( 'NONE', #4181, #15049, #18043 ) ;
#15442 = ORIENTED_EDGE ( 'NONE', *, *, #11222, .F. ) ;
#15443 = ADVANCED_FACE ( 'NONE', ( #28769 ), #5365, .F. ) ;
#15444 = VERTEX_POINT ( 'NONE', #31215 ) ;
#15445 = DIRECTION ( 'NONE',  ( 0.000000000000000000, 0.000000000000000000, -1.000000000000000000 ) ) ;
#15446 = ORIENTED_EDGE ( 'NONE', *, *, #26190, .T. ) ;
#15447 = ORIENTED_EDGE ( 'NONE', *, *, #1519, .F. ) ;
#15448 = AXIS2_PLACEMENT_3D ( 'NONE', #30958, #23025, #36916 ) ;
#15449 = CARTESIAN_POINT ( 'NONE',  ( 67.99999662536838230, 34.64101615137758472, -9.999999999999998224 ) ) ;
#15450 = LINE ( 'NONE', #19008, #10497 ) ;
#15451 = ORIENTED_EDGE ( 'NONE', *, *, #494, .T. ) ;
#15452 = EDGE_LOOP ( 'NONE', ( #6080, #1596, #13696, #11168 ) ) ;
#15453 = DIRECTION ( 'NONE',  ( 0.000000000000000000, 0.000000000000000000, 1.000000000000000000 ) ) ;
#15454 = VECTOR ( 'NONE', #2173, 1000.000000000000000 ) ;
#15455 = CARTESIAN_POINT ( 'NONE',  ( -82.00000337463094979, -2.404119930384582903E-14, 17.49999999999999645 ) ) ;
#15456 = CARTESIAN_POINT ( 'NONE',  ( 56.99999662536844625, 43.30127018922198801, -9.999999999999998224 ) ) ;
#15457 = LINE ( 'NONE', #7015, #22070 ) ;
#15458 = ORIENTED_EDGE ( 'NONE', *, *, #5572, .T. ) ;
#15459 = CARTESIAN_POINT ( 'NONE',  ( 6.999996625368645198, 77.94228634059957983, -9.999999999999998224 ) ) ;
#15461 = CIRCLE ( 'NONE', #5883, 3.000000000000002665 ) ;
#15460 = CARTESIAN_POINT ( 'NONE',  ( -62.00000337463104927, 51.96152422706639129, -9.999999999999998224 ) ) ;
#15462 = ORIENTED_EDGE ( 'NONE', *, *, #2958, .T. ) ;
#15463 = CARTESIAN_POINT ( 'NONE',  ( 21.99999662536862033, -86.60254037844400443, -5.000000000000000000 ) ) ;
#15464 = CONICAL_SURFACE ( 'NONE', #2298, 5.000000000000000888, 1.047197551196596299 ) ;
#15465 = CIRCLE ( 'NONE', #12475, 33.00000000000001421 ) ;
#15466 = DIRECTION ( 'NONE',  ( 0.000000000000000000, 0.000000000000000000, 1.000000000000000000 ) ) ;
#15467 = CARTESIAN_POINT ( 'NONE',  ( -56.67878100130369035, 27.78182860042797131, -49.86348611802629449 ) ) ;
#15468 = ADVANCED_FACE ( 'NONE', ( #2917 ), #20341, .T. ) ;
#15469 = DIRECTION ( 'NONE',  ( 1.000000000000000000, 0.000000000000000000, 0.000000000000000000 ) ) ;
#15470 = DIRECTION ( 'NONE',  ( 0.000000000000000000, 0.000000000000000000, -1.000000000000000000 ) ) ;
#15471 = AXIS2_PLACEMENT_3D ( 'NONE', #6374, #26438, #23621 ) ;
#15472 = CARTESIAN_POINT ( 'NONE',  ( -18.00000337463123046, 86.60254037844397601, 17.49999999999999645 ) ) ;
#15473 = ORIENTED_EDGE ( 'NONE', *, *, #7925, .F. ) ;
#15474 = DIRECTION ( 'NONE',  ( 0.000000000000000000, 0.000000000000000000, 1.000000000000000000 ) ) ;
#15475 = LINE ( 'NONE', #29701, #15958 ) ;
#15476 = DIRECTION ( 'NONE',  ( 1.000000000000000000, 0.000000000000000000, 0.000000000000000000 ) ) ;
#15477 = VERTEX_POINT ( 'NONE', #8157 ) ;
#15478 = EDGE_CURVE ( 'NONE', #3872, #21416, #36528, .T. ) ;
#15479 = AXIS2_PLACEMENT_3D ( 'NONE', #36450, #7936, #10760 ) ;
#15480 = VERTEX_POINT ( 'NONE', #11343 ) ;
#15481 = ORIENTED_EDGE ( 'NONE', *, *, #8613, .T. ) ;
#15482 = DIRECTION ( 'NONE',  ( 0.000000000000000000, 0.000000000000000000, 1.000000000000000000 ) ) ;
#15483 = DIRECTION ( 'NONE',  ( -1.000000000000000000, 0.000000000000000000, -0.000000000000000000 ) ) ;
#15484 = DIRECTION ( 'NONE',  ( -0.5000000000000094369, -0.8660254037844332675, 0.000000000000000000 ) ) ;
#15485 = VECTOR ( 'NONE', #34195, 1000.000000000000000 ) ;
#15486 = PRODUCT_DEFINITION_SHAPE ( 'NONE', 'NONE',  #37129 ) ;
#15487 = DIRECTION ( 'NONE',  ( 1.000000000000000000, 0.000000000000000000, 0.000000000000000000 ) ) ;
#15488 = VECTOR ( 'NONE', #8444, 1000.000000000000114 ) ;
#15489 = CARTESIAN_POINT ( 'NONE',  ( 74.99999662536836809, 43.30127018922198801, 17.49999999999999645 ) ) ;
#15490 = ORIENTED_EDGE ( 'NONE', *, *, #14603, .F. ) ;
#15491 = EDGE_CURVE ( 'NONE', #36272, #24938, #18563, .T. ) ;
#15492 = CARTESIAN_POINT ( 'NONE',  ( 0.000000000000000000, 55.00000000000000000, -5.000000000000000000 ) ) ;
#15493 = ORIENTED_EDGE ( 'NONE', *, *, #35963, .T. ) ;
#15494 = VECTOR ( 'NONE', #26692, 1000.000000000000000 ) ;
#15495 = FACE_BOUND ( 'NONE', #6029, .T. ) ;
#15496 = CARTESIAN_POINT ( 'NONE',  ( 19.99999662536861678, -86.60254037844400443, -5.000000000000000000 ) ) ;
#15497 = CONICAL_SURFACE ( 'NONE', #36462, 2.541999999999999815, 1.047197551196591858 ) ;
#15498 = FACE_OUTER_BOUND ( 'NONE', #26820, .T. ) ;
#15499 = DIRECTION ( 'NONE',  ( 0.000000000000000000, 0.000000000000000000, -1.000000000000000000 ) ) ;
#15500 = ORIENTED_EDGE ( 'NONE', *, *, #1887, .F. ) ;
#15501 = CARTESIAN_POINT ( 'NONE',  ( 5.000000000000000000, 2.886751345948137981, -5.553418012614792509 ) ) ;
#15502 = VECTOR ( 'NONE', #33381, 1000.000000000000000 ) ;
#15503 = DIRECTION ( 'NONE',  ( -0.000000000000000000, -0.000000000000000000, 1.000000000000000000 ) ) ;
#15504 = VECTOR ( 'NONE', #29633, 999.9999999999998863 ) ;
#15505 = DIRECTION ( 'NONE',  ( -1.000000000000000000, 0.000000000000000000, 0.000000000000000000 ) ) ;
#15506 = DIRECTION ( 'NONE',  ( -0.7650473262243671080, -0.6439740589782688707, -0.000000000000000000 ) ) ;
#15507 = ADVANCED_FACE ( 'NONE', ( #11689 ), #22795, .F. ) ;
#15508 = VERTEX_POINT ( 'NONE', #22399 ) ;
#15509 = CYLINDRICAL_SURFACE ( 'NONE', #1641, 150.0000000000000284 ) ;
#15510 = CARTESIAN_POINT ( 'NONE',  ( -15.00000337463125710, -77.94228634059960825, 17.49999999999999645 ) ) ;
#15511 = DIRECTION ( 'NONE',  ( -1.000000000000000000, 0.000000000000000000, 0.000000000000000000 ) ) ;
#15512 = EDGE_CURVE ( 'NONE', #32313, #19796, #25956, .T. ) ;
#15513 = ORIENTED_EDGE ( 'NONE', *, *, #23416, .T. ) ;
#15514 = ORIENTED_EDGE ( 'NONE', *, *, #24453, .T. ) ;
#15515 = AXIS2_PLACEMENT_3D ( 'NONE', #31086, #5414, #24911 ) ;
#15516 = ORIENTED_EDGE ( 'NONE', *, *, #10549, .F. ) ;
#15517 = EDGE_CURVE ( 'NONE', #4478, #23649, #34595, .T. ) ;
#15518 = AXIS2_PLACEMENT_3D ( 'NONE', #25012, #5495, #10756 ) ;
#15519 = DIRECTION ( 'NONE',  ( -1.000000000000000000, 0.000000000000000000, 0.000000000000000000 ) ) ;
#15520 = CARTESIAN_POINT ( 'NONE',  ( 64.99999662536841072, 25.98076211353318854, -5.000000000000000000 ) ) ;
#15521 = FACE_OUTER_BOUND ( 'NONE', #14685, .T. ) ;
#15522 = EDGE_CURVE ( 'NONE', #18158, #8626, #37001, .T. ) ;
#15523 = CIRCLE ( 'NONE', #8909, 1.999999999999998224 ) ;
#15524 = DIRECTION ( 'NONE',  ( 1.000000000000000000, 0.000000000000000000, 0.000000000000000000 ) ) ;
#15525 = DIRECTION ( 'NONE',  ( 0.000000000000000000, 0.000000000000000000, 1.000000000000000000 ) ) ;
#15527 = CARTESIAN_POINT ( 'NONE',  ( -28.00000337463118427, 69.28203230275516944, -5.000000000000000000 ) ) ;
#15526 = CIRCLE ( 'NONE', #19155, 2.000000000000000000 ) ;
#15528 = ORIENTED_EDGE ( 'NONE', *, *, #13653, .T. ) ;
#15529 = EDGE_LOOP ( 'NONE', ( #25790, #15607 ) ) ;
#15530 = FILL_AREA_STYLE ('',( #4094 ) ) ;
#15531 = CARTESIAN_POINT ( 'NONE',  ( -71.20512444582767841, -36.23716251175871861, -5.000000000000000000 ) ) ;
#15532 = ORIENTED_EDGE ( 'NONE', *, *, #28451, .F. ) ;
#15533 = CIRCLE ( 'NONE', #2377, 2.000000000000001776 ) ;
#15534 = DIRECTION ( 'NONE',  ( 0.000000000000000000, 0.000000000000000000, -1.000000000000000000 ) ) ;
#15535 = ORIENTED_EDGE ( 'NONE', *, *, #34088, .F. ) ;
#15536 = DIRECTION ( 'NONE',  ( -0.000000000000000000, -0.000000000000000000, 1.000000000000000000 ) ) ;
#15537 = EDGE_CURVE ( 'NONE', #10828, #17104, #15420, .T. ) ;
#15538 = AXIS2_PLACEMENT_3D ( 'NONE', #2452, #19695, #30743 ) ;
#15539 = DIRECTION ( 'NONE',  ( 1.000000000000000000, 0.000000000000000000, 0.000000000000000000 ) ) ;
#15540 = AXIS2_PLACEMENT_3D ( 'NONE', #30300, #33854, #10970 ) ;
#15541 = VERTEX_POINT ( 'NONE', #28387 ) ;
#15542 = EDGE_LOOP ( 'NONE', ( #14971, #22590, #6816, #3677 ) ) ;
#15543 = AXIS2_PLACEMENT_3D ( 'NONE', #2412, #8217, #124 ) ;
#15544 = CARTESIAN_POINT ( 'NONE',  ( -82.00000337463094979, -17.32050807568882078, 17.49999999999999645 ) ) ;
#15545 = ORIENTED_EDGE ( 'NONE', *, *, #8537, .F. ) ;
#15546 = EDGE_CURVE ( 'NONE', #33148, #20492, #20211, .T. ) ;
#15547 = DIRECTION ( 'NONE',  ( 0.5000000000000039968, 0.8660254037844363761, 0.000000000000000000 ) ) ;
#15548 = DIRECTION ( 'NONE',  ( -0.000000000000000000, -0.000000000000000000, 1.000000000000000000 ) ) ;
#15549 = CARTESIAN_POINT ( 'NONE',  ( -27.78182860042817026, -56.67878100130359087, -4.999999999999997335 ) ) ;
#15550 = EDGE_CURVE ( 'NONE', #24230, #22827, #28582, .T. ) ;
#15551 = ORIENTED_EDGE ( 'NONE', *, *, #13155, .T. ) ;
#15552 = AXIS2_PLACEMENT_3D ( 'NONE', #14338, #2908, #2527 ) ;
#15553 = ORIENTED_EDGE ( 'NONE', *, *, #30114, .T. ) ;
#15554 = ORIENTED_EDGE ( 'NONE', *, *, #18978, .T. ) ;
#15555 = ORIENTED_EDGE ( 'NONE', *, *, #7506, .T. ) ;
#15556 = CARTESIAN_POINT ( 'NONE',  ( -45.00000337463111322, 77.94228634059959404, -9.999999999999998224 ) ) ;
#15557 = CIRCLE ( 'NONE', #4193, 2.000000000000001776 ) ;
#15558 = DIRECTION ( 'NONE',  ( 1.000000000000000000, 0.000000000000000000, 0.000000000000000000 ) ) ;
#15559 = EDGE_LOOP ( 'NONE', ( #1586, #13091, #1256, #20141 ) ) ;
#15560 = CARTESIAN_POINT ( 'NONE',  ( 31.46585318596250502, 86.45172111230321832, -49.86348611802629449 ) ) ;
#15561 = PLANE ( 'NONE',  #18753 ) ;
#15562 = CIRCLE ( 'NONE', #20940, 19.53925848833874213 ) ;
#15563 = PLANE ( 'NONE',  #36351 ) ;
#15564 = ORIENTED_EDGE ( 'NONE', *, *, #15723, .F. ) ;
#15565 = DIRECTION ( 'NONE',  ( 0.000000000000000000, 0.000000000000000000, -1.000000000000000000 ) ) ;
#15566 = CARTESIAN_POINT ( 'NONE',  ( -31.74999999999995737, 0.000000000000000000, 0.000000000000000000 ) ) ;
#15567 = EDGE_CURVE ( 'NONE', #7036, #21808, #35218, .T. ) ;
#15568 = VECTOR ( 'NONE', #34963, 1000.000000000000000 ) ;
#15569 = FACE_OUTER_BOUND ( 'NONE', #20984, .T. ) ;
#15570 = VERTEX_POINT ( 'NONE', #33847 ) ;
#15571 = DIRECTION ( 'NONE',  ( -1.000000000000000000, 0.000000000000000000, 0.000000000000000000 ) ) ;
#15572 = AXIS2_PLACEMENT_3D ( 'NONE', #24910, #30339, #25111 ) ;
#15573 = CARTESIAN_POINT ( 'NONE',  ( 56.67878100130369035, -27.78182860042797131, -49.86348611802629449 ) ) ;
#15574 = VERTEX_POINT ( 'NONE', #16961 ) ;
#15575 = ORIENTED_EDGE ( 'NONE', *, *, #34118, .F. ) ;
#15576 = DIRECTION ( 'NONE',  ( 0.000000000000000000, 0.000000000000000000, 1.000000000000000000 ) ) ;
#15577 = LINE ( 'NONE', #27570, #12118 ) ;
#15578 = CARTESIAN_POINT ( 'NONE',  ( 59.99999662536843914, -34.64101615137759893, -5.000000000000000000 ) ) ;
#15579 = CARTESIAN_POINT ( 'NONE',  ( -50.00000337463109190, 69.28203230275518365, 12.50000000000000000 ) ) ;
#15580 = EDGE_LOOP ( 'NONE', ( #22913, #23591, #16150, #3627, #10650 ) ) ;
#15581 = UNCERTAINTY_MEASURE_WITH_UNIT (LENGTH_MEASURE( 1.000000000000000082E-05 ), #26744, 'distance_accuracy_value', 'NONE');
#15582 = VECTOR ( 'NONE', #4802, 1000.000000000000000 ) ;
#15583 = DIRECTION ( 'NONE',  ( 0.000000000000000000, 0.000000000000000000, 1.000000000000000000 ) ) ;
#15584 = DIRECTION ( 'NONE',  ( -0.000000000000000000, -0.000000000000000000, 1.000000000000000000 ) ) ;
#15585 = EDGE_CURVE ( 'NONE', #15870, #698, #28034, .T. ) ;
#15586 = ORIENTED_EDGE ( 'NONE', *, *, #4972, .T. ) ;
#15587 = EDGE_CURVE ( 'NONE', #32894, #2284, #30406, .T. ) ;
#15588 = CARTESIAN_POINT ( 'NONE',  ( 22.99999662536857059, 77.94228634059957983, -9.999999999999998224 ) ) ;
#15589 = ORIENTED_EDGE ( 'NONE', *, *, #24044, .F. ) ;
#15590 = DIRECTION ( 'NONE',  ( 0.000000000000000000, 0.000000000000000000, -1.000000000000000000 ) ) ;
#15591 = EDGE_CURVE ( 'NONE', #22677, #18010, #35801, .T. ) ;
#15592 = CARTESIAN_POINT ( 'NONE',  ( 71.99999662536838230, -51.96152422706639840, 17.49999999999999645 ) ) ;
#15593 = AXIS2_PLACEMENT_3D ( 'NONE', #20399, #17967, #18138 ) ;
#15594 = CARTESIAN_POINT ( 'NONE',  ( 6.999996625368676284, -77.94228634059960825, -9.999999999999998224 ) ) ;
#15595 = EDGE_CURVE ( 'NONE', #28024, #26731, #16542, .T. ) ;
#15596 = ORIENTED_EDGE ( 'NONE', *, *, #18949, .F. ) ;
#15597 = EDGE_LOOP ( 'NONE', ( #26785, #16598, #3994, #8457 ) ) ;
#15598 = EDGE_CURVE ( 'NONE', #13211, #33059, #17509, .T. ) ;
#15599 = ORIENTED_EDGE ( 'NONE', *, *, #1203, .T. ) ;
#15600 = DIRECTION ( 'NONE',  ( 1.000000000000000000, 0.000000000000000000, 0.000000000000000000 ) ) ;
#15601 = CYLINDRICAL_SURFACE ( 'NONE', #17361, 2.000000000000001776 ) ;
#15602 = CIRCLE ( 'NONE', #17396, 2.000000000000001776 ) ;
#15603 = CARTESIAN_POINT ( 'NONE',  ( -60.00000337463107059, -34.64101615137762025, -9.999999999999998224 ) ) ;
#15604 = DIRECTION ( 'NONE',  ( 1.000000000000000000, 0.000000000000000000, 0.000000000000000000 ) ) ;
#15605 = CYLINDRICAL_SURFACE ( 'NONE', #17154, 2.000000000000001776 ) ;
#15606 = EDGE_CURVE ( 'NONE', #35441, #31631, #6455, .T. ) ;
#15607 = ORIENTED_EDGE ( 'NONE', *, *, #17116, .F. ) ;
#15608 = CARTESIAN_POINT ( 'NONE',  ( 4.999999999999999112, 2.886751345948153968, -0.5999999999999998668 ) ) ;
#15609 = EDGE_CURVE ( 'NONE', #30886, #36051, #4674, .T. ) ;
#15610 = CARTESIAN_POINT ( 'NONE',  ( -65.00000337463102085, 25.98076211353317433, 17.49999999999999645 ) ) ;
#15611 = ADVANCED_FACE ( 'NONE', ( #12430 ), #21062, .T. ) ;
#15612 = AXIS2_PLACEMENT_3D ( 'NONE', #36417, #27598, #22518 ) ;
#15613 = DIRECTION ( 'NONE',  ( 1.000000000000000000, 0.000000000000000000, 0.000000000000000000 ) ) ;
#15614 = ORIENTED_EDGE ( 'NONE', *, *, #6352, .T. ) ;
#15615 = B_SPLINE_CURVE_WITH_KNOTS ( 'NONE', 3,
 ( #31345, #14307, #8663, #33807, #16761, #28181 ),
 .UNSPECIFIED., .F., .F.,
 ( 4, 2, 4 ),
 ( 0.002950759650825675751, 0.004429055062152274097, 0.005907350473478872009 ),
 .UNSPECIFIED. ) ;
#15616 = CARTESIAN_POINT ( 'NONE',  ( 0.000000000000000000, 0.000000000000000000, 15.00000000000000000 ) ) ;
#15617 = DIRECTION ( 'NONE',  ( 1.000000000000000000, 0.000000000000000000, 0.000000000000000000 ) ) ;
#15618 = DIRECTION ( 'NONE',  ( 0.000000000000000000, 0.000000000000000000, 1.000000000000000000 ) ) ;
#15619 = ORIENTED_EDGE ( 'NONE', *, *, #3035, .F. ) ;
#15620 = VERTEX_POINT ( 'NONE', #12222 ) ;
#15621 = LINE ( 'NONE', #10534, #1334 ) ;
#15622 = CARTESIAN_POINT ( 'NONE',  ( -15.00000337463125710, -77.94228634059960825, -9.999999999999998224 ) ) ;
#15623 = DIRECTION ( 'NONE',  ( -1.000000000000000000, 0.000000000000000000, 0.000000000000000000 ) ) ;
#15624 = VERTEX_POINT ( 'NONE', #14695 ) ;
#15625 = VERTEX_POINT ( 'NONE', #15449 ) ;
#15626 = VERTEX_POINT ( 'NONE', #641 ) ;
#15627 = DIRECTION ( 'NONE',  ( 1.000000000000000000, 0.000000000000000000, 0.000000000000000000 ) ) ;
#15628 = EDGE_CURVE ( 'NONE', #10938, #28829, #448, .T. ) ;
#15629 = EDGE_LOOP ( 'NONE', ( #8581, #25505 ) ) ;
#15630 = EDGE_CURVE ( 'NONE', #14791, #26021, #12051, .T. ) ;
#15631 = ORIENTED_EDGE ( 'NONE', *, *, #16052, .F. ) ;
#15632 = DIRECTION ( 'NONE',  ( 0.000000000000000000, 0.000000000000000000, 1.000000000000000000 ) ) ;
#15633 = VERTEX_POINT ( 'NONE', #34780 ) ;
#15634 = EDGE_LOOP ( 'NONE', ( #15405, #5356, #20989, #7953 ) ) ;
#15635 = PLANE ( 'NONE',  #14240 ) ;
#15636 = CARTESIAN_POINT ( 'NONE',  ( -40.99999999999999289, -103.4105893997321743, 32.50000000000000000 ) ) ;
#15637 = ORIENTED_EDGE ( 'NONE', *, *, #23774, .F. ) ;
#15638 = ORIENTED_EDGE ( 'NONE', *, *, #13926, .F. ) ;
#15639 = ADVANCED_FACE ( 'NONE', ( #32490 ), #26687, .F. ) ;
#15640 = DIRECTION ( 'NONE',  ( 0.000000000000000000, 0.000000000000000000, 1.000000000000000000 ) ) ;
#15641 = CARTESIAN_POINT ( 'NONE',  ( -80.00000337463094979, 17.32050807568878525, -5.000000000000000000 ) ) ;
#15642 = CARTESIAN_POINT ( 'NONE',  ( -33.21453780030408609, 78.84345928898012801, -5.000000000000000000 ) ) ;
#15643 = DIRECTION ( 'NONE',  ( 0.000000000000000000, 0.000000000000000000, 1.000000000000000000 ) ) ;
#15644 = ORIENTED_EDGE ( 'NONE', *, *, #22942, .T. ) ;
#15645 = CARTESIAN_POINT ( 'NONE',  ( 36.99999662536855283, -77.94228634059960825, -9.999999999999998224 ) ) ;
#15646 = ORIENTED_EDGE ( 'NONE', *, *, #6463, .T. ) ;
#15647 = DIRECTION ( 'NONE',  ( 1.000000000000000000, 0.000000000000000000, 0.000000000000000000 ) ) ;
#15648 = CARTESIAN_POINT ( 'NONE',  ( -80.00000337463094979, -2.428612866367529932E-14, -9.999999999999998224 ) ) ;
#15649 = CARTESIAN_POINT ( 'NONE',  ( -47.63139720814438505, -27.49999999999955591, -10.00000000000000000 ) ) ;
#15650 = FACE_OUTER_BOUND ( 'NONE', #14364, .T. ) ;
#15651 = ADVANCED_FACE ( 'NONE', ( #20333 ), #9248, .T. ) ;
#15652 = DIRECTION ( 'NONE',  ( 1.000000000000000000, 0.000000000000000000, 0.000000000000000000 ) ) ;
#15653 = EDGE_CURVE ( 'NONE', #19903, #28212, #18423, .T. ) ;
#15654 = DIRECTION ( 'NONE',  ( 0.000000000000000000, 0.000000000000000000, 1.000000000000000000 ) ) ;
#15655 = ADVANCED_FACE ( 'NONE', ( #20495, #29320, #31918, #26500, #3644, #814, #23696, #6637, #1006 ), #30053, .F. ) ;
#15656 = ADVANCED_FACE ( 'NONE', ( #7004 ), #2107, .F. ) ;
#15657 = DIRECTION ( 'NONE',  ( 0.000000000000000000, 0.000000000000000000, 1.000000000000000000 ) ) ;
#15658 = ORIENTED_EDGE ( 'NONE', *, *, #30008, .T. ) ;
#15659 = CARTESIAN_POINT ( 'NONE',  ( -5.000000000000000000, 0.000000000000000000, -6.000000000000000000 ) ) ;
#15660 = AXIS2_PLACEMENT_3D ( 'NONE', #847, #22481, #25687 ) ;
#15661 = CYLINDRICAL_SURFACE ( 'NONE', #8753, 2.000000000000001776 ) ;
#15662 = CARTESIAN_POINT ( 'NONE',  ( 0.000000000000000000, 0.000000000000000000, 15.00000000000000000 ) ) ;
#15663 = ORIENTED_EDGE ( 'NONE', *, *, #487, .F. ) ;
#15664 = ORIENTED_EDGE ( 'NONE', *, *, #5273, .F. ) ;
#15665 = ORIENTED_EDGE ( 'NONE', *, *, #10591, .T. ) ;
#15666 = CARTESIAN_POINT ( 'NONE',  ( 5.999999999999999112, 0.000000000000000000, -3.250000000000001332 ) ) ;
#15667 = DIRECTION ( 'NONE',  ( 0.000000000000000000, 0.000000000000000000, -1.000000000000000000 ) ) ;
#15668 = CARTESIAN_POINT ( 'NONE',  ( 108.3061974404898820, 19.22934205794938478, 32.50000000000000000 ) ) ;
#15669 = VERTEX_POINT ( 'NONE', #29876 ) ;
#15670 = DIRECTION ( 'NONE',  ( 1.000000000000000000, 0.000000000000000000, 0.000000000000000000 ) ) ;
#15671 = LINE ( 'NONE', #848, #9325 ) ;
#15672 = ORIENTED_EDGE ( 'NONE', *, *, #10349, .F. ) ;
#15673 =( REPRESENTATION_RELATIONSHIP ('NONE','NONE', #15268, #22738 ) REPRESENTATION_RELATIONSHIP_WITH_TRANSFORMATION ( #25797 )SHAPE_REPRESENTATION_RELATIONSHIP( ) );
#15674 = DIRECTION ( 'NONE',  ( 1.000000000000000000, 0.000000000000000000, 0.000000000000000000 ) ) ;
#15675 = ORIENTED_EDGE ( 'NONE', *, *, #6707, .F. ) ;
#15676 = FACE_BOUND ( 'NONE', #4333, .T. ) ;
#15677 = ADVANCED_FACE ( 'NONE', ( #18638 ), #15635, .T. ) ;
#15678 = LINE ( 'NONE', #27482, #14209 ) ;
#15679 = DIRECTION ( 'NONE',  ( 1.000000000000000000, 0.000000000000000000, 0.000000000000000000 ) ) ;
#15680 = AXIS2_PLACEMENT_3D ( 'NONE', #259, #23518, #28941 ) ;
#15681 = PLANE ( 'NONE',  #24772 ) ;
#15682 = ORIENTED_EDGE ( 'NONE', *, *, #2366, .F. ) ;
#15683 = CARTESIAN_POINT ( 'NONE',  ( 44.99999662536849598, 60.62177826491077326, -5.000000000000000000 ) ) ;
#15684 = AXIS2_PLACEMENT_3D ( 'NONE', #21381, #15191, #579 ) ;
#15685 = CONTEXT_DEPENDENT_SHAPE_REPRESENTATION ( #6086, #18785 ) ;
#15686 = DIRECTION ( 'NONE',  ( 0.000000000000000000, 0.000000000000000000, 1.000000000000000000 ) ) ;
#15687 = CARTESIAN_POINT ( 'NONE',  ( 0.000000000000000000, 0.000000000000000000, -6.000000000000000000 ) ) ;
#15688 = DIRECTION ( 'NONE',  ( 1.000000000000000000, 0.000000000000000000, 0.000000000000000000 ) ) ;
#15689 = VERTEX_POINT ( 'NONE', #7558 ) ;
#15690 = DIRECTION ( 'NONE',  ( 1.000000000000000000, 0.000000000000000000, 0.000000000000000000 ) ) ;
#15691 = LINE ( 'NONE', #23957, #22644 ) ;
#15692 = DIRECTION ( 'NONE',  ( 1.000000000000000000, 0.000000000000000000, 0.000000000000000000 ) ) ;
#15693 = VERTEX_POINT ( 'NONE', #21443 ) ;
#15694 = EDGE_CURVE ( 'NONE', #13344, #15444, #6453, .T. ) ;
#15695 = ORIENTED_EDGE ( 'NONE', *, *, #32355, .T. ) ;
#15696 = CARTESIAN_POINT ( 'NONE',  ( -2.448772250512182280E-15, 99.94802294027086020, -19.99999999999999645 ) ) ;
#15697 = DIRECTION ( 'NONE',  ( 1.000000000000000000, 0.000000000000000000, 0.000000000000000000 ) ) ;
#15698 = CARTESIAN_POINT ( 'NONE',  ( 57.99999662536844625, 34.64101615137759893, 17.49999999999999645 ) ) ;
#15699 = ORIENTED_EDGE ( 'NONE', *, *, #16710, .T. ) ;
#15700 = AXIS2_PLACEMENT_3D ( 'NONE', #57, #34204, #11111 ) ;
#15701 = LINE ( 'NONE', #30516, #25987 ) ;
#15702 = DIRECTION ( 'NONE',  ( -0.000000000000000000, -0.000000000000000000, 1.000000000000000000 ) ) ;
#15703 = CARTESIAN_POINT ( 'NONE',  ( 79.99999662536832545, -17.32050807568879591, -9.999999999999998224 ) ) ;
#15704 = CARTESIAN_POINT ( 'NONE',  ( 64.99999662536842493, 43.30127018922200222, -9.999999999999998224 ) ) ;
#15705 = ORIENTED_EDGE ( 'NONE', *, *, #19738, .T. ) ;
#15706 = ORIENTED_EDGE ( 'NONE', *, *, #36207, .T. ) ;
#15707 = DIRECTION ( 'NONE',  ( -1.000000000000000000, 0.000000000000000000, -0.000000000000000000 ) ) ;
#15708 = DIRECTION ( 'NONE',  ( 1.000000000000000000, 0.000000000000000000, 0.000000000000000000 ) ) ;
#15709 = EDGE_LOOP ( 'NONE', ( #13454, #35473, #27691, #1503 ) ) ;
#15710 = DIRECTION ( 'NONE',  ( 0.000000000000000000, 0.000000000000000000, -1.000000000000000000 ) ) ;
#15711 = ORIENTED_EDGE ( 'NONE', *, *, #29562, .F. ) ;
#15712 = CARTESIAN_POINT ( 'NONE',  ( -59.13646009116099833, 70.47608876694653190, -4.999999999999997335 ) ) ;
#15713 = EDGE_CURVE ( 'NONE', #12842, #31614, #23829, .T. ) ;
#15714 = AXIS2_PLACEMENT_3D ( 'NONE', #24198, #12745, #33188 ) ;
#15715 = CIRCLE ( 'NONE', #3744, 33.00000000000001421 ) ;
#15716 = FACE_BOUND ( 'NONE', #4107, .T. ) ;
#15717 = ORIENTED_EDGE ( 'NONE', *, *, #18375, .F. ) ;
#15718 = ORIENTED_EDGE ( 'NONE', *, *, #36489, .F. ) ;
#15719 = PRODUCT_RELATED_PRODUCT_CATEGORY ( 'part', '', ( #5881 ) ) ;
#15720 = PLANE ( 'NONE',  #35616 ) ;
#15721 = ORIENTED_EDGE ( 'NONE', *, *, #25735, .T. ) ;
#15722 = CARTESIAN_POINT ( 'NONE',  ( 19.99999662536857770, 86.60254037844397601, -9.999999999999998224 ) ) ;
#15723 = EDGE_CURVE ( 'NONE', #11450, #12872, #7046, .T. ) ;
#15724 = CIRCLE ( 'NONE', #25891, 2.000000000000001776 ) ;
#15725 = LINE ( 'NONE', #2213, #20329 ) ;
#15726 = DIRECTION ( 'NONE',  ( 0.000000000000000000, -0.000000000000000000, -1.000000000000000000 ) ) ;
#15727 = ORIENTED_EDGE ( 'NONE', *, *, #11020, .F. ) ;
#15728 = DIRECTION ( 'NONE',  ( -1.000000000000000000, 0.000000000000000000, 0.000000000000000000 ) ) ;
#15729 = DIRECTION ( 'NONE',  ( 1.000000000000000000, 0.000000000000000000, 0.000000000000000000 ) ) ;
#15730 = VERTEX_POINT ( 'NONE', #1367 ) ;
#15731 = ORIENTED_EDGE ( 'NONE', *, *, #32785, .F. ) ;
#15732 = ORIENTED_EDGE ( 'NONE', *, *, #31089, .T. ) ;
#15733 = DIRECTION ( 'NONE',  ( 0.000000000000000000, 0.000000000000000000, 1.000000000000000000 ) ) ;
#15734 = EDGE_CURVE ( 'NONE', #27983, #23723, #27790, .T. ) ;
#15735 = LINE ( 'NONE', #24000, #1215 ) ;
#15736 = ORIENTED_EDGE ( 'NONE', *, *, #13954, .T. ) ;
#15737 = FACE_OUTER_BOUND ( 'NONE', #24418, .T. ) ;
#15738 = DIRECTION ( 'NONE',  ( -1.000000000000000000, 0.000000000000000000, 0.000000000000000000 ) ) ;
#15739 = ORIENTED_EDGE ( 'NONE', *, *, #12601, .T. ) ;
#15740 = FACE_OUTER_BOUND ( 'NONE', #35438, .T. ) ;
#15741 = CIRCLE ( 'NONE', #24123, 2.000000000000001776 ) ;
#15742 = CARTESIAN_POINT ( 'NONE',  ( -50.00000337463109190, 69.28203230275518365, -9.999999999999998224 ) ) ;
#15743 = CARTESIAN_POINT ( 'NONE',  ( 35.19434990244975126, -52.39915983220758022, 12.49999999999999822 ) ) ;
#15744 = CARTESIAN_POINT ( 'NONE',  ( -43.00000337463112743, -60.62177826491080168, -9.999999999999998224 ) ) ;
#15745 = DIRECTION ( 'NONE',  ( -1.000000000000000000, -0.000000000000000000, -0.000000000000000000 ) ) ;
#15746 = CARTESIAN_POINT ( 'NONE',  ( 47.99999662536846756, 51.96152422706637708, 12.50000000000000000 ) ) ;
#15747 = ORIENTED_EDGE ( 'NONE', *, *, #31672, .T. ) ;
#15748 = EDGE_CURVE ( 'NONE', #4556, #3254, #34881, .T. ) ;
#15749 = ORIENTED_EDGE ( 'NONE', *, *, #12902, .T. ) ;
#15750 = CARTESIAN_POINT ( 'NONE',  ( 11.99999662536861855, 69.28203230275516944, -5.000000000000000000 ) ) ;
#15751 = CIRCLE ( 'NONE', #36708, 2.000000000000001776 ) ;
#15752 = ADVANCED_FACE ( 'NONE', ( #9997 ), #35694, .F. ) ;
#15753 = CARTESIAN_POINT ( 'NONE',  ( -52.00000337463110611, -69.28203230275519786, 12.50000000000000000 ) ) ;
#15754 = CARTESIAN_POINT ( 'NONE',  ( -62.97617850287781494, -4.279621169095772615, -4.999999999999997335 ) ) ;
#15755 = CIRCLE ( 'NONE', #8556, 2.000000000000001776 ) ;
#15756 = DIRECTION ( 'NONE',  ( 1.000000000000000000, 0.000000000000000000, 0.000000000000000000 ) ) ;
#15757 = ORIENTED_EDGE ( 'NONE', *, *, #7768, .T. ) ;
#15758 = LINE ( 'NONE', #35640, #17162 ) ;
#15759 = CARTESIAN_POINT ( 'NONE',  ( -104.8061974404896262, 19.22934205795090534, 32.50000000000000000 ) ) ;
#15760 = ORIENTED_EDGE ( 'NONE', *, *, #19595, .T. ) ;
#15761 = EDGE_CURVE ( 'NONE', #8015, #14529, #7636, .T. ) ;
#15762 = CARTESIAN_POINT ( 'NONE',  ( 4.220257619726806020, 79.78402657284750887, -5.000000000000000000 ) ) ;
#15763 = AXIS2_PLACEMENT_3D ( 'NONE', #28023, #33479, #7408 ) ;
#15764 = EDGE_LOOP ( 'NONE', ( #16141, #399 ) ) ;
#15765 = CARTESIAN_POINT ( 'NONE',  ( 64.99999662536842493, 43.30127018922200222, -5.000000000000000000 ) ) ;
#15766 = AXIS2_PLACEMENT_3D ( 'NONE', #12312, #27326, #15708 ) ;
#15767 = CYLINDRICAL_SURFACE ( 'NONE', #12808, 3.500000000000000888 ) ;
#15768 = EDGE_CURVE ( 'NONE', #19731, #2354, #16630, .T. ) ;
#15769 = CARTESIAN_POINT ( 'NONE',  ( 2.008727693139922721, 4.613763217533267458, -0.5592653008974296514 ) ) ;
#15770 = ORIENTED_EDGE ( 'NONE', *, *, #16277, .T. ) ;
#15771 = ORIENTED_EDGE ( 'NONE', *, *, #5521, .T. ) ;
#15772 = AXIS2_PLACEMENT_3D ( 'NONE', #14408, #19849, #22295 ) ;
#15773 = ORIENTED_EDGE ( 'NONE', *, *, #36790, .F. ) ;
#15774 = FACE_OUTER_BOUND ( 'NONE', #23028, .T. ) ;
#15775 = CIRCLE ( 'NONE', #33746, 1.999999999999998224 ) ;
#15776 = FACE_BOUND ( 'NONE', #36621, .T. ) ;
#15777 = CARTESIAN_POINT ( 'NONE',  ( 106.7731239591688848, 98.28784258492994752, 27.50000000000000000 ) ) ;
#15778 = DIRECTION ( 'NONE',  ( 0.000000000000000000, 0.000000000000000000, 1.000000000000000000 ) ) ;
#15779 = DIRECTION ( 'NONE',  ( 0.000000000000000000, 0.000000000000000000, 1.000000000000000000 ) ) ;
#15780 = ORIENTED_EDGE ( 'NONE', *, *, #4783, .T. ) ;
#15781 = DIRECTION ( 'NONE',  ( 1.000000000000000000, 0.000000000000000000, 0.000000000000000000 ) ) ;
#15782 = PRODUCT_DEFINITION_SHAPE ( 'NONE', 'NONE',  #37136 ) ;
#15783 = EDGE_CURVE ( 'NONE', #10643, #23885, #12398, .T. ) ;
#15784 = DIRECTION ( 'NONE',  ( 0.000000000000000000, 0.000000000000000000, 1.000000000000000000 ) ) ;
#15785 = CARTESIAN_POINT ( 'NONE',  ( 20.39230124433451152, -84.64139349818795210, 12.50000000000000000 ) ) ;
#15786 = ORIENTED_EDGE ( 'NONE', *, *, #10048, .T. ) ;
#15787 = DIRECTION ( 'NONE',  ( 0.000000000000000000, 0.000000000000000000, -1.000000000000000000 ) ) ;
#15788 = DIRECTION ( 'NONE',  ( -1.000000000000000000, 0.000000000000000000, 0.000000000000000000 ) ) ;
#15789 = ORIENTED_EDGE ( 'NONE', *, *, #22199, .F. ) ;
#15790 = EDGE_CURVE ( 'NONE', #30459, #12033, #10633, .T. ) ;
#15791 = CIRCLE ( 'NONE', #9815, 2.000000000000001776 ) ;
#15792 = ORIENTED_EDGE ( 'NONE', *, *, #35156, .F. ) ;
#15793 = EDGE_CURVE ( 'NONE', #13489, #210, #7372, .T. ) ;
#15794 = PLANE ( 'NONE',  #24097 ) ;
#15795 = DIRECTION ( 'NONE',  ( 0.000000000000000000, 0.000000000000000000, -1.000000000000000000 ) ) ;
#15796 = CARTESIAN_POINT ( 'NONE',  ( -1.084202172485504434E-14, -5.773502691896260863, -2.080000000000000071 ) ) ;
#15797 = ORIENTED_EDGE ( 'NONE', *, *, #11855, .F. ) ;
#15798 = EDGE_LOOP ( 'NONE', ( #17019, #9960, #14075, #21557 ) ) ;
#15799 = VERTEX_POINT ( 'NONE', #4568 ) ;
#15800 = AXIS2_PLACEMENT_3D ( 'NONE', #25909, #24859, #23093 ) ;
#15801 = DIRECTION ( 'NONE',  ( 0.000000000000000000, 0.000000000000000000, 1.000000000000000000 ) ) ;
#15802 = VERTEX_POINT ( 'NONE', #16006 ) ;
#15803 = EDGE_LOOP ( 'NONE', ( #25610, #30119, #15410, #7904 ) ) ;
#15804 = FACE_BOUND ( 'NONE', #13394, .T. ) ;
#15805 = ORIENTED_EDGE ( 'NONE', *, *, #8831, .F. ) ;
#15806 = EDGE_LOOP ( 'NONE', ( #17754, #10288, #24876, #25953 ) ) ;
#15807 = DIRECTION ( 'NONE',  ( 0.000000000000000000, 0.000000000000000000, -1.000000000000000000 ) ) ;
#15808 = ADVANCED_FACE ( 'NONE', ( #16198 ), #27617, .F. ) ;
#15809 = LINE ( 'NONE', #10556, #8673 ) ;
#15810 = EDGE_LOOP ( 'NONE', ( #31873, #22988, #15378, #11044 ) ) ;
#15811 = ORIENTED_EDGE ( 'NONE', *, *, #10394, .F. ) ;
#15812 = DIRECTION ( 'NONE',  ( 0.000000000000000000, 0.000000000000000000, 1.000000000000000000 ) ) ;
#15813 = DIRECTION ( 'NONE',  ( 0.000000000000000000, 0.000000000000000000, 1.000000000000000000 ) ) ;
#15814 = LINE ( 'NONE', #15256, #2510 ) ;
#15815 = DIRECTION ( 'NONE',  ( 0.000000000000000000, 0.000000000000000000, 1.000000000000000000 ) ) ;
#15816 = AXIS2_PLACEMENT_3D ( 'NONE', #15283, #23933, #18486 ) ;
#15817 = VERTEX_POINT ( 'NONE', #7755 ) ;
#15818 = FACE_OUTER_BOUND ( 'NONE', #25171, .T. ) ;
#15819 = ORIENTED_EDGE ( 'NONE', *, *, #27927, .T. ) ;
#15820 = FACE_OUTER_BOUND ( 'NONE', #20331, .T. ) ;
#15821 = FACE_OUTER_BOUND ( 'NONE', #4202, .T. ) ;
#15822 = DIRECTION ( 'NONE',  ( 1.000000000000000000, 0.000000000000000000, 0.000000000000000000 ) ) ;
#15823 = CARTESIAN_POINT ( 'NONE',  ( -72.00000337463102085, -34.64101615137762025, -9.999999999999998224 ) ) ;
#15824 = CARTESIAN_POINT ( 'NONE',  ( 89.67878100130370456, -27.78182860042797131, -4.999999999999997335 ) ) ;
#15825 = VECTOR ( 'NONE', #10506, 1000.000000000000000 ) ;
#15826 = ADVANCED_FACE ( 'NONE', ( #36246 ), #5490, .F. ) ;
#15827 = CARTESIAN_POINT ( 'NONE',  ( 72.99999662536836809, 43.30127018922198801, 17.49999999999999645 ) ) ;
#15828 = AXIS2_PLACEMENT_3D ( 'NONE', #29248, #20809, #26614 ) ;
#15829 = DIRECTION ( 'NONE',  ( -1.000000000000000000, 0.000000000000000000, 0.000000000000000000 ) ) ;
#15830 = EDGE_LOOP ( 'NONE', ( #35737, #2476, #34772, #4933, #6409, #18245 ) ) ;
#15831 = EDGE_CURVE ( 'NONE', #9610, #19401, #30996, .T. ) ;
#15832 = CARTESIAN_POINT ( 'NONE',  ( -65.00000337463102085, 25.98076211353317433, -9.999999999999998224 ) ) ;
#15833 = DIRECTION ( 'NONE',  ( -1.000000000000000000, 0.000000000000000000, 0.000000000000000000 ) ) ;
#15834 = CARTESIAN_POINT ( 'NONE',  ( 86.99999662536831124, -25.98076211353319565, -9.999999999999998224 ) ) ;
#15835 = ORIENTED_EDGE ( 'NONE', *, *, #27545, .F. ) ;
#15836 = EDGE_CURVE ( 'NONE', #9631, #7182, #13031, .T. ) ;
#15837 = VERTEX_POINT ( 'NONE', #25548 ) ;
#15838 = ORIENTED_EDGE ( 'NONE', *, *, #21004, .F. ) ;
#15839 = DIRECTION ( 'NONE',  ( -0.000000000000000000, -0.000000000000000000, -1.000000000000000000 ) ) ;
#15840 = DIRECTION ( 'NONE',  ( 0.000000000000000000, 0.000000000000000000, 1.000000000000000000 ) ) ;
#15841 = DIRECTION ( 'NONE',  ( 1.000000000000000000, 0.000000000000000000, 0.000000000000000000 ) ) ;
#15842 = CIRCLE ( 'NONE', #36795, 2.000000000000001776 ) ;
#15843 = EDGE_CURVE ( 'NONE', #30108, #6520, #17820, .T. ) ;
#15844 = ORIENTED_EDGE ( 'NONE', *, *, #24914, .T. ) ;
#15845 = EDGE_CURVE ( 'NONE', #20137, #5193, #11239, .T. ) ;
#15846 = AXIS2_PLACEMENT_3D ( 'NONE', #9748, #21184, #32616 ) ;
#15847 = CARTESIAN_POINT ( 'NONE',  ( -80.00000337463096400, -34.64101615137762025, 12.50000000000000000 ) ) ;
#15848 = DIRECTION ( 'NONE',  ( 1.000000000000000000, 0.000000000000000000, 0.000000000000000000 ) ) ;
#15849 = ORIENTED_EDGE ( 'NONE', *, *, #22229, .F. ) ;
#15850 = CARTESIAN_POINT ( 'NONE',  ( -35.00000337463116296, -60.62177826491080168, -5.000000000000000000 ) ) ;
#15851 = ORIENTED_EDGE ( 'NONE', *, *, #35904, .T. ) ;
#15852 = CARTESIAN_POINT ( 'NONE',  ( 12.99999662536859901, 77.94228634059957983, -5.000000000000000000 ) ) ;
#15853 = EDGE_CURVE ( 'NONE', #13150, #20921, #22747, .T. ) ;
#15854 = CIRCLE ( 'NONE', #33213, 1.999999999999998224 ) ;
#15855 = AXIS2_PLACEMENT_3D ( 'NONE', #3351, #22869, #20578 ) ;
#15856 = EDGE_CURVE ( 'NONE', #17677, #6799, #18451, .T. ) ;
#15857 = CARTESIAN_POINT ( 'NONE',  ( 72.99999662536835388, -43.30127018922199511, -9.999999999999998224 ) ) ;
#15858 = DIRECTION ( 'NONE',  ( 0.000000000000000000, 0.000000000000000000, 1.000000000000000000 ) ) ;
#15859 = ADVANCED_FACE ( 'NONE', ( #28533 ), #34189, .F. ) ;
#15860 = VECTOR ( 'NONE', #4313, 1000.000000000000000 ) ;
#15861 = EDGE_CURVE ( 'NONE', #15313, #26527, #34624, .T. ) ;
#15862 = DIRECTION ( 'NONE',  ( 1.000000000000000000, -0.000000000000000000, 0.000000000000000000 ) ) ;
#15863 = EDGE_LOOP ( 'NONE', ( #24438, #18203, #34252, #26980 ) ) ;
#15864 = DIRECTION ( 'NONE',  ( 1.000000000000000000, 0.000000000000000000, 0.000000000000000000 ) ) ;
#15865 = DIRECTION ( 'NONE',  ( -0.000000000000000000, -0.8660254037844419273, -0.4999999999999941158 ) ) ;
#15866 = CARTESIAN_POINT ( 'NONE',  ( 49.99999662536848177, -51.96152422706640550, -9.999999999999998224 ) ) ;
#15867 = CIRCLE ( 'NONE', #275, 3.000000000000002665 ) ;
#15868 = DIRECTION ( 'NONE',  ( 1.000000000000000000, 0.000000000000000000, -0.000000000000000000 ) ) ;
#15869 = DIRECTION ( 'NONE',  ( 0.000000000000000000, 0.000000000000000000, 1.000000000000000000 ) ) ;
#15870 = VERTEX_POINT ( 'NONE', #22188 ) ;
#15871 = DIRECTION ( 'NONE',  ( 0.000000000000000000, 0.000000000000000000, 1.000000000000000000 ) ) ;
#15872 = AXIS2_PLACEMENT_3D ( 'NONE', #32698, #12807, #18471 ) ;
#15873 = DIRECTION ( 'NONE',  ( 1.000000000000000000, 0.000000000000000000, 0.000000000000000000 ) ) ;
#15874 = DIRECTION ( 'NONE',  ( 0.000000000000000000, 0.000000000000000000, 1.000000000000000000 ) ) ;
#15875 = AXIS2_PLACEMENT_3D ( 'NONE', #23029, #31992, #29006 ) ;
#15876 = ORIENTED_EDGE ( 'NONE', *, *, #17191, .T. ) ;
#15877 = EDGE_LOOP ( 'NONE', ( #3099, #17813, #10188, #28890 ) ) ;
#15878 = LINE ( 'NONE', #7437, #18958 ) ;
#15879 = CARTESIAN_POINT ( 'NONE',  ( -77.00000337463097821, -8.660254037844422825, -9.999999999999998224 ) ) ;
#15880 = AXIS2_PLACEMENT_3D ( 'NONE', #27490, #32738, #6861 ) ;
#15881 = AXIS2_PLACEMENT_3D ( 'NONE', #14696, #8900, #20334 ) ;
#15882 = DIRECTION ( 'NONE',  ( 1.000000000000000000, 0.000000000000000000, 0.000000000000000000 ) ) ;
#15883 = VERTEX_POINT ( 'NONE', #28340 ) ;
#15884 = DIRECTION ( 'NONE',  ( 0.000000000000000000, 0.000000000000000000, -1.000000000000000000 ) ) ;
#15885 = LINE ( 'NONE', #12684, #325 ) ;
#15886 = CARTESIAN_POINT ( 'NONE',  ( 71.99999662536841072, 51.96152422706640550, -9.999999999999998224 ) ) ;
#15887 = FACE_OUTER_BOUND ( 'NONE', #27535, .T. ) ;
#15888 = EDGE_LOOP ( 'NONE', ( #8305, #14245 ) ) ;
#15889 = ORIENTED_EDGE ( 'NONE', *, *, #26511, .T. ) ;
#15890 = CARTESIAN_POINT ( 'NONE',  ( 47.99999662536846756, 69.28203230275516944, 12.50000000000000000 ) ) ;
#15891 = AXIS2_PLACEMENT_3D ( 'NONE', #30069, #4225, #7944 ) ;
#15892 = CARTESIAN_POINT ( 'NONE',  ( 64.99999662536841072, -25.98076211353320275, -5.000000000000000000 ) ) ;
#15893 = ORIENTED_EDGE ( 'NONE', *, *, #22390, .T. ) ;
#15894 = AXIS2_PLACEMENT_3D ( 'NONE', #10381, #33258, #3070 ) ;
#15895 = DIRECTION ( 'NONE',  ( -1.000000000000000000, 0.000000000000000000, 0.000000000000000000 ) ) ;
#15896 = VERTEX_POINT ( 'NONE', #5659 ) ;
#15897 = DIRECTION ( 'NONE',  ( 0.000000000000000000, 0.000000000000000000, 1.000000000000000000 ) ) ;
#15898 = CIRCLE ( 'NONE', #327, 2.000000000000001776 ) ;
#15899 = AXIS2_PLACEMENT_3D ( 'NONE', #24336, #28069, #16443 ) ;
#15900 = CYLINDRICAL_SURFACE ( 'NONE', #1744, 2.000000000000000000 ) ;
#15901 = VERTEX_POINT ( 'NONE', #31337 ) ;
#15902 = ORIENTED_EDGE ( 'NONE', *, *, #2909, .T. ) ;
#15903 = EDGE_CURVE ( 'NONE', #6458, #28343, #11840, .T. ) ;
#15904 = CARTESIAN_POINT ( 'NONE',  ( 32.49191361593954497, 89.27079897466093428, -5.000000000000000000 ) ) ;
#15905 = VERTEX_POINT ( 'NONE', #5319 ) ;
#15906 = AXIS2_PLACEMENT_3D ( 'NONE', #10415, #28225, #2537 ) ;
#15907 = CARTESIAN_POINT ( 'NONE',  ( -43.19957991610399972, -47.04203867989563292, 12.49999999999999822 ) ) ;
#15908 = DIRECTION ( 'NONE',  ( -1.000000000000000000, 0.000000000000000000, 0.000000000000000000 ) ) ;
#15909 = LINE ( 'NONE', #20981, #28671 ) ;
#15910 = ORIENTED_EDGE ( 'NONE', *, *, #8345, .F. ) ;
#15911 = DIRECTION ( 'NONE',  ( -1.000000000000000000, 0.000000000000000000, 0.000000000000000000 ) ) ;
#15912 = DIRECTION ( 'NONE',  ( 0.000000000000000000, 0.000000000000000000, 1.000000000000000000 ) ) ;
#15913 = DIRECTION ( 'NONE',  ( 0.000000000000000000, 0.000000000000000000, -1.000000000000000000 ) ) ;
#15914 = ORIENTED_EDGE ( 'NONE', *, *, #22353, .T. ) ;
#15915 = VERTEX_POINT ( 'NONE', #27986 ) ;
#15916 = ORIENTED_EDGE ( 'NONE', *, *, #25265, .F. ) ;
#15918 = DIRECTION ( 'NONE',  ( 1.000000000000000000, 0.000000000000000000, 0.000000000000000000 ) ) ;
#15917 = VECTOR ( 'NONE', #19928, 1000.000000000000000 ) ;
#15919 = CARTESIAN_POINT ( 'NONE',  ( 35.19434990244975126, -52.39915983220758022, -49.22241343995298024 ) ) ;
#15920 = VERTEX_POINT ( 'NONE', #25197 ) ;
#15921 = AXIS2_PLACEMENT_3D ( 'NONE', #28502, #30950, #22716 ) ;
#15922 = CARTESIAN_POINT ( 'NONE',  ( 12.99999662536859901, 77.94228634059957983, 12.50000000000000000 ) ) ;
#15923 = AXIS2_PLACEMENT_3D ( 'NONE', #3535, #35021, #31648 ) ;
#15924 = DIRECTION ( 'NONE',  ( 0.000000000000000000, 0.000000000000000000, 1.000000000000000000 ) ) ;
#15925 = EDGE_CURVE ( 'NONE', #6013, #9603, #36623, .T. ) ;
#15926 = CIRCLE ( 'NONE', #35712, 6.726859516510129922 ) ;
#15927 = AXIS2_PLACEMENT_3D ( 'NONE', #18671, #26537, #32359 ) ;
#15928 = PLANE ( 'NONE',  #19453 ) ;
#15929 = EDGE_CURVE ( 'NONE', #28764, #8464, #33412, .T. ) ;
#15930 = AXIS2_PLACEMENT_3D ( 'NONE', #32705, #35722, #1226 ) ;
#15931 = CARTESIAN_POINT ( 'NONE',  ( -58.00000337463107059, -34.64101615137762025, -9.999999999999998224 ) ) ;
#15932 = CARTESIAN_POINT ( 'NONE',  ( -25.00000337463121980, -77.94228634059963667, 12.50000000000000000 ) ) ;
#15933 = DIRECTION ( 'NONE',  ( 0.000000000000000000, -1.000000000000000000, 0.000000000000000000 ) ) ;
#15934 = DIRECTION ( 'NONE',  ( 0.000000000000000000, 0.000000000000000000, 1.000000000000000000 ) ) ;
#15935 = CARTESIAN_POINT ( 'NONE',  ( -78.00000337463094979, 34.64101615137757051, 17.49999999999999645 ) ) ;
#15936 = EDGE_LOOP ( 'NONE', ( #36829, #7361, #4873, #12423 ) ) ;
#15937 = CIRCLE ( 'NONE', #32677, 33.00000000000002132 ) ;
#15938 = VERTEX_POINT ( 'NONE', #25359 ) ;
#15939 = EDGE_CURVE ( 'NONE', #1757, #12432, #36792, .T. ) ;
#15940 = CYLINDRICAL_SURFACE ( 'NONE', #26620, 2.000000000000001776 ) ;
#15941 = LINE ( 'NONE', #16143, #19358 ) ;
#15942 = CARTESIAN_POINT ( 'NONE',  ( 51.99999662536847467, 69.28203230275516944, -9.999999999999998224 ) ) ;
#15943 = CARTESIAN_POINT ( 'NONE',  ( 77.99999662536833966, -3.224517592124143893E-15, -9.999999999999998224 ) ) ;
#15944 = EDGE_LOOP ( 'NONE', ( #30308, #25258, #22638 ) ) ;
#15945 = CIRCLE ( 'NONE', #36899, 2.000000000000001776 ) ;
#15946 = DIRECTION ( 'NONE',  ( 0.000000000000000000, 0.000000000000000000, 1.000000000000000000 ) ) ;
#15947 = DIRECTION ( 'NONE',  ( 0.000000000000000000, 0.000000000000000000, 1.000000000000000000 ) ) ;
#15948 = AXIS2_PLACEMENT_3D ( 'NONE', #22514, #36595, #5629 ) ;
#15949 = DIRECTION ( 'NONE',  ( 1.000000000000000000, 0.000000000000000000, 0.000000000000000000 ) ) ;
#15950 = ORIENTED_EDGE ( 'NONE', *, *, #16749, .T. ) ;
#15951 = ADVANCED_FACE ( 'NONE', ( #17100 ), #25748, .T. ) ;
#15952 = CARTESIAN_POINT ( 'NONE',  ( 16.99999662536863454, -77.94228634059960825, -9.999999999999998224 ) ) ;
#15953 = VERTEX_POINT ( 'NONE', #4316 ) ;
#15954 = AXIS2_PLACEMENT_3D ( 'NONE', #31021, #28374, #16588 ) ;
#15955 = VECTOR ( 'NONE', #11101, 1000.000000000000000 ) ;
#15956 = VECTOR ( 'NONE', #10312, 1000.000000000000000 ) ;
#15957 = DIRECTION ( 'NONE',  ( 0.000000000000000000, 0.000000000000000000, -1.000000000000000000 ) ) ;
#15958 = VECTOR ( 'NONE', #4787, 1000.000000000000000 ) ;
#15959 = CARTESIAN_POINT ( 'NONE',  ( -68.00000337463099243, -2.428612866367529932E-14, 17.49999999999999645 ) ) ;
#15960 = AXIS2_PLACEMENT_3D ( 'NONE', #31973, #3320, #34658 ) ;
#15961 = CARTESIAN_POINT ( 'NONE',  ( -15.00000337463125710, -77.94228634059960825, -9.999999999999998224 ) ) ;
#15962 = VERTEX_POINT ( 'NONE', #27917 ) ;
#15963 = EDGE_LOOP ( 'NONE', ( #26804, #4998, #2635, #14465 ) ) ;
#15964 = VECTOR ( 'NONE', #1748, 1000.000000000000000 ) ;
#15965 = ORIENTED_EDGE ( 'NONE', *, *, #23552, .F. ) ;
#15966 = DIRECTION ( 'NONE',  ( -0.000000000000000000, -0.000000000000000000, 1.000000000000000000 ) ) ;
#15967 = EDGE_CURVE ( 'NONE', #16244, #27148, #27433, .T. ) ;
#15968 = CARTESIAN_POINT ( 'NONE',  ( 51.68138994340220904, 113.8157894736842053, 32.50000000000000000 ) ) ;
#15969 = CARTESIAN_POINT ( 'NONE',  ( 19.99999662536861678, -86.60254037844400443, 12.50000000000000000 ) ) ;
#15970 = FACE_OUTER_BOUND ( 'NONE', #6076, .T. ) ;
#15971 = FACE_OUTER_BOUND ( 'NONE', #29519, .T. ) ;
#15972 = EDGE_CURVE ( 'NONE', #10440, #4982, #25894, .T. ) ;
#15973 = VERTEX_POINT ( 'NONE', #22127 ) ;
#15974 = DIRECTION ( 'NONE',  ( 0.000000000000000000, 0.000000000000000000, 1.000000000000000000 ) ) ;
#15975 = AXIS2_PLACEMENT_3D ( 'NONE', #26101, #20298, #12187 ) ;
#15976 = CARTESIAN_POINT ( 'NONE',  ( -68.00000337463100664, -17.32050807568882078, -9.999999999999998224 ) ) ;
#15977 = AXIS2_PLACEMENT_3D ( 'NONE', #21918, #35450, #35822 ) ;
#15978 = PRODUCT_DEFINITION ( 'UNKNOWN', '', #23146, #16694 ) ;
#15979 = SURFACE_SIDE_STYLE ('',( #16175 ) ) ;
#15980 = ORIENTED_EDGE ( 'NONE', *, *, #12567, .T. ) ;
#15981 = CARTESIAN_POINT ( 'NONE',  ( 61.53067111003264955, -72.28378166041994746, -4.999999999999997335 ) ) ;
#15982 = EDGE_CURVE ( 'NONE', #29268, #25160, #24747, .T. ) ;
#15983 = AXIS2_PLACEMENT_3D ( 'NONE', #2962, #13650, #28084 ) ;
#15984 = DIRECTION ( 'NONE',  ( 0.000000000000000000, 0.000000000000000000, 1.000000000000000000 ) ) ;
#15985 = CIRCLE ( 'NONE', #36940, 3.866666666667000651 ) ;
#15986 = VERTEX_POINT ( 'NONE', #15746 ) ;
#15987 = ORIENTED_EDGE ( 'NONE', *, *, #25538, .T. ) ;
#15988 = VECTOR ( 'NONE', #1430, 1000.000000000000000 ) ;
#15989 = ADVANCED_FACE ( 'NONE', ( #16482 ), #27368, .F. ) ;
#15990 = DIRECTION ( 'NONE',  ( 1.000000000000000000, 0.000000000000000000, 0.000000000000000000 ) ) ;
#15991 = DIRECTION ( 'NONE',  ( 0.000000000000000000, 0.000000000000000000, 1.000000000000000000 ) ) ;
#15992 = DIRECTION ( 'NONE',  ( 0.000000000000000000, 0.000000000000000000, -1.000000000000000000 ) ) ;
#15993 = ORIENTED_EDGE ( 'NONE', *, *, #531, .T. ) ;
#15994 = ORIENTED_EDGE ( 'NONE', *, *, #20823, .F. ) ;
#15995 = ORIENTED_EDGE ( 'NONE', *, *, #3892, .T. ) ;
#15996 = VECTOR ( 'NONE', #34901, 1000.000000000000000 ) ;
#15997 = FACE_BOUND ( 'NONE', #31915, .T. ) ;
#15998 = ORIENTED_EDGE ( 'NONE', *, *, #35796, .F. ) ;
#15999 = VECTOR ( 'NONE', #9263, 1000.000000000000000 ) ;
#16000 = DIRECTION ( 'NONE',  ( 1.000000000000000000, 0.000000000000000000, 0.000000000000000000 ) ) ;
#16001 = ORIENTED_EDGE ( 'NONE', *, *, #4319, .F. ) ;
#16002 = CIRCLE ( 'NONE', #20772, 2.000000000000001776 ) ;
#16003 = AXIS2_PLACEMENT_3D ( 'NONE', #34154, #36590, #31140 ) ;
#16004 = VERTEX_POINT ( 'NONE', #24380 ) ;
#16005 = ADVANCED_FACE ( 'NONE', ( #33571 ), #36012, .T. ) ;
#16006 = CARTESIAN_POINT ( 'NONE',  ( -5.253368672218637236, 3.033033817057754877, -4.359491423763649287 ) ) ;
#16007 = CIRCLE ( 'NONE', #32779, 2.000000000000001776 ) ;
#16008 = DIRECTION ( 'NONE',  ( 0.000000000000000000, 0.000000000000000000, 1.000000000000000000 ) ) ;
#16009 = ORIENTED_EDGE ( 'NONE', *, *, #6043, .F. ) ;
#16010 = EDGE_LOOP ( 'NONE', ( #18634, #5159 ) ) ;
#16011 = CYLINDRICAL_SURFACE ( 'NONE', #9521, 2.000000000000001776 ) ;
#16012 = DIRECTION ( 'NONE',  ( -0.000000000000000000, -0.000000000000000000, 1.000000000000000000 ) ) ;
#16013 = EDGE_CURVE ( 'NONE', #12099, #36951, #24449, .T. ) ;
#16014 = CIRCLE ( 'NONE', #5813, 5.000000000000000000 ) ;
#16015 = CARTESIAN_POINT ( 'NONE',  ( 139.0000000000000284, -5.056524707326808249E-13, 32.55002500000000509 ) ) ;
#16016 = CARTESIAN_POINT ( 'NONE',  ( 42.99999662536850309, 77.94228634059959404, -9.999999999999998224 ) ) ;
#16017 = AXIS2_PLACEMENT_3D ( 'NONE', #14910, #29337, #9654 ) ;
#16018 = VERTEX_POINT ( 'NONE', #18748 ) ;
#16019 = DIRECTION ( 'NONE',  ( 0.000000000000000000, 0.000000000000000000, 1.000000000000000000 ) ) ;
#16021 = EDGE_LOOP ( 'NONE', ( #19251, #5585 ) ) ;
#16020 = EDGE_CURVE ( 'NONE', #21899, #1410, #4498, .T. ) ;
#16022 = DIRECTION ( 'NONE',  ( 0.000000000000000000, -0.8660254037844419273, -0.4999999999999945044 ) ) ;
#16023 = DIRECTION ( 'NONE',  ( 1.000000000000000000, 0.000000000000000000, 0.000000000000000000 ) ) ;
#16024 = CARTESIAN_POINT ( 'NONE',  ( 0.000000000000000000, 0.000000000000000000, 12.49999999999999822 ) ) ;
#16025 = CIRCLE ( 'NONE', #35774, 2.000000000000001776 ) ;
#16026 = DIRECTION ( 'NONE',  ( -0.000000000000000000, -0.000000000000000000, -1.000000000000000000 ) ) ;
#16027 = LINE ( 'NONE', #24652, #31995 ) ;
#16028 = LINE ( 'NONE', #1578, #37086 ) ;
#16029 = DIRECTION ( 'NONE',  ( 1.000000000000000000, 0.000000000000000000, 0.000000000000000000 ) ) ;
#16030 = VERTEX_POINT ( 'NONE', #25135 ) ;
#16031 = CARTESIAN_POINT ( 'NONE',  ( -40.99999999999999289, 103.4105893997321743, 32.50000000000000000 ) ) ;
#16032 = CIRCLE ( 'NONE', #15407, 2.000000000000001776 ) ;
#16033 = DIRECTION ( 'NONE',  ( 1.000000000000000000, 0.000000000000000000, 0.000000000000000000 ) ) ;
#16034 = DIRECTION ( 'NONE',  ( 0.000000000000000000, 0.000000000000000000, -1.000000000000000000 ) ) ;
#16035 = CIRCLE ( 'NONE', #17236, 2.000000000000001776 ) ;
#16036 = ORIENTED_EDGE ( 'NONE', *, *, #20828, .T. ) ;
#16037 = VERTEX_POINT ( 'NONE', #15935 ) ;
#16038 = VERTEX_POINT ( 'NONE', #7490 ) ;
#16039 = ADVANCED_FACE ( 'NONE', ( #13127 ), #13474, .F. ) ;
#16040 = VECTOR ( 'NONE', #19773, 1000.000000000000000 ) ;
#16041 = CARTESIAN_POINT ( 'NONE',  ( -3.374631303565411855E-06, -86.60254037844400443, -9.999999999999998224 ) ) ;
#16042 = CARTESIAN_POINT ( 'NONE',  ( -60.00000337463104216, 51.96152422706639129, -9.999999999999998224 ) ) ;
#16043 = EDGE_LOOP ( 'NONE', ( #13916, #20965 ) ) ;
#16044 = CIRCLE ( 'NONE', #22004, 2.000000000000001776 ) ;
#16045 = AXIS2_PLACEMENT_3D ( 'NONE', #36838, #34401, #5911 ) ;
#16046 = DIRECTION ( 'NONE',  ( 0.000000000000000000, 0.000000000000000000, 1.000000000000000000 ) ) ;
#16047 = DIRECTION ( 'NONE',  ( 0.000000000000000000, 0.000000000000000000, 1.000000000000000000 ) ) ;
#16048 = ORIENTED_EDGE ( 'NONE', *, *, #18685, .T. ) ;
#16049 = DIRECTION ( 'NONE',  ( 0.000000000000000000, 0.000000000000000000, 1.000000000000000000 ) ) ;
#16050 = VERTEX_POINT ( 'NONE', #36183 ) ;
#16051 = CARTESIAN_POINT ( 'NONE',  ( -20.00000337463122690, 86.60254037844397601, -9.999999999999998224 ) ) ;
#16052 = EDGE_CURVE ( 'NONE', #6561, #36949, #1694, .T. ) ;
#16053 = DIRECTION ( 'NONE',  ( 1.000000000000000000, 0.000000000000000000, 0.000000000000000000 ) ) ;
#16054 = CARTESIAN_POINT ( 'NONE',  ( -50.00000337463110611, -69.28203230275519786, -5.000000000000000000 ) ) ;
#16055 = CIRCLE ( 'NONE', #20244, 33.00000000000001421 ) ;
#16056 = CARTESIAN_POINT ( 'NONE',  ( -5.000000000000000888, -2.886751345948162406, -5.700000000000000178 ) ) ;
#16057 = EDGE_CURVE ( 'NONE', #29683, #9216, #21737, .T. ) ;
#16058 = ORIENTED_EDGE ( 'NONE', *, *, #15056, .F. ) ;
#16059 = CARTESIAN_POINT ( 'NONE',  ( 28.99999999999998934, 103.4105893997321743, -11.00000000000000355 ) ) ;
#16060 = AXIS2_PLACEMENT_3D ( 'NONE', #17185, #29163, #14729 ) ;
#16061 = AXIS2_PLACEMENT_3D ( 'NONE', #28902, #23305, #3228 ) ;
#16062 = ITEM_DEFINED_TRANSFORMATION ( 'NONE', 'NONE', #6385,  #21385 ) ;
#16063 = CIRCLE ( 'NONE', #1087, 2.000000000000001776 ) ;
#16064 = ADVANCED_FACE ( 'NONE', ( #16139 ), #1871, .T. ) ;
#16065 = CARTESIAN_POINT ( 'NONE',  ( 76.99999662536835388, -25.98076211353319565, -9.999999999999998224 ) ) ;
#16066 = CARTESIAN_POINT ( 'NONE',  ( 19.31922176934805435, 76.99660315353983719, 27.49999999999999645 ) ) ;
#16067 = VERTEX_POINT ( 'NONE', #7688 ) ;
#16068 = CARTESIAN_POINT ( 'NONE',  ( 6.249999999999998224, 3.980102097228899218E-16, 3.250000000000001332 ) ) ;
#16069 = DIRECTION ( 'NONE',  ( 1.000000000000000000, 0.000000000000000000, 0.000000000000000000 ) ) ;
#16070 = ORIENTED_EDGE ( 'NONE', *, *, #6812, .F. ) ;
#16071 = DIRECTION ( 'NONE',  ( 0.000000000000000000, 0.000000000000000000, 1.000000000000000000 ) ) ;
#16072 = EDGE_CURVE ( 'NONE', #24009, #22036, #19140, .T. ) ;
#16073 = DIRECTION ( 'NONE',  ( 0.000000000000000000, -0.8660254037844421493, -0.4999999999999942268 ) ) ;
#16074 = DIRECTION ( 'NONE',  ( 0.000000000000000000, 0.000000000000000000, -1.000000000000000000 ) ) ;
#16075 = EDGE_CURVE ( 'NONE', #13023, #17723, #16310, .T. ) ;
#16076 = CIRCLE ( 'NONE', #15448, 33.00000000000001421 ) ;
#16077 = VERTEX_POINT ( 'NONE', #24937 ) ;
#16078 = ORIENTED_EDGE ( 'NONE', *, *, #10471, .T. ) ;
#16079 = FACE_OUTER_BOUND ( 'NONE', #20822, .T. ) ;
#16080 = AXIS2_PLACEMENT_3D ( 'NONE', #17844, #21348, #1666 ) ;
#16081 = CYLINDRICAL_SURFACE ( 'NONE', #28498, 2.000000000000001776 ) ;
#16082 = ADVANCED_FACE ( 'NONE', ( #21373 ), #32816, .F. ) ;
#16083 = ADVANCED_FACE ( 'NONE', ( #22473 ), #5246, .F. ) ;
#16084 = DIRECTION ( 'NONE',  ( 1.000000000000000000, 0.000000000000000000, 0.000000000000000000 ) ) ;
#16085 = ORIENTED_EDGE ( 'NONE', *, *, #18809, .T. ) ;
#16086 = EDGE_CURVE ( 'NONE', #18552, #18736, #14226, .T. ) ;
#16087 = CIRCLE ( 'NONE', #26268, 33.00000000000001421 ) ;
#16088 = FACE_OUTER_BOUND ( 'NONE', #21283, .T. ) ;
#16089 = CARTESIAN_POINT ( 'NONE',  ( 3.035766082959412415E-15, 5.773502691896260863, -2.080000000000000071 ) ) ;
#16090 = EDGE_CURVE ( 'NONE', #2687, #11195, #3491, .T. ) ;
#16091 = AXIS2_PLACEMENT_3D ( 'NONE', #28309, #2632, #28694 ) ;
#16092 = CARTESIAN_POINT ( 'NONE',  ( 3.368272016354702636, 101.4480229402710592, -25.00000000000000000 ) ) ;
#16093 = DIRECTION ( 'NONE',  ( 1.000000000000000000, 0.000000000000000000, 0.000000000000000000 ) ) ;
#16094 = VERTEX_POINT ( 'NONE', #28111 ) ;
#16095 = AXIS2_PLACEMENT_3D ( 'NONE', #3659, #29146, #20700 ) ;
#16096 = VERTEX_POINT ( 'NONE', #8426 ) ;
#16097 = CARTESIAN_POINT ( 'NONE',  ( -53.00000337463106348, 60.62177826491078747, -9.999999999999998224 ) ) ;
#16098 = AXIS2_PLACEMENT_3D ( 'NONE', #24744, #15933, #19137 ) ;
#16099 = CARTESIAN_POINT ( 'NONE',  ( -20.00000337463124112, 69.28203230275516944, 12.50000000000000000 ) ) ;
#16100 = VERTEX_POINT ( 'NONE', #19677 ) ;
#16101 = CARTESIAN_POINT ( 'NONE',  ( -45.00000337463111322, 60.62177826491077326, -9.999999999999998224 ) ) ;
#16102 = ORIENTED_EDGE ( 'NONE', *, *, #15783, .T. ) ;
#16103 = CARTESIAN_POINT ( 'NONE',  ( -31.74999999999995737, 6.123233995736766282E-16, -5.000000000000000000 ) ) ;
#16104 = CIRCLE ( 'NONE', #12486, 3.500000000000000888 ) ;
#16105 = TOROIDAL_SURFACE ( 'NONE', #25078, 17.55872235085559652, 2.000000000000000000 ) ;
#16106 = EDGE_CURVE ( 'NONE', #16140, #8932, #22650, .T. ) ;
#16107 = CARTESIAN_POINT ( 'NONE',  ( 90.60231327712337190, 15.97563234535636134, 12.49999999999999822 ) ) ;
#16108 = VERTEX_POINT ( 'NONE', #14580 ) ;
#16109 = DIRECTION ( 'NONE',  ( 0.000000000000000000, 0.000000000000000000, 1.000000000000000000 ) ) ;
#16110 = ORIENTED_EDGE ( 'NONE', *, *, #21202, .F. ) ;
#16111 = CARTESIAN_POINT ( 'NONE',  ( -3.500000000000000888, -55.00000000000000000, -5.000000000000000888 ) ) ;
#16112 = AXIS2_PLACEMENT_3D ( 'NONE', #15549, #24160, #35611 ) ;
#16113 = DIRECTION ( 'NONE',  ( 0.000000000000000000, 0.000000000000000000, 1.000000000000000000 ) ) ;
#16114 = PLANE ( 'NONE',  #22718 ) ;
#16115 = EDGE_LOOP ( 'NONE', ( #15226, #29129, #14117, #8324 ) ) ;
#16116 = CYLINDRICAL_SURFACE ( 'NONE', #17853, 2.000000000000001776 ) ;
#16117 = EDGE_CURVE ( 'NONE', #9506, #4700, #2600, .T. ) ;
#16118 = AXIS2_PLACEMENT_3D ( 'NONE', #451, #23147, #35153 ) ;
#16119 = DIRECTION ( 'NONE',  ( -0.000000000000000000, 1.000000000000000000, 1.224646799147353207E-16 ) ) ;
#16120 = DIRECTION ( 'NONE',  ( 0.000000000000000000, 0.000000000000000000, 1.000000000000000000 ) ) ;
#16121 = ORIENTED_EDGE ( 'NONE', *, *, #7869, .T. ) ;
#16122 = EDGE_LOOP ( 'NONE', ( #2044, #16160, #27973, #29475 ) ) ;
#16123 = EDGE_LOOP ( 'NONE', ( #15717, #34697, #32342, #8153, #27013, #16395, #22197, #19704 ) ) ;
#16124 = CIRCLE ( 'NONE', #29860, 3.000000000000007994 ) ;
#16125 = DIRECTION ( 'NONE',  ( 1.000000000000000000, 0.000000000000000000, 0.000000000000000000 ) ) ;
#16126 = ORIENTED_EDGE ( 'NONE', *, *, #2684, .F. ) ;
#16127 = CARTESIAN_POINT ( 'NONE',  ( 3.500000000000000888, -55.00000000000000000, -5.000000000000000888 ) ) ;
#16128 = DIRECTION ( 'NONE',  ( 0.000000000000000000, 0.000000000000000000, 1.000000000000000000 ) ) ;
#16129 = AXIS2_PLACEMENT_3D ( 'NONE', #36384, #25142, #10693 ) ;
#16130 = EDGE_CURVE ( 'NONE', #545, #6597, #8242, .T. ) ;
#16131 = DIRECTION ( 'NONE',  ( -1.000000000000000000, 0.000000000000000000, 0.000000000000000000 ) ) ;
#16132 = CIRCLE ( 'NONE', #25128, 3.000000000000007105 ) ;
#16133 = EDGE_CURVE ( 'NONE', #34090, #19348, #32211, .T. ) ;
#16134 = EDGE_CURVE ( 'NONE', #29294, #22278, #25299, .T. ) ;
#16135 = DIRECTION ( 'NONE',  ( 0.000000000000000000, 0.000000000000000000, 1.000000000000000000 ) ) ;
#16136 = CIRCLE ( 'NONE', #36507, 27.00000000000001421 ) ;
#16137 = CARTESIAN_POINT ( 'NONE',  ( 71.99999662536839651, 17.32050807568879236, -9.999999999999998224 ) ) ;
#16138 = CARTESIAN_POINT ( 'NONE',  ( -5.999999999999998224, -145.0000000000000568, 32.50000000000000000 ) ) ;
#16139 = FACE_OUTER_BOUND ( 'NONE', #15359, .T. ) ;
#16140 = VERTEX_POINT ( 'NONE', #8781 ) ;
#16141 = ORIENTED_EDGE ( 'NONE', *, *, #24241, .T. ) ;
#16142 = VECTOR ( 'NONE', #35572, 1000.000000000000000 ) ;
#16143 = CARTESIAN_POINT ( 'NONE',  ( -62.00000337463104927, 51.96152422706639129, -9.999999999999998224 ) ) ;
#16144 = CYLINDRICAL_SURFACE ( 'NONE', #24657, 2.000000000000001776 ) ;
#16145 = CARTESIAN_POINT ( 'NONE',  ( -75.00000337463097821, -8.660254037844422825, 12.50000000000000000 ) ) ;
#16146 = EDGE_LOOP ( 'NONE', ( #28383, #28382, #5033, #20186 ) ) ;
#16147 = AXIS2_PLACEMENT_3D ( 'NONE', #11304, #10559, #25552 ) ;
#16148 = DIRECTION ( 'NONE',  ( 0.000000000000000000, 0.000000000000000000, 1.000000000000000000 ) ) ;
#16149 = CARTESIAN_POINT ( 'NONE',  ( -90.00000337463090716, -1.040834085586084257E-14, -9.999999999999998224 ) ) ;
#16150 = ORIENTED_EDGE ( 'NONE', *, *, #32252, .T. ) ;
#16151 = AXIS2_PLACEMENT_3D ( 'NONE', #20928, #12829, #15670 ) ;
#16152 = FACE_OUTER_BOUND ( 'NONE', #13408, .T. ) ;
#16153 = VERTEX_POINT ( 'NONE', #8592 ) ;
#16154 = ADVANCED_FACE ( 'NONE', ( #5433 ), #14028, .T. ) ;
#16155 = LINE ( 'NONE', #27583, #10914 ) ;
#16156 = DIRECTION ( 'NONE',  ( 0.000000000000000000, 0.000000000000000000, 1.000000000000000000 ) ) ;
#16157 = CIRCLE ( 'NONE', #26926, 2.000000000000001776 ) ;
#16158 = CARTESIAN_POINT ( 'NONE',  ( -58.88972745734203329, -33.99999999999965894, -4.999999999999997335 ) ) ;
#16159 = ORIENTED_EDGE ( 'NONE', *, *, #717, .F. ) ;
#16160 = ORIENTED_EDGE ( 'NONE', *, *, #11430, .T. ) ;
#16161 = AXIS2_PLACEMENT_3D ( 'NONE', #9164, #14611, #25876 ) ;
#16162 = DIRECTION ( 'NONE',  ( 0.5000000000000006661, -0.8660254037844383745, 0.000000000000000000 ) ) ;
#16163 = ORIENTED_EDGE ( 'NONE', *, *, #36253, .T. ) ;
#16164 = DIRECTION ( 'NONE',  ( -1.000000000000000000, -8.737866397512800437E-15, 0.000000000000000000 ) ) ;
#16165 = CIRCLE ( 'NONE', #12522, 2.000000000000001776 ) ;
#16166 = CARTESIAN_POINT ( 'NONE',  ( 62.99999662536842493, 43.30127018922200222, 17.49999999999999645 ) ) ;
#16167 = CIRCLE ( 'NONE', #17366, 2.000000000000001776 ) ;
#16168 = DIRECTION ( 'NONE',  ( -1.000000000000000000, 0.000000000000000000, 0.000000000000000000 ) ) ;
#16169 = CARTESIAN_POINT ( 'NONE',  ( -5.000000000000000888, -2.710505431213761085E-14, -3.620524600599874798 ) ) ;
#16170 = LINE ( 'NONE', #27200, #14732 ) ;
#16171 = ORIENTED_EDGE ( 'NONE', *, *, #10268, .T. ) ;
#16172 = FACE_OUTER_BOUND ( 'NONE', #23912, .T. ) ;
#16173 = FACE_OUTER_BOUND ( 'NONE', #35437, .T. ) ;
#16174 = EDGE_CURVE ( 'NONE', #30738, #7932, #16076, .T. ) ;
#16175 = SURFACE_STYLE_FILL_AREA ( #4913 ) ;
#16176 = ORIENTED_EDGE ( 'NONE', *, *, #16993, .F. ) ;
#16177 = CYLINDRICAL_SURFACE ( 'NONE', #2870, 2.000000000000001776 ) ;
#16178 = CARTESIAN_POINT ( 'NONE',  ( 9.999996625368625658, 86.60254037844397601, 17.49999999999999645 ) ) ;
#16179 = CIRCLE ( 'NONE', #33556, 2.000000000000001776 ) ;
#16180 = ORIENTED_EDGE ( 'NONE', *, *, #36489, .T. ) ;
#16181 = ORIENTED_EDGE ( 'NONE', *, *, #131, .F. ) ;
#16182 = CARTESIAN_POINT ( 'NONE',  ( -39.27785635698568711, -86.50000000000001421, 27.50000000000000000 ) ) ;
#16183 = COLOUR_RGB ( '', 0.31764706, 0.68627451, 0.89019608) ;
#16184 = CYLINDRICAL_SURFACE ( 'NONE', #18792, 3.000000000000002665 ) ;
#16185 = CARTESIAN_POINT ( 'NONE',  ( -2.981146944884250694, -4.052336700773510714, -0.5666985376598571156 ) ) ;
#16186 = ORIENTED_EDGE ( 'NONE', *, *, #12582, .F. ) ;
#16187 = ORIENTED_EDGE ( 'NONE', *, *, #8723, .F. ) ;
#16188 = CIRCLE ( 'NONE', #4814, 2.000000000000001776 ) ;
#16189 = ORIENTED_EDGE ( 'NONE', *, *, #24575, .T. ) ;
#16190 = DIRECTION ( 'NONE',  ( 1.000000000000000000, 0.000000000000000000, 0.000000000000000000 ) ) ;
#16191 = CIRCLE ( 'NONE', #3600, 2.000000000000001776 ) ;
#16192 = ORIENTED_EDGE ( 'NONE', *, *, #35928, .T. ) ;
#16193 = AXIS2_PLACEMENT_3D ( 'NONE', #13806, #25242, #22236 ) ;
#16194 = DIRECTION ( 'NONE',  ( -1.000000000000000000, 0.000000000000000000, 0.000000000000000000 ) ) ;
#16195 = ORIENTED_EDGE ( 'NONE', *, *, #9145, .T. ) ;
#16196 = ADVANCED_FACE ( 'NONE', ( #11228 ), #22675, .F. ) ;
#16197 = ORIENTED_EDGE ( 'NONE', *, *, #19403, .T. ) ;
#16198 = FACE_OUTER_BOUND ( 'NONE', #25266, .T. ) ;
#16199 = CARTESIAN_POINT ( 'NONE',  ( 19.99999662536861678, -86.60254037844400443, 17.49999999999999645 ) ) ;
#16200 = EDGE_LOOP ( 'NONE', ( #21938, #35307, #21006, #33056 ) ) ;
#16201 = EDGE_CURVE ( 'NONE', #4892, #32887, #30433, .T. ) ;
#16202 = ORIENTED_EDGE ( 'NONE', *, *, #31226, .T. ) ;
#16203 = DIRECTION ( 'NONE',  ( 0.000000000000000000, 0.000000000000000000, 1.000000000000000000 ) ) ;
#16204 = FACE_OUTER_BOUND ( 'NONE', #10792, .T. ) ;
#16205 = CARTESIAN_POINT ( 'NONE',  ( -35.00000337463116296, 77.94228634059957983, -5.000000000000000000 ) ) ;
#16206 = LINE ( 'NONE', #5126, #29838 ) ;
#16207 = EDGE_CURVE ( 'NONE', #31817, #17794, #7691, .T. ) ;
#16208 = ORIENTED_EDGE ( 'NONE', *, *, #34757, .T. ) ;
#16209 = DIRECTION ( 'NONE',  ( -0.000000000000000000, -0.000000000000000000, 1.000000000000000000 ) ) ;
#16210 = AXIS2_PLACEMENT_3D ( 'NONE', #5468, #25174, #36599 ) ;
#16211 = FACE_BOUND ( 'NONE', #9725, .T. ) ;
#16212 = DIRECTION ( 'NONE',  ( 0.000000000000000000, 0.000000000000000000, 1.000000000000000000 ) ) ;
#16213 = CIRCLE ( 'NONE', #32365, 33.00000000000001421 ) ;
#16214 = CARTESIAN_POINT ( 'NONE',  ( -94.55012560584690107, -9.234378588653415321, 32.50000000000000000 ) ) ;
#16215 = CYLINDRICAL_SURFACE ( 'NONE', #5748, 3.000000000000002665 ) ;
#16216 = DIRECTION ( 'NONE',  ( 0.000000000000000000, 0.000000000000000000, 1.000000000000000000 ) ) ;
#16217 = DIRECTION ( 'NONE',  ( 1.000000000000000000, 0.000000000000000000, 0.000000000000000000 ) ) ;
#16218 = EDGE_CURVE ( 'NONE', #1626, #11213, #7662, .T. ) ;
#16219 = DIRECTION ( 'NONE',  ( 1.000000000000000000, 0.000000000000000000, 0.000000000000000000 ) ) ;
#16220 = EDGE_LOOP ( 'NONE', ( #18193, #4364, #32530, #11362 ) ) ;
#16221 = CARTESIAN_POINT ( 'NONE',  ( 0.000000000000000000, 0.000000000000000000, -5.000000000000000000 ) ) ;
#16222 = CARTESIAN_POINT ( 'NONE',  ( 39.27785635698568711, 86.50000000000001421, 27.50000000000000000 ) ) ;
#16223 = DIRECTION ( 'NONE',  ( 0.000000000000000000, 0.000000000000000000, 1.000000000000000000 ) ) ;
#16224 = VERTEX_POINT ( 'NONE', #20026 ) ;
#16225 = ORIENTED_EDGE ( 'NONE', *, *, #10544, .T. ) ;
#16226 = ORIENTED_EDGE ( 'NONE', *, *, #26189, .F. ) ;
#16227 = CYLINDRICAL_SURFACE ( 'NONE', #35799, 2.000000000000001776 ) ;
#16228 = CARTESIAN_POINT ( 'NONE',  ( 37.99999662536853151, 69.28203230275518365, -5.000000000000000000 ) ) ;
#16229 = ORIENTED_EDGE ( 'NONE', *, *, #26824, .F. ) ;
#16230 = ADVANCED_FACE ( 'NONE', ( #17234 ), #3026, .F. ) ;
#16231 = DIRECTION ( 'NONE',  ( 0.4999999999999919509, -0.8660254037844433705, 0.000000000000000000 ) ) ;
#16232 = DIRECTION ( 'NONE',  ( 0.000000000000000000, 0.000000000000000000, 1.000000000000000000 ) ) ;
#16233 = VERTEX_POINT ( 'NONE', #20501 ) ;
#16234 = EDGE_CURVE ( 'NONE', #12760, #6161, #1071, .T. ) ;
#16235 = CIRCLE ( 'NONE', #4860, 25.00000000000000000 ) ;
#16236 = FACE_OUTER_BOUND ( 'NONE', #3112, .T. ) ;
#16237 = ORIENTED_EDGE ( 'NONE', *, *, #34193, .T. ) ;
#16238 = FACE_BOUND ( 'NONE', #9296, .T. ) ;
#16239 = EDGE_CURVE ( 'NONE', #2055, #14243, #31601, .T. ) ;
#16240 = CARTESIAN_POINT ( 'NONE',  ( 52.39915983220795681, 35.19434990244919703, 12.49999999999999822 ) ) ;
#16241 = CYLINDRICAL_SURFACE ( 'NONE', #14943, 2.000000000000001776 ) ;
#16242 = FACE_OUTER_BOUND ( 'NONE', #19456, .T. ) ;
#16243 = EDGE_CURVE ( 'NONE', #13116, #27668, #36415, .T. ) ;
#16244 = VERTEX_POINT ( 'NONE', #9814 ) ;
#16245 = DIRECTION ( 'NONE',  ( 1.000000000000000000, 0.000000000000000000, 0.000000000000000000 ) ) ;
#16246 = CONTEXT_DEPENDENT_SHAPE_REPRESENTATION ( #36495, #20853 ) ;
#16247 = CARTESIAN_POINT ( 'NONE',  ( 14.99999662536859901, 77.94228634059957983, -5.000000000000000000 ) ) ;
#16248 = DIRECTION ( 'NONE',  ( 1.000000000000000000, 0.000000000000000000, 0.000000000000000000 ) ) ;
#16249 = EDGE_CURVE ( 'NONE', #17343, #22235, #8885, .T. ) ;
#16250 = ORIENTED_EDGE ( 'NONE', *, *, #9771, .T. ) ;
#16251 = FACE_BOUND ( 'NONE', #12294, .T. ) ;
#16252 = FACE_OUTER_BOUND ( 'NONE', #9512, .T. ) ;
#16253 = ORIENTED_EDGE ( 'NONE', *, *, #22651, .T. ) ;
#16254 = CARTESIAN_POINT ( 'NONE',  ( 0.000000000000000000, 0.000000000000000000, 27.50000000000000000 ) ) ;
#16255 = AXIS2_PLACEMENT_3D ( 'NONE', #28117, #5603, #5801 ) ;
#16256 = FACE_OUTER_BOUND ( 'NONE', #3225, .T. ) ;
#16257 = DIRECTION ( 'NONE',  ( 1.000000000000000000, 0.000000000000000000, 0.000000000000000000 ) ) ;
#16258 = ORIENTED_EDGE ( 'NONE', *, *, #26135, .F. ) ;
#16259 = ORIENTED_EDGE ( 'NONE', *, *, #32824, .F. ) ;
#16260 = CARTESIAN_POINT ( 'NONE',  ( 0.000000000000000000, 0.000000000000000000, -5.000000000000000000 ) ) ;
#16261 = CARTESIAN_POINT ( 'NONE',  ( 76.99999662536835388, -25.98076211353319565, -9.999999999999998224 ) ) ;
#16262 = DIRECTION ( 'NONE',  ( 0.000000000000000000, 0.000000000000000000, -1.000000000000000000 ) ) ;
#16263 = EDGE_CURVE ( 'NONE', #7415, #5822, #1377, .T. ) ;
#16264 = ORIENTED_EDGE ( 'NONE', *, *, #155, .T. ) ;
#16265 = ORIENTED_EDGE ( 'NONE', *, *, #28962, .T. ) ;
#16266 = DIRECTION ( 'NONE',  ( -1.000000000000000000, 0.000000000000000000, -0.000000000000000000 ) ) ;
#16267 = CARTESIAN_POINT ( 'NONE',  ( -107.2724133595221190, -47.49999999999924682, 32.50002500000000083 ) ) ;
#16268 = DIRECTION ( 'NONE',  ( 0.000000000000000000, 0.000000000000000000, 1.000000000000000000 ) ) ;
#16269 = CARTESIAN_POINT ( 'NONE',  ( -103.8783455066836297, 60.08523189856654056, 32.50000000000000000 ) ) ;
#16270 = ORIENTED_EDGE ( 'NONE', *, *, #7965, .F. ) ;
#16271 = EDGE_CURVE ( 'NONE', #6061, #29798, #26510, .T. ) ;
#16272 = ORIENTED_EDGE ( 'NONE', *, *, #22483, .F. ) ;
#16273 = CARTESIAN_POINT ( 'NONE',  ( -39.27785635698568711, 86.50000000000001421, 32.50000000000000000 ) ) ;
#16274 = CIRCLE ( 'NONE', #15680, 65.00000000000000000 ) ;
#16275 = CARTESIAN_POINT ( 'NONE',  ( -82.27241335952113843, 47.50000000000096634, 27.50000000000000000 ) ) ;
#16276 = ORIENTED_EDGE ( 'NONE', *, *, #30554, .F. ) ;
#16277 = EDGE_CURVE ( 'NONE', #23050, #12167, #15457, .T. ) ;
#16278 = FACE_BOUND ( 'NONE', #28835, .T. ) ;
#16279 = EDGE_CURVE ( 'NONE', #33654, #36096, #9077, .T. ) ;
#16280 = ORIENTED_EDGE ( 'NONE', *, *, #381, .T. ) ;
#16281 = AXIS2_PLACEMENT_3D ( 'NONE', #15383, #23631, #24188 ) ;
#16282 = DIRECTION ( 'NONE',  ( 1.000000000000000000, 0.000000000000000000, 0.000000000000000000 ) ) ;
#16283 = DIRECTION ( 'NONE',  ( 0.000000000000000000, -1.000000000000000000, 1.034244904716769672E-15 ) ) ;
#16284 = CARTESIAN_POINT ( 'NONE',  ( -70.00000337463099243, 51.96152422706637708, -9.999999999999998224 ) ) ;
#16285 = ORIENTED_EDGE ( 'NONE', *, *, #24751, .T. ) ;
#16286 = SURFACE_SIDE_STYLE ('',( #4671 ) ) ;
#16287 = CARTESIAN_POINT ( 'NONE',  ( -56.74224907228983028, 68.66839587347264739, -4.999999999999997335 ) ) ;
#16288 = EDGE_CURVE ( 'NONE', #1500, #12218, #26846, .T. ) ;
#16289 = CYLINDRICAL_SURFACE ( 'NONE', #26298, 3.499999999999996003 ) ;
#16290 = DIRECTION ( 'NONE',  ( 0.000000000000000000, 0.000000000000000000, 1.000000000000000000 ) ) ;
#16291 = ORIENTED_EDGE ( 'NONE', *, *, #11731, .T. ) ;
#16292 = LINE ( 'NONE', #30342, #20268 ) ;
#16293 = CARTESIAN_POINT ( 'NONE',  ( -102.3448362992174623, 32.57931213457970188, 32.50000000000000000 ) ) ;
#16294 = CARTESIAN_POINT ( 'NONE',  ( -22.00000337463122690, 86.60254037844397601, -9.999999999999998224 ) ) ;
#16295 = ORIENTED_EDGE ( 'NONE', *, *, #24770, .F. ) ;
#16296 = ORIENTED_EDGE ( 'NONE', *, *, #31331, .T. ) ;
#16297 = ORIENTED_EDGE ( 'NONE', *, *, #22269, .F. ) ;
#16298 = AXIS2_PLACEMENT_3D ( 'NONE', #25762, #11482, #34367 ) ;
#16299 = CARTESIAN_POINT ( 'NONE',  ( -74.30619744049063513, -84.18124734178186941, 27.50000000000000000 ) ) ;
#16300 = VERTEX_POINT ( 'NONE', #17899 ) ;
#16301 = CARTESIAN_POINT ( 'NONE',  ( 0.000000000000000000, 0.000000000000000000, 5.000000000000000000 ) ) ;
#16302 = CYLINDRICAL_SURFACE ( 'NONE', #20199, 2.000000000000000000 ) ;
#16303 = DIRECTION ( 'NONE',  ( 0.000000000000000000, 0.000000000000000000, 1.000000000000000000 ) ) ;
#16304 = EDGE_CURVE ( 'NONE', #15633, #23588, #34068, .T. ) ;
#16305 = CARTESIAN_POINT ( 'NONE',  ( -27.78182860042817026, -56.67878100130359087, -49.86348611802629449 ) ) ;
#16306 = CARTESIAN_POINT ( 'NONE',  ( -72.00000337463100664, 34.64101615137758472, 17.49999999999999645 ) ) ;
#16307 = DIRECTION ( 'NONE',  ( -1.000000000000000000, -0.000000000000000000, -0.000000000000000000 ) ) ;
#16308 = EDGE_CURVE ( 'NONE', #10426, #18123, #2936, .T. ) ;
#16309 = CARTESIAN_POINT ( 'NONE',  ( 74.30619744049005249, 84.18124734178236679, 27.50000000000000000 ) ) ;
#16310 = LINE ( 'NONE', #27727, #10073 ) ;
#16311 = VERTEX_POINT ( 'NONE', #26695 ) ;
#16312 = EDGE_CURVE ( 'NONE', #36034, #4855, #10102, .T. ) ;
#16313 = VERTEX_POINT ( 'NONE', #21069 ) ;
#16314 = LINE ( 'NONE', #27730, #17618 ) ;
#16315 = DIRECTION ( 'NONE',  ( 0.000000000000000000, 0.000000000000000000, 1.000000000000000000 ) ) ;
#16316 = DIRECTION ( 'NONE',  ( 0.000000000000000000, 0.000000000000000000, -1.000000000000000000 ) ) ;
#16317 = DIRECTION ( 'NONE',  ( 1.000000000000000000, 0.000000000000000000, 0.000000000000000000 ) ) ;
#16318 = EDGE_CURVE ( 'NONE', #13911, #32985, #24078, .T. ) ;
#16319 = VERTEX_POINT ( 'NONE', #6814 ) ;
#16320 = EDGE_CURVE ( 'NONE', #29299, #30786, #21251, .T. ) ;
#16321 = CARTESIAN_POINT ( 'NONE',  ( 4.749999999999999112, 5.817072295949926440E-16, 0.000000000000000000 ) ) ;
#16322 = CARTESIAN_POINT ( 'NONE',  ( 31.09745072740910388, 83.47442710120324705, -49.86348611802629449 ) ) ;
#16323 = ORIENTED_EDGE ( 'NONE', *, *, #4972, .F. ) ;
#16324 = AXIS2_PLACEMENT_3D ( 'NONE', #19883, #11, #28310 ) ;
#16325 = DIRECTION ( 'NONE',  ( 0.000000000000000000, 0.000000000000000000, 1.000000000000000000 ) ) ;
#16326 = VERTEX_POINT ( 'NONE', #29681 ) ;
#16327 = EDGE_CURVE ( 'NONE', #18000, #15802, #17404, .T. ) ;
#16328 =( LENGTH_UNIT ( ) NAMED_UNIT ( * ) SI_UNIT ( .MILLI., .METRE. ) );
#16329 = DIRECTION ( 'NONE',  ( 0.000000000000000000, 0.000000000000000000, -1.000000000000000000 ) ) ;
#16330 = EDGE_CURVE ( 'NONE', #34395, #12253, #16206, .T. ) ;
#16331 = CARTESIAN_POINT ( 'NONE',  ( -57.00000337463111322, -43.30127018922202353, -9.999999999999998224 ) ) ;
#16332 = EDGE_CURVE ( 'NONE', #18228, #34315, #24481, .T. ) ;
#16333 = DIRECTION ( 'NONE',  ( 0.000000000000000000, 0.000000000000000000, 1.000000000000000000 ) ) ;
#16334 = EDGE_CURVE ( 'NONE', #35831, #34111, #1719, .T. ) ;
#16335 = B_SPLINE_CURVE_WITH_KNOTS ( 'NONE', 3,
 ( #18086, #32512, #12454, #35535, #29512, #27078, #1389, #24264, #23923, #35375 ),
 .UNSPECIFIED., .F., .F.,
 ( 4, 2, 2, 2, 4 ),
 ( 0.01815567983891738443, 0.01899359644517026671, 0.01983151305142315246, 0.02066942965767603474, 0.02150734626392891702 ),
 .UNSPECIFIED. ) ;
#16336 = ORIENTED_EDGE ( 'NONE', *, *, #13228, .T. ) ;
#16337 = ORIENTED_EDGE ( 'NONE', *, *, #36266, .T. ) ;
#16338 = VERTEX_POINT ( 'NONE', #10209 ) ;
#16339 = DIRECTION ( 'NONE',  ( 3.491481338843133750E-15, 1.000000000000000000, -0.000000000000000000 ) ) ;
#16340 = CARTESIAN_POINT ( 'NONE',  ( -86.45172111230354517, 31.46585318596159553, -4.999999999999997335 ) ) ;
#16341 = CARTESIAN_POINT ( 'NONE',  ( -17.00000337463126243, 77.94228634059957983, -9.999999999999998224 ) ) ;
#16342 = DIRECTION ( 'NONE',  ( 0.000000000000000000, 0.000000000000000000, 1.000000000000000000 ) ) ;
#16343 = DIRECTION ( 'NONE',  ( 0.000000000000000000, 0.000000000000000000, 1.000000000000000000 ) ) ;
#16344 = ORIENTED_EDGE ( 'NONE', *, *, #31674, .T. ) ;
#16345 = DIRECTION ( 'NONE',  ( 0.000000000000000000, 0.000000000000000000, 1.000000000000000000 ) ) ;
#16346 = DIRECTION ( 'NONE',  ( -1.000000000000000000, 0.000000000000000000, 0.000000000000000000 ) ) ;
#16347 = ORIENTED_EDGE ( 'NONE', *, *, #21556, .F. ) ;
#16348 = VECTOR ( 'NONE', #16223, 1000.000000000000000 ) ;
#16349 = CARTESIAN_POINT ( 'NONE',  ( -35.00000337463116296, 60.62177826491077326, 17.49999999999999645 ) ) ;
#16350 = CARTESIAN_POINT ( 'NONE',  ( 32.99999662536855283, 60.62177826491078747, -9.999999999999998224 ) ) ;
#16351 = VERTEX_POINT ( 'NONE', #13001 ) ;
#16352 = ORIENTED_EDGE ( 'NONE', *, *, #5654, .T. ) ;
#16353 = CARTESIAN_POINT ( 'NONE',  ( 77.99999662536832545, -34.64101615137759183, 12.50000000000000000 ) ) ;
#16354 = CARTESIAN_POINT ( 'NONE',  ( 11.99999662536861855, 69.28203230275516944, 12.50000000000000000 ) ) ;
#16355 = CARTESIAN_POINT ( 'NONE',  ( -77.93343913441745485, -72.12058696850748163, 27.50000000000000000 ) ) ;
#16356 = VERTEX_POINT ( 'NONE', #16565 ) ;
#16357 = EDGE_LOOP ( 'NONE', ( #36756, #10780, #517, #23155 ) ) ;
#16358 = CIRCLE ( 'NONE', #9760, 2.000000000000001776 ) ;
#16359 = DIRECTION ( 'NONE',  ( 1.000000000000000000, 0.000000000000000000, 0.000000000000000000 ) ) ;
#16360 = CIRCLE ( 'NONE', #30717, 2.541999999999999815 ) ;
#16361 = EDGE_LOOP ( 'NONE', ( #23977, #3951, #22744, #29015 ) ) ;
#16362 = LINE ( 'NONE', #16553, #17769 ) ;
#16363 = EDGE_LOOP ( 'NONE', ( #4757, #29647 ) ) ;
#16364 = ORIENTED_EDGE ( 'NONE', *, *, #1532, .F. ) ;
#16365 = DIRECTION ( 'NONE',  ( 0.000000000000000000, 0.000000000000000000, -1.000000000000000000 ) ) ;
#16366 = VECTOR ( 'NONE', #14866, 1000.000000000000000 ) ;
#16367 = FACE_OUTER_BOUND ( 'NONE', #36059, .T. ) ;
#16368 = EDGE_CURVE ( 'NONE', #3872, #21374, #1935, .T. ) ;
#16369 = ORIENTED_EDGE ( 'NONE', *, *, #13088, .T. ) ;
#16370 = VERTEX_POINT ( 'NONE', #18823 ) ;
#16371 = DIRECTION ( 'NONE',  ( -1.000000000000000000, 0.000000000000000000, 0.000000000000000000 ) ) ;
#16372 = LINE ( 'NONE', #33448, #23148 ) ;
#16373 = LINE ( 'NONE', #16015, #29443 ) ;
#16374 = CARTESIAN_POINT ( 'NONE',  ( 71.99999662536839651, 34.64101615137758472, -9.999999999999998224 ) ) ;
#16375 = VERTEX_POINT ( 'NONE', #36075 ) ;
#16376 = DIRECTION ( 'NONE',  ( 0.000000000000000000, 0.000000000000000000, 1.000000000000000000 ) ) ;
#16377 =( REPRESENTATION_RELATIONSHIP ('NONE','NONE', #15268, #34443 ) REPRESENTATION_RELATIONSHIP_WITH_TRANSFORMATION ( #4815 )SHAPE_REPRESENTATION_RELATIONSHIP( ) );
#16378 = FACE_BOUND ( 'NONE', #13414, .T. ) ;
#16379 = DIRECTION ( 'NONE',  ( 0.000000000000000000, 0.000000000000000000, 1.000000000000000000 ) ) ;
#16380 = AXIS2_PLACEMENT_3D ( 'NONE', #1787, #27646, #4795 ) ;
#16381 = CARTESIAN_POINT ( 'NONE',  ( -30.00000337463119848, -69.28203230275522628, -9.999999999999998224 ) ) ;
#16382 = DIRECTION ( 'NONE',  ( 1.000000000000000000, 0.000000000000000000, 0.000000000000000000 ) ) ;
#16383 = CARTESIAN_POINT ( 'NONE',  ( -33.00000337463116296, 77.94228634059957983, 12.50000000000000000 ) ) ;
#16384 = AXIS2_PLACEMENT_3D ( 'NONE', #21143, #13080, #23782 ) ;
#16385 = FACE_OUTER_BOUND ( 'NONE', #15081, .T. ) ;
#16386 = CARTESIAN_POINT ( 'NONE',  ( 79.99999662536832545, -34.64101615137759183, -9.999999999999998224 ) ) ;
#16387 = ORIENTED_EDGE ( 'NONE', *, *, #27737, .T. ) ;
#16388 = DIRECTION ( 'NONE',  ( -1.000000000000000000, 0.000000000000000000, -0.000000000000000000 ) ) ;
#16389 = DIRECTION ( 'NONE',  ( 1.000000000000000000, 0.000000000000000000, 0.000000000000000000 ) ) ;
#16390 = CARTESIAN_POINT ( 'NONE',  ( 40.99999999999999289, 103.4105893997321743, 32.50000000000000000 ) ) ;
#16391 = EDGE_CURVE ( 'NONE', #22972, #1373, #13555, .T. ) ;
#16392 = ADVANCED_FACE ( 'NONE', ( #13197 ), #24820, .F. ) ;
#16393 = AXIS2_PLACEMENT_3D ( 'NONE', #36990, #11299, #22916 ) ;
#16394 = ORIENTED_EDGE ( 'NONE', *, *, #27069, .F. ) ;
#16395 = ORIENTED_EDGE ( 'NONE', *, *, #10977, .F. ) ;
#16396 = ORIENTED_EDGE ( 'NONE', *, *, #2668, .F. ) ;
#16397 = VECTOR ( 'NONE', #28505, 1000.000000000000000 ) ;
#16398 = CARTESIAN_POINT ( 'NONE',  ( 21.99999662536857770, 86.60254037844397601, -9.999999999999998224 ) ) ;
#16399 = CARTESIAN_POINT ( 'NONE',  ( 0.000000000000000000, 0.000000000000000000, 4.700000000000000178 ) ) ;
#16400 = ORIENTED_EDGE ( 'NONE', *, *, #24311, .F. ) ;
#16401 = CIRCLE ( 'NONE', #7410, 2.000000000000001776 ) ;
#16402 = DIRECTION ( 'NONE',  ( -0.000000000000000000, -0.000000000000000000, 1.000000000000000000 ) ) ;
#16403 = EDGE_CURVE ( 'NONE', #17104, #10828, #19681, .T. ) ;
#16404 = LINE ( 'NONE', #33485, #26678 ) ;
#16405 = ORIENTED_EDGE ( 'NONE', *, *, #10155, .T. ) ;
#16406 = DIRECTION ( 'NONE',  ( 0.000000000000000000, 0.000000000000000000, 1.000000000000000000 ) ) ;
#16407 = ORIENTED_EDGE ( 'NONE', *, *, #25927, .F. ) ;
#16408 = DIRECTION ( 'NONE',  ( -1.000000000000000000, 0.000000000000000000, 0.000000000000000000 ) ) ;
#16409 = AXIS2_PLACEMENT_3D ( 'NONE', #17573, #8968, #14769 ) ;
#16410 = DIRECTION ( 'NONE',  ( -1.000000000000000000, 0.000000000000000000, 0.000000000000000000 ) ) ;
#16411 = CARTESIAN_POINT ( 'NONE',  ( 29.99999662536857770, -69.28203230275519786, -9.999999999999998224 ) ) ;
#16412 = EDGE_CURVE ( 'NONE', #31817, #15730, #30465, .T. ) ;
#16413 = ORIENTED_EDGE ( 'NONE', *, *, #15591, .T. ) ;
#16414 = DIRECTION ( 'NONE',  ( -0.7071067811865388020, 0.7071067811865563435, 0.000000000000000000 ) ) ;
#16415 = CIRCLE ( 'NONE', #36199, 27.00000000000001421 ) ;
#16416 = CARTESIAN_POINT ( 'NONE',  ( 6.497954182785949224E-14, 5.999999999999947597, 32.50000000000000000 ) ) ;
#16417 = CARTESIAN_POINT ( 'NONE',  ( -12.00000337463128908, 69.28203230275516944, -9.999999999999998224 ) ) ;
#16418 = EDGE_LOOP ( 'NONE', ( #12901, #8356, #3012, #31125, #30551 ) ) ;
#16419 = AXIS2_PLACEMENT_3D ( 'NONE', #24046, #977, #15613 ) ;
#16420 = FACE_BOUND ( 'NONE', #24957, .T. ) ;
#16421 = CYLINDRICAL_SURFACE ( 'NONE', #36513, 3.500000000000003109 ) ;
#16422 = ORIENTED_EDGE ( 'NONE', *, *, #20999, .T. ) ;
#16423 = CARTESIAN_POINT ( 'NONE',  ( 64.99999662536839651, -60.62177826491080168, -9.999999999999998224 ) ) ;
#16424 = DIRECTION ( 'NONE',  ( 0.000000000000000000, 0.000000000000000000, -1.000000000000000000 ) ) ;
#16425 = DIRECTION ( 'NONE',  ( 0.000000000000000000, 0.000000000000000000, 1.000000000000000000 ) ) ;
#16426 = ORIENTED_EDGE ( 'NONE', *, *, #11688, .T. ) ;
#16427 = EDGE_CURVE ( 'NONE', #19893, #15625, #27466, .T. ) ;
#16428 = ORIENTED_EDGE ( 'NONE', *, *, #16466, .T. ) ;
#16429 = PLANE ( 'NONE',  #8196 ) ;
#16430 = CARTESIAN_POINT ( 'NONE',  ( 64.99999662536839651, 60.62177826491078747, -9.999999999999998224 ) ) ;
#16431 = CARTESIAN_POINT ( 'NONE',  ( 66.99999662536839651, -43.30127018922199511, -9.999999999999998224 ) ) ;
#16432 = ORIENTED_EDGE ( 'NONE', *, *, #12948, .T. ) ;
#16433 = ORIENTED_EDGE ( 'NONE', *, *, #15047, .F. ) ;
#16434 = CARTESIAN_POINT ( 'NONE',  ( -20.00000337463123756, -86.60254037844400443, 12.50000000000000000 ) ) ;
#16435 = LINE ( 'NONE', #1829, #26806 ) ;
#16436 = ADVANCED_FACE ( 'NONE', ( #30241 ), #19208, .F. ) ;
#16437 = DIRECTION ( 'NONE',  ( 1.000000000000000000, 0.000000000000000000, 0.000000000000000000 ) ) ;
#16438 = CARTESIAN_POINT ( 'NONE',  ( 0.000000000000000000, 0.000000000000000000, -5.624496230895140947 ) ) ;
#16439 = EDGE_LOOP ( 'NONE', ( #22401, #26965, #10099, #22300 ) ) ;
#16440 = AXIS2_PLACEMENT_3D ( 'NONE', #546, #11782, #23426 ) ;
#16441 = CIRCLE ( 'NONE', #26014, 45.00000000000000000 ) ;
#16442 = ORIENTED_EDGE ( 'NONE', *, *, #595, .F. ) ;
#16443 = DIRECTION ( 'NONE',  ( 1.000000000000000000, 0.000000000000000000, 0.000000000000000000 ) ) ;
#16444 = EDGE_CURVE ( 'NONE', #34315, #34831, #11298, .T. ) ;
#16445 = VECTOR ( 'NONE', #23065, 1000.000000000000000 ) ;
#16446 = DIRECTION ( 'NONE',  ( -0.000000000000000000, -0.000000000000000000, -1.000000000000000000 ) ) ;
#16447 = ORIENTED_EDGE ( 'NONE', *, *, #5914, .T. ) ;
#16448 = CARTESIAN_POINT ( 'NONE',  ( -1.721886139904448276, -5.052888355616937055, -4.057689166958561522 ) ) ;
#16449 = ORIENTED_EDGE ( 'NONE', *, *, #10090, .T. ) ;
#16450 = CARTESIAN_POINT ( 'NONE',  ( -40.00000337463113453, -69.28203230275519786, -9.999999999999998224 ) ) ;
#16451 = DIRECTION ( 'NONE',  ( 1.000000000000000000, 0.000000000000000000, 0.000000000000000000 ) ) ;
#16452 = AXIS2_PLACEMENT_3D ( 'NONE', #23616, #29244, #32239 ) ;
#16453 = VECTOR ( 'NONE', #5, 1000.000000000000000 ) ;
#16454 = CARTESIAN_POINT ( 'NONE',  ( 4.319324222803677671, 3.279739689143281289, -3.838711833383739780 ) ) ;
#16455 = ORIENTED_EDGE ( 'NONE', *, *, #24523, .F. ) ;
#16456 = VECTOR ( 'NONE', #35074, 1000.000000000000000 ) ;
#16457 = DIRECTION ( 'NONE',  ( -1.000000000000000000, 0.000000000000000000, -0.000000000000000000 ) ) ;
#16458 = EDGE_CURVE ( 'NONE', #29420, #6561, #509, .T. ) ;
#16459 = DIRECTION ( 'NONE',  ( 0.000000000000000000, 0.000000000000000000, -1.000000000000000000 ) ) ;
#16460 = DIRECTION ( 'NONE',  ( 1.000000000000000000, 0.000000000000000000, 0.000000000000000000 ) ) ;
#16461 = ORIENTED_EDGE ( 'NONE', *, *, #16013, .T. ) ;
#16462 = CARTESIAN_POINT ( 'NONE',  ( 108.3061974404897825, -19.22934205795014151, 32.50000000000000000 ) ) ;
#16463 = DIRECTION ( 'NONE',  ( -0.000000000000000000, -0.000000000000000000, -1.000000000000000000 ) ) ;
#16464 = LINE ( 'NONE', #19122, #30298 ) ;
#16465 = AXIS2_PLACEMENT_3D ( 'NONE', #17392, #28809, #3133 ) ;
#16466 = EDGE_CURVE ( 'NONE', #15620, #24169, #35899, .T. ) ;
#16467 = CIRCLE ( 'NONE', #18881, 2.000000000000001776 ) ;
#16468 = ORIENTED_EDGE ( 'NONE', *, *, #2909, .F. ) ;
#16469 = ORIENTED_EDGE ( 'NONE', *, *, #32388, .T. ) ;
#16470 = ADVANCED_FACE ( 'NONE', ( #27443 ), #21451, .F. ) ;
#16471 = DIRECTION ( 'NONE',  ( -1.000000000000000000, 0.000000000000000000, 0.000000000000000000 ) ) ;
#16472 = EDGE_LOOP ( 'NONE', ( #35045, #27522, #22436, #35487 ) ) ;
#16473 = CARTESIAN_POINT ( 'NONE',  ( 6.123233995736731770E-16, -145.0000000000000568, 32.55002500000000509 ) ) ;
#16474 = CARTESIAN_POINT ( 'NONE',  ( -39.27785635698568711, 86.50000000000001421, 27.50000000000000000 ) ) ;
#16475 = DIRECTION ( 'NONE',  ( 0.8660254037844344888, -0.5000000000000071054, 0.000000000000000000 ) ) ;
#16476 = AXIS2_PLACEMENT_3D ( 'NONE', #25408, #19411, #13601 ) ;
#16477 = DIRECTION ( 'NONE',  ( 1.000000000000000000, 0.000000000000000000, 0.000000000000000000 ) ) ;
#16478 = CARTESIAN_POINT ( 'NONE',  ( 80.47895202573684514, -72.44487385379852640, 32.50000000000000000 ) ) ;
#16479 = DIRECTION ( 'NONE',  ( 0.000000000000000000, 0.000000000000000000, 1.000000000000000000 ) ) ;
#16480 = AXIS2_PLACEMENT_3D ( 'NONE', #17363, #11165, #34067 ) ;
#16481 = CARTESIAN_POINT ( 'NONE',  ( 3.000000000000000000, 3.113052163432572109E-16, -2.541999999999999815 ) ) ;
#16482 = FACE_OUTER_BOUND ( 'NONE', #21310, .T. ) ;
#16483 = AXIS2_PLACEMENT_3D ( 'NONE', #20185, #290, #8562 ) ;
#16484 = ORIENTED_EDGE ( 'NONE', *, *, #19233, .F. ) ;
#16485 = AXIS2_PLACEMENT_3D ( 'NONE', #708, #9532, #18142 ) ;
#16486 = ORIENTED_EDGE ( 'NONE', *, *, #25811, .F. ) ;
#16487 = PRESENTATION_STYLE_ASSIGNMENT (( #33378 ) ) ;
#16488 = EDGE_CURVE ( 'NONE', #29904, #2589, #7567, .T. ) ;
#16489 = CARTESIAN_POINT ( 'NONE',  ( -10.00000337463125000, -86.60254037844400443, -5.000000000000000000 ) ) ;
#16490 = CARTESIAN_POINT ( 'NONE',  ( 72.99999662536835388, -25.98076211353319565, 17.49999999999999645 ) ) ;
#16491 = DIRECTION ( 'NONE',  ( -1.000000000000000000, 0.000000000000000000, 0.000000000000000000 ) ) ;
#16492 = EDGE_LOOP ( 'NONE', ( #31789, #34932, #25704, #29024 ) ) ;
#16493 = AXIS2_PLACEMENT_3D ( 'NONE', #3497, #32154, #32356 ) ;
#16494 = VECTOR ( 'NONE', #27663, 1000.000000000000000 ) ;
#16495 = AXIS2_PLACEMENT_3D ( 'NONE', #18882, #10820, #30311 ) ;
#16496 = DIRECTION ( 'NONE',  ( 0.000000000000000000, 0.000000000000000000, 1.000000000000000000 ) ) ;
#16497 = ORIENTED_EDGE ( 'NONE', *, *, #28086, .T. ) ;
#16498 = ORIENTED_EDGE ( 'NONE', *, *, #4175, .T. ) ;
#16499 = DIRECTION ( 'NONE',  ( -0.000000000000000000, -0.000000000000000000, 1.000000000000000000 ) ) ;
#16500 = ORIENTED_EDGE ( 'NONE', *, *, #30719, .F. ) ;
#16501 = FACE_OUTER_BOUND ( 'NONE', #9097, .T. ) ;
#16502 = DIRECTION ( 'NONE',  ( -1.000000000000000000, 0.000000000000000000, -0.000000000000000000 ) ) ;
#16503 = EDGE_CURVE ( 'NONE', #21657, #20554, #17274, .T. ) ;
#16504 = AXIS2_PLACEMENT_3D ( 'NONE', #3069, #23107, #58 ) ;
#16505 = DIRECTION ( 'NONE',  ( -0.000000000000000000, -0.000000000000000000, -1.000000000000000000 ) ) ;
#16506 = ORIENTED_EDGE ( 'NONE', *, *, #19097, .T. ) ;
#16507 = EDGE_CURVE ( 'NONE', #17078, #18795, #19109, .T. ) ;
#16508 = CIRCLE ( 'NONE', #2131, 2.000000000000001776 ) ;
#16509 = VERTEX_POINT ( 'NONE', #11477 ) ;
#16510 = CIRCLE ( 'NONE', #3334, 2.000000000000001776 ) ;
#16511 = CIRCLE ( 'NONE', #3335, 3.500000000000003109 ) ;
#16512 = EDGE_LOOP ( 'NONE', ( #28506, #19702 ) ) ;
#16513 = AXIS2_PLACEMENT_3D ( 'NONE', #30275, #36656, #13589 ) ;
#16514 = ADVANCED_FACE ( 'NONE', ( #19564 ), #6051, .F. ) ;
#16515 = AXIS2_PLACEMENT_3D ( 'NONE', #29347, #32346, #476 ) ;
#16516 = ORIENTED_EDGE ( 'NONE', *, *, #1865, .T. ) ;
#16517 = CARTESIAN_POINT ( 'NONE',  ( -20.00000337463123756, -86.60254037844400443, -9.999999999999998224 ) ) ;
#16518 = CARTESIAN_POINT ( 'NONE',  ( 0.000000000000000000, 89.94802294027088863, 30.77834620192012594 ) ) ;
#16519 = EDGE_CURVE ( 'NONE', #35595, #34395, #34650, .T. ) ;
#16520 = CARTESIAN_POINT ( 'NONE',  ( 0.000000000000000000, 0.000000000000000000, 17.49999999999999645 ) ) ;
#16521 = FACE_OUTER_BOUND ( 'NONE', #25321, .T. ) ;
#16522 = CARTESIAN_POINT ( 'NONE',  ( 4.999999999999999112, -1.088215558004119066, -3.720998139100774260 ) ) ;
#16523 = EDGE_CURVE ( 'NONE', #16356, #20554, #32846, .T. ) ;
#16524 = ORIENTED_EDGE ( 'NONE', *, *, #11577, .F. ) ;
#16525 = DIRECTION ( 'NONE',  ( 0.000000000000000000, 0.000000000000000000, -1.000000000000000000 ) ) ;
#16526 = CIRCLE ( 'NONE', #14133, 2.000000000000001776 ) ;
#16527 = DIRECTION ( 'NONE',  ( -0.000000000000000000, -0.000000000000000000, -1.000000000000000000 ) ) ;
#16528 = ORIENTED_EDGE ( 'NONE', *, *, #4995, .T. ) ;
#16529 = DIRECTION ( 'NONE',  ( 0.000000000000000000, 0.000000000000000000, 1.000000000000000000 ) ) ;
#16530 = DIRECTION ( 'NONE',  ( 0.000000000000000000, 0.000000000000000000, -1.000000000000000000 ) ) ;
#16531 = EDGE_CURVE ( 'NONE', #2942, #15689, #34198, .T. ) ;
#16532 = VERTEX_POINT ( 'NONE', #17112 ) ;
#16533 = CIRCLE ( 'NONE', #24918, 6.000000000000005329 ) ;
#16534 = ADVANCED_FACE ( 'NONE', ( #19755 ), #16105, .T. ) ;
#16535 = ORIENTED_EDGE ( 'NONE', *, *, #10453, .T. ) ;
#16536 = DIRECTION ( 'NONE',  ( -1.000000000000000000, -0.000000000000000000, -0.000000000000000000 ) ) ;
#16537 = EDGE_CURVE ( 'NONE', #13513, #3470, #18482, .T. ) ;
#16538 = CIRCLE ( 'NONE', #13556, 150.0000000000000284 ) ;
#16539 = EDGE_CURVE ( 'NONE', #17144, #37066, #3062, .T. ) ;
#16540 = DIRECTION ( 'NONE',  ( 0.000000000000000000, 0.000000000000000000, 1.000000000000000000 ) ) ;
#16541 = CARTESIAN_POINT ( 'NONE',  ( 0.8441225671311781698, -5.568793373801108615, -4.176900509771829029 ) ) ;
#16542 = B_SPLINE_CURVE_WITH_KNOTS ( 'NONE', 3,
 ( #34048, #19794, #14143, #23897, #15072, #9456, #8897, #28935, #20684, #31756, #11881, #6083, #17692, #32114, #29127, #26139, #29488, #6256, #3462, #14893 ),
 .UNSPECIFIED., .F., .F.,
 ( 4, 2, 2, 2, 2, 2, 2, 2, 2, 4 ),
 ( 2.781148944256651962E-07, 0.0008372784139787452749, 0.001674278713063064939, 0.002511279012147384603, 0.003348279311231704483, 0.003766779460773864857, 0.004185279610316025231, 0.005022279909400345112, 0.005859280208484664992, 0.006696280507568985740 ),
 .UNSPECIFIED. ) ;
#16543 = EDGE_CURVE ( 'NONE', #2363, #17289, #31053, .T. ) ;
#16544 = CARTESIAN_POINT ( 'NONE',  ( -4.828573329308746942, -2.985724580418009921, -1.878862934774787830 ) ) ;
#16545 = VERTEX_POINT ( 'NONE', #37000 ) ;
#16546 = ORIENTED_EDGE ( 'NONE', *, *, #27912, .T. ) ;
#16547 = VECTOR ( 'NONE', #35291, 1000.000000000000000 ) ;
#16548 = AXIS2_PLACEMENT_3D ( 'NONE', #12295, #32188, #35413 ) ;
#16549 = VECTOR ( 'NONE', #18841, 1000.000000000000000 ) ;
#16550 = FACE_BOUND ( 'NONE', #12545, .T. ) ;
#16551 = CIRCLE ( 'NONE', #30905, 1.999999999999998224 ) ;
#16552 = ORIENTED_EDGE ( 'NONE', *, *, #9288, .T. ) ;
#16553 = CARTESIAN_POINT ( 'NONE',  ( 4.242640687119251020, -4.242640687119268783, 32.50000000000000000 ) ) ;
#16554 = ORIENTED_EDGE ( 'NONE', *, *, #34984, .F. ) ;
#16555 = VERTEX_POINT ( 'NONE', #31718 ) ;
#16556 = AXIS2_PLACEMENT_3D ( 'NONE', #12426, #29483, #3805 ) ;
#16557 = DIRECTION ( 'NONE',  ( 0.000000000000000000, 0.000000000000000000, 1.000000000000000000 ) ) ;
#16558 = DIRECTION ( 'NONE',  ( 1.000000000000000000, 0.000000000000000000, 0.000000000000000000 ) ) ;
#16559 = ORIENTED_EDGE ( 'NONE', *, *, #6430, .F. ) ;
#16560 = ORIENTED_EDGE ( 'NONE', *, *, #24863, .T. ) ;
#16561 = LINE ( 'NONE', #19368, #34105 ) ;
#16562 = DIRECTION ( 'NONE',  ( -1.000000000000000000, 0.000000000000000000, 0.000000000000000000 ) ) ;
#16563 = AXIS2_PLACEMENT_3D ( 'NONE', #217, #28897, #6410 ) ;
#16564 = DIRECTION ( 'NONE',  ( 0.000000000000000000, 0.000000000000000000, 1.000000000000000000 ) ) ;
#16565 = CARTESIAN_POINT ( 'NONE',  ( -68.00000337463099243, 51.96152422706637708, 12.50000000000000000 ) ) ;
#16566 = ORIENTED_EDGE ( 'NONE', *, *, #3746, .T. ) ;
#16567 = DIRECTION ( 'NONE',  ( 1.000000000000000000, 0.000000000000000000, 0.000000000000000000 ) ) ;
#16568 = FACE_BOUND ( 'NONE', #30084, .T. ) ;
#16569 = AXIS2_PLACEMENT_3D ( 'NONE', #14559, #35204, #3689 ) ;
#16570 = DIRECTION ( 'NONE',  ( 0.000000000000000000, 0.000000000000000000, 1.000000000000000000 ) ) ;
#16571 = CARTESIAN_POINT ( 'NONE',  ( 77.99999662536833966, 34.64101615137759183, -9.999999999999998224 ) ) ;
#16572 = AXIS2_PLACEMENT_3D ( 'NONE', #32889, #15813, #6811 ) ;
#16573 = DIRECTION ( 'NONE',  ( 0.000000000000000000, 0.000000000000000000, -1.000000000000000000 ) ) ;
#16574 = CARTESIAN_POINT ( 'NONE',  ( -22.00000337463124112, -86.60254037844400443, 17.49999999999999645 ) ) ;
#16575 = VECTOR ( 'NONE', #11076, 1000.000000000000000 ) ;
#16576 = DIRECTION ( 'NONE',  ( 1.000000000000000000, 0.000000000000000000, 0.000000000000000000 ) ) ;
#16577 = LINE ( 'NONE', #28012, #27731 ) ;
#16578 = ORIENTED_EDGE ( 'NONE', *, *, #28428, .T. ) ;
#16579 = PLANE ( 'NONE',  #29768 ) ;
#16580 = DIRECTION ( 'NONE',  ( 1.000000000000000000, 0.000000000000000000, 0.000000000000000000 ) ) ;
#16581 = DIRECTION ( 'NONE',  ( 0.000000000000000000, 0.000000000000000000, 1.000000000000000000 ) ) ;
#16582 = ORIENTED_EDGE ( 'NONE', *, *, #21533, .F. ) ;
#16583 = CIRCLE ( 'NONE', #20764, 2.000000000000001776 ) ;
#16584 = EDGE_CURVE ( 'NONE', #21660, #14230, #14883, .T. ) ;
#16585 = ORIENTED_EDGE ( 'NONE', *, *, #7390, .F. ) ;
#16586 = ORIENTED_EDGE ( 'NONE', *, *, #3033, .F. ) ;
#16587 = EDGE_CURVE ( 'NONE', #27152, #11435, #2322, .T. ) ;
#16588 = DIRECTION ( 'NONE',  ( 1.000000000000000000, 0.000000000000000000, 0.000000000000000000 ) ) ;
#16589 = FACE_OUTER_BOUND ( 'NONE', #21430, .T. ) ;
#16590 = ORIENTED_EDGE ( 'NONE', *, *, #22016, .T. ) ;
#16591 = AXIS2_PLACEMENT_3D ( 'NONE', #16517, #28495, #28141 ) ;
#16592 = CARTESIAN_POINT ( 'NONE',  ( -30.00000337463118427, 69.28203230275516944, -5.000000000000000000 ) ) ;
#16593 = AXIS2_PLACEMENT_3D ( 'NONE', #31684, #3184, #26055 ) ;
#16594 = CYLINDRICAL_SURFACE ( 'NONE', #11124, 2.000000000000001776 ) ;
#16595 = VERTEX_POINT ( 'NONE', #14104 ) ;
#16596 = AXIS2_PLACEMENT_3D ( 'NONE', #2658, #11467, #25545 ) ;
#16597 = CARTESIAN_POINT ( 'NONE',  ( 21.64608276454480063, -107.6288746094956537, 32.49999999999999289 ) ) ;
#16598 = ORIENTED_EDGE ( 'NONE', *, *, #16201, .F. ) ;
#16599 = DIRECTION ( 'NONE',  ( 1.000000000000000000, 0.000000000000000000, 0.000000000000000000 ) ) ;
#16600 = AXIS2_PLACEMENT_3D ( 'NONE', #24011, #35458, #27366 ) ;
#16601 = AXIS2_PLACEMENT_3D ( 'NONE', #2618, #36941, #11248 ) ;
#16602 = VECTOR ( 'NONE', #22371, 1000.000000000000000 ) ;
#16603 = DIRECTION ( 'NONE',  ( -0.000000000000000000, -0.8660254037844414832, 0.4999999999999953371 ) ) ;
#16604 = CARTESIAN_POINT ( 'NONE',  ( 77.99999662536833966, 34.64101615137759183, -9.999999999999998224 ) ) ;
#16605 = ORIENTED_EDGE ( 'NONE', *, *, #21623, .T. ) ;
#16606 = DIRECTION ( 'NONE',  ( -1.000000000000000000, 0.000000000000000000, 0.000000000000000000 ) ) ;
#16607 = ITEM_DEFINED_TRANSFORMATION ( 'NONE', 'NONE', #30925,  #21385 ) ;
#16608 = ADVANCED_FACE ( 'NONE', ( #13753 ), #2877, .F. ) ;
#16609 = CARTESIAN_POINT ( 'NONE',  ( 3.000000000000000000, 3.673940397442059868E-16, -5.974599999999999689 ) ) ;
#16610 = CARTESIAN_POINT ( 'NONE',  ( 10.21421739743242618, 84.61404610869705323, 12.50000000000000000 ) ) ;
#16611 = EDGE_LOOP ( 'NONE', ( #22099, #51 ) ) ;
#16612 = DIRECTION ( 'NONE',  ( -1.000000000000000000, 0.000000000000000000, 0.000000000000000000 ) ) ;
#16613 = LINE ( 'NONE', #2171, #9569 ) ;
#16614 = EDGE_LOOP ( 'NONE', ( #8565, #37049 ) ) ;
#16615 = CARTESIAN_POINT ( 'NONE',  ( -57.00000337463111322, -43.30127018922202353, 12.50000000000000000 ) ) ;
#16616 = AXIS2_PLACEMENT_3D ( 'NONE', #11845, #23479, #26299 ) ;
#16617 = CARTESIAN_POINT ( 'NONE',  ( -5.000003374631269537, -77.94228634059960825, 12.50000000000000000 ) ) ;
#16618 = FACE_OUTER_BOUND ( 'NONE', #15207, .T. ) ;
#16620 = AXIS2_PLACEMENT_3D ( 'NONE', #10286, #768, #7667 ) ;
#16619 = DIRECTION ( 'NONE',  ( 0.000000000000000000, 0.000000000000000000, 1.000000000000000000 ) ) ;
#16621 = ADVANCED_FACE ( 'NONE', ( #25204 ), #36631, .F. ) ;
#16622 = VERTEX_POINT ( 'NONE', #22364 ) ;
#16623 = CIRCLE ( 'NONE', #438, 2.000000000000001776 ) ;
#16624 = EDGE_LOOP ( 'NONE', ( #29351, #7138, #7650, #35850 ) ) ;
#16625 = CARTESIAN_POINT ( 'NONE',  ( 0.8144415599836856146, -5.303284638000501872, -0.2680587191991445906 ) ) ;
#16626 = CARTESIAN_POINT ( 'NONE',  ( 1.999996625368710257, -69.28203230275519786, -9.999999999999998224 ) ) ;
#16627 = MECHANICAL_DESIGN_GEOMETRIC_PRESENTATION_REPRESENTATION (  '', ( #3949 ), #8749 ) ;
#16628 = AXIS2_PLACEMENT_3D ( 'NONE', #25298, #8041, #30724 ) ;
#16629 = CARTESIAN_POINT ( 'NONE',  ( 0.000000000000000000, 55.00000000000000000, 5.000000000000000888 ) ) ;
#16630 = CIRCLE ( 'NONE', #11811, 2.000000000000001776 ) ;
#16631 = ORIENTED_EDGE ( 'NONE', *, *, #8225, .T. ) ;
#16632 = VERTEX_POINT ( 'NONE', #11644 ) ;
#16633 = EDGE_CURVE ( 'NONE', #3797, #27610, #15615, .T. ) ;
#16634 = FACE_OUTER_BOUND ( 'NONE', #36654, .T. ) ;
#16635 = CARTESIAN_POINT ( 'NONE',  ( -4.282125186551308360, 3.301216562737181892, -1.327869168827478408 ) ) ;
#16636 = CARTESIAN_POINT ( 'NONE',  ( 86.99999662536831124, -8.660254037844397956, -9.999999999999998224 ) ) ;
#16637 = VECTOR ( 'NONE', #23355, 1000.000000000000000 ) ;
#16638 = EDGE_LOOP ( 'NONE', ( #17383, #23411 ) ) ;
#16639 = ORIENTED_EDGE ( 'NONE', *, *, #22546, .T. ) ;
#16640 = CARTESIAN_POINT ( 'NONE',  ( 47.63139720814400846, -27.50000000000022737, -10.00000000000000178 ) ) ;
#16641 = DIRECTION ( 'NONE',  ( 1.000000000000000000, 0.000000000000000000, 0.000000000000000000 ) ) ;
#16642 = ORIENTED_EDGE ( 'NONE', *, *, #3208, .F. ) ;
#16643 = DIRECTION ( 'NONE',  ( 0.000000000000000000, 0.000000000000000000, 1.000000000000000000 ) ) ;
#16644 = ORIENTED_EDGE ( 'NONE', *, *, #16488, .F. ) ;
#16645 = AXIS2_PLACEMENT_3D ( 'NONE', #23733, #29521, #15841 ) ;
#16646 = FACE_BOUND ( 'NONE', #22208, .T. ) ;
#16647 = AXIS2_PLACEMENT_3D ( 'NONE', #8579, #14398, #11398 ) ;
#16648 = VECTOR ( 'NONE', #23873, 1000.000000000000000 ) ;
#16649 = CARTESIAN_POINT ( 'NONE',  ( -4.182066831946699814, 3.358985280702823761, -5.826062401966626503 ) ) ;
#16650 = EDGE_CURVE ( 'NONE', #21235, #25006, #25757, .T. ) ;
#16651 = CARTESIAN_POINT ( 'NONE',  ( -0.2117491801717998334, 5.895756138069137009, -4.027903350935056359 ) ) ;
#16652 = EDGE_LOOP ( 'NONE', ( #21887, #15335, #16506, #14293 ) ) ;
#16653 = ADVANCED_FACE ( 'NONE', ( #36800 ), #12016, .F. ) ;
#16654 = DIRECTION ( 'NONE',  ( 0.000000000000000000, 0.000000000000000000, 1.000000000000000000 ) ) ;
#16655 = CARTESIAN_POINT ( 'NONE',  ( 89.42901512340354486, -31.83425564451495404, -49.86348611802629449 ) ) ;
#16656 = VECTOR ( 'NONE', #4698, 1000.000000000000000 ) ;
#16657 = DIRECTION ( 'NONE',  ( 1.000000000000000000, 0.000000000000000000, 0.000000000000000000 ) ) ;
#16658 = DIRECTION ( 'NONE',  ( 0.000000000000000000, 0.000000000000000000, -1.000000000000000000 ) ) ;
#16659 = ORIENTED_EDGE ( 'NONE', *, *, #11063, .F. ) ;
#16660 = FACE_OUTER_BOUND ( 'NONE', #7123, .T. ) ;
#16661 = EDGE_CURVE ( 'NONE', #8789, #24647, #20289, .T. ) ;
#16662 = CARTESIAN_POINT ( 'NONE',  ( 69.99999662536839651, 17.32050807568879236, -5.000000000000000000 ) ) ;
#16663 = CIRCLE ( 'NONE', #4108, 33.00000000000002132 ) ;
#16664 = CARTESIAN_POINT ( 'NONE',  ( -5.000000000000000000, -2.886751345948137981, -5.553418012614792509 ) ) ;
#16665 = ORIENTED_EDGE ( 'NONE', *, *, #1629, .F. ) ;
#16666 = EDGE_CURVE ( 'NONE', #5840, #14472, #769, .T. ) ;
#16667 = ORIENTED_EDGE ( 'NONE', *, *, #22975, .F. ) ;
#16668 = AXIS2_PLACEMENT_3D ( 'NONE', #21243, #32884, #29878 ) ;
#16669 = DIRECTION ( 'NONE',  ( 1.000000000000000000, 0.000000000000000000, 0.000000000000000000 ) ) ;
#16670 = VERTEX_POINT ( 'NONE', #23297 ) ;
#16671 = AXIS2_PLACEMENT_3D ( 'NONE', #15284, #17925, #18668 ) ;
#16672 = CIRCLE ( 'NONE', #36434, 2.000000000000001776 ) ;
#16673 = DIRECTION ( 'NONE',  ( -1.000000000000000000, 0.000000000000000000, 0.000000000000000000 ) ) ;
#16674 = CARTESIAN_POINT ( 'NONE',  ( -72.00000337463102085, -34.64101615137762025, -9.999999999999998224 ) ) ;
#16675 = CIRCLE ( 'NONE', #25584, 2.000000000000001776 ) ;
#16676 = DIRECTION ( 'NONE',  ( 1.000000000000000000, 0.000000000000000000, 0.000000000000000000 ) ) ;
#16677 = AXIS2_PLACEMENT_3D ( 'NONE', #18006, #15184, #370 ) ;
#16678 = DIRECTION ( 'NONE',  ( 1.000000000000000000, 0.000000000000000000, 0.000000000000000000 ) ) ;
#16679 = EDGE_CURVE ( 'NONE', #23931, #17038, #9602, .T. ) ;
#16680 = CARTESIAN_POINT ( 'NONE',  ( -55.00000337463110611, -43.30127018922202353, -9.999999999999998224 ) ) ;
#16681 = DIRECTION ( 'NONE',  ( 0.000000000000000000, 0.000000000000000000, 1.000000000000000000 ) ) ;
#16682 = LINE ( 'NONE', #13854, #13030 ) ;
#16684 = VECTOR ( 'NONE', #24020, 1000.000000000000000 ) ;
#16683 = DIRECTION ( 'NONE',  ( 0.000000000000000000, 0.000000000000000000, 1.000000000000000000 ) ) ;
#16685 = VERTEX_POINT ( 'NONE', #33153 ) ;
#16686 = VERTEX_POINT ( 'NONE', #18030 ) ;
#16687 = AXIS2_PLACEMENT_3D ( 'NONE', #34959, #31924, #3469 ) ;
#16688 = EDGE_CURVE ( 'NONE', #36954, #18446, #11900, .T. ) ;
#16689 = CARTESIAN_POINT ( 'NONE',  ( 64.99999662536841072, 25.98076211353318854, -9.999999999999998224 ) ) ;
#16690 = DIRECTION ( 'NONE',  ( 0.000000000000000000, 0.000000000000000000, 1.000000000000000000 ) ) ;
#16691 = DIRECTION ( 'NONE',  ( 0.000000000000000000, 0.000000000000000000, 1.000000000000000000 ) ) ;
#16692 = DIRECTION ( 'NONE',  ( 1.000000000000000000, 0.000000000000000000, 0.000000000000000000 ) ) ;
#16693 = ORIENTED_EDGE ( 'NONE', *, *, #33157, .F. ) ;
#16694 = PRODUCT_DEFINITION_CONTEXT ( 'detailed design', #11816, 'design' ) ;
#16695 = CIRCLE ( 'NONE', #10108, 1.999999999999998224 ) ;
#16696 = EDGE_CURVE ( 'NONE', #25889, #7714, #16713, .T. ) ;
#16697 = DIRECTION ( 'NONE',  ( 1.000000000000000000, 0.000000000000000000, 0.000000000000000000 ) ) ;
#16698 = CIRCLE ( 'NONE', #26859, 0.2999999999999999334 ) ;
#16699 = ORIENTED_EDGE ( 'NONE', *, *, #30542, .F. ) ;
#16700 = ORIENTED_EDGE ( 'NONE', *, *, #23918, .F. ) ;
#16701 = ADVANCED_FACE ( 'NONE', ( #403 ), #9037, .F. ) ;
#16702 = CIRCLE ( 'NONE', #521, 6.000000000000005329 ) ;
#16703 = CARTESIAN_POINT ( 'NONE',  ( 3.000000000000000000, 0.000000000000000000, 0.000000000000000000 ) ) ;
#16704 = EDGE_LOOP ( 'NONE', ( #29144, #7735, #11979, #4148, #581, #27613 ) ) ;
#16705 = DIRECTION ( 'NONE',  ( -1.000000000000000000, 0.000000000000000000, 0.000000000000000000 ) ) ;
#16706 = DIRECTION ( 'NONE',  ( 0.000000000000000000, 0.000000000000000000, -1.000000000000000000 ) ) ;
#16707 = CARTESIAN_POINT ( 'NONE',  ( 47.99999662536848177, -51.96152422706640550, -9.999999999999998224 ) ) ;
#16708 = ORIENTED_EDGE ( 'NONE', *, *, #36365, .T. ) ;
#16709 = ORIENTED_EDGE ( 'NONE', *, *, #14252, .F. ) ;
#16710 = EDGE_CURVE ( 'NONE', #18201, #12378, #6216, .T. ) ;
#16711 = AXIS2_PLACEMENT_3D ( 'NONE', #14419, #28834, #11579 ) ;
#16712 = ORIENTED_EDGE ( 'NONE', *, *, #12263, .T. ) ;
#16713 = CIRCLE ( 'NONE', #23288, 2.000000000000001776 ) ;
#16714 = ORIENTED_EDGE ( 'NONE', *, *, #6698, .F. ) ;
#16715 = AXIS2_PLACEMENT_3D ( 'NONE', #35982, #24344, #35790 ) ;
#16716 = EDGE_CURVE ( 'NONE', #25787, #37029, #22095, .T. ) ;
#16717 = ORIENTED_EDGE ( 'NONE', *, *, #7145, .F. ) ;
#16718 = CARTESIAN_POINT ( 'NONE',  ( -45.00000337463112743, -60.62177826491080168, -9.999999999999998224 ) ) ;
#16719 = CARTESIAN_POINT ( 'NONE',  ( 56.67878100130369035, -27.78182860042797131, -49.86348611802629449 ) ) ;
#16720 = CARTESIAN_POINT ( 'NONE',  ( 35.19434990244975126, -52.39915983220758022, -4.999999999999997335 ) ) ;
#16721 = DIRECTION ( 'NONE',  ( 0.000000000000000000, 0.000000000000000000, 1.000000000000000000 ) ) ;
#16722 = CARTESIAN_POINT ( 'NONE',  ( 5.236773920621756062, 1.020523963592002925, -4.056123266998443277 ) ) ;
#16723 = ORIENTED_EDGE ( 'NONE', *, *, #17382, .T. ) ;
#16724 = CARTESIAN_POINT ( 'NONE',  ( 34.00000000000000000, -103.4105893997321743, 32.50000000000000000 ) ) ;
#16725 = CARTESIAN_POINT ( 'NONE',  ( -65.00000337463102085, 25.98076211353317433, 17.49999999999999645 ) ) ;
#16726 = AXIS2_PLACEMENT_3D ( 'NONE', #21543, #15726, #13101 ) ;
#16727 = DIRECTION ( 'NONE',  ( 0.000000000000000000, 0.000000000000000000, -1.000000000000000000 ) ) ;
#16728 = ORIENTED_EDGE ( 'NONE', *, *, #27242, .T. ) ;
#16729 = FACE_OUTER_BOUND ( 'NONE', #26619, .T. ) ;
#16730 = CIRCLE ( 'NONE', #14929, 33.00000000000001421 ) ;
#16731 = DIRECTION ( 'NONE',  ( 1.000000000000000000, 0.000000000000000000, 0.000000000000000000 ) ) ;
#16732 = ORIENTED_EDGE ( 'NONE', *, *, #6450, .F. ) ;
#16733 = ORIENTED_EDGE ( 'NONE', *, *, #2941, .F. ) ;
#16734 = ADVANCED_FACE ( 'NONE', ( #10287 ), #27347, .F. ) ;
#16735 = CARTESIAN_POINT ( 'NONE',  ( 51.99999662536847467, -69.28203230275519786, 12.50000000000000000 ) ) ;
#16736 = AXIS2_PLACEMENT_3D ( 'NONE', #3845, #33088, #13032 ) ;
#16737 = CARTESIAN_POINT ( 'NONE',  ( 0.2117491801717859834, 5.895756138069137009, -4.027903350935056359 ) ) ;
#16738 = FACE_BOUND ( 'NONE', #21324, .T. ) ;
#16739 = DIRECTION ( 'NONE',  ( 0.000000000000000000, 0.4999999999999997224, -0.8660254037844388186 ) ) ;
#16740 = ORIENTED_EDGE ( 'NONE', *, *, #11014, .T. ) ;
#16741 = EDGE_LOOP ( 'NONE', ( #22508, #10731, #16989, #2203 ) ) ;
#16742 = AXIS2_PLACEMENT_3D ( 'NONE', #17974, #9537, #29400 ) ;
#16743 = EDGE_CURVE ( 'NONE', #5023, #14473, #2343, .T. ) ;
#16744 = PLANE ( 'NONE',  #12276 ) ;
#16745 = CIRCLE ( 'NONE', #20935, 2.000000000000001776 ) ;
#16746 = VERTEX_POINT ( 'NONE', #9209 ) ;
#16747 = EDGE_CURVE ( 'NONE', #8382, #9458, #28080, .T. ) ;
#16748 = AXIS2_PLACEMENT_3D ( 'NONE', #34797, #26521, #29150 ) ;
#16749 = EDGE_CURVE ( 'NONE', #17257, #27540, #13105, .T. ) ;
#16750 = CARTESIAN_POINT ( 'NONE',  ( -4.279621169095561228, 62.97617850287782915, 12.49999999999999822 ) ) ;
#16751 = VERTEX_POINT ( 'NONE', #32071 ) ;
#16752 = CARTESIAN_POINT ( 'NONE',  ( -78.00000337463094979, -2.428612866367529932E-14, 17.49999999999999645 ) ) ;
#16753 = CARTESIAN_POINT ( 'NONE',  ( 0.000000000000000000, 2.935248768560057453, -3.903127820947815962E-15 ) ) ;
#16754 = CIRCLE ( 'NONE', #35922, 2.000000000000001776 ) ;
#16755 = CARTESIAN_POINT ( 'NONE',  ( -13.89091430021420237, -62.33939050065180254, 12.49999999999999822 ) ) ;
#16756 = ORIENTED_EDGE ( 'NONE', *, *, #24797, .T. ) ;
#16757 = ORIENTED_EDGE ( 'NONE', *, *, #27532, .F. ) ;
#16758 = CARTESIAN_POINT ( 'NONE',  ( -17.00000337463126243, 77.94228634059957983, 17.49999999999999645 ) ) ;
#16759 = DIRECTION ( 'NONE',  ( 0.000000000000000000, 0.000000000000000000, 1.000000000000000000 ) ) ;
#16760 = LINE ( 'NONE', #22005, #25268 ) ;
#16761 = CARTESIAN_POINT ( 'NONE',  ( 4.597743007729422793, 3.118994528718954662, -0.4198507760575557746 ) ) ;
#16762 = EDGE_CURVE ( 'NONE', #20325, #14036, #2760, .T. ) ;
#16763 = ORIENTED_EDGE ( 'NONE', *, *, #33907, .T. ) ;
#16764 = DIRECTION ( 'NONE',  ( 0.000000000000000000, 0.000000000000000000, 1.000000000000000000 ) ) ;
#16765 = FACE_BOUND ( 'NONE', #15062, .T. ) ;
#16766 = DIRECTION ( 'NONE',  ( -1.000000000000000000, 0.000000000000000000, 0.000000000000000000 ) ) ;
#16767 = CARTESIAN_POINT ( 'NONE',  ( 19.13981058454793072, -60.93295298010985306, 12.49999999999999822 ) ) ;
#16768 = CARTESIAN_POINT ( 'NONE',  ( 69.99999662536838230, -34.64101615137759183, -9.999999999999998224 ) ) ;
#16769 = AXIS2_PLACEMENT_3D ( 'NONE', #11506, #25231, #10791 ) ;
#16770 = FACE_OUTER_BOUND ( 'NONE', #2436, .T. ) ;
#16771 = CIRCLE ( 'NONE', #13146, 33.00000000000001421 ) ;
#16772 = DIRECTION ( 'NONE',  ( 1.000000000000000000, 0.000000000000000000, 0.000000000000000000 ) ) ;
#16773 = CIRCLE ( 'NONE', #29333, 45.00000000000000711 ) ;
#16774 = DIRECTION ( 'NONE',  ( 1.000000000000000000, 0.000000000000000000, 0.000000000000000000 ) ) ;
#16775 = EDGE_LOOP ( 'NONE', ( #34575, #13610, #9221, #17604 ) ) ;
#16776 = DIRECTION ( 'NONE',  ( 0.000000000000000000, 0.000000000000000000, -1.000000000000000000 ) ) ;
#16777 = DIRECTION ( 'NONE',  ( 0.000000000000000000, 0.000000000000000000, 1.000000000000000000 ) ) ;
#16778 = CIRCLE ( 'NONE', #36535, 3.500000000000003109 ) ;
#16779 = CYLINDRICAL_SURFACE ( 'NONE', #22788, 3.000000000000002665 ) ;
#16780 = ORIENTED_EDGE ( 'NONE', *, *, #13392, .F. ) ;
#16781 = ORIENTED_EDGE ( 'NONE', *, *, #21087, .T. ) ;
#16782 = EDGE_CURVE ( 'NONE', #16375, #35812, #356, .T. ) ;
#16783 = EDGE_LOOP ( 'NONE', ( #34691, #10626, #8857, #20576 ) ) ;
#16784 = VECTOR ( 'NONE', #3101, 1000.000000000000000 ) ;
#16785 = CARTESIAN_POINT ( 'NONE',  ( 0.000000000000000000, 0.000000000000000000, -5.000000000000000000 ) ) ;
#16786 = DIRECTION ( 'NONE',  ( 0.000000000000000000, 0.000000000000000000, 1.000000000000000000 ) ) ;
#16787 = EDGE_CURVE ( 'NONE', #5093, #3514, #26708, .T. ) ;
#16788 = ORIENTED_EDGE ( 'NONE', *, *, #33924, .F. ) ;
#16789 = DIRECTION ( 'NONE',  ( 0.000000000000000000, 0.000000000000000000, -1.000000000000000000 ) ) ;
#16790 = VERTEX_POINT ( 'NONE', #29452 ) ;
#16791 = CIRCLE ( 'NONE', #1234, 27.00000000000001776 ) ;
#16792 = CARTESIAN_POINT ( 'NONE',  ( 18.19094855014379064, -112.1612271170976953, 32.50000000000000000 ) ) ;
#16794 = EDGE_CURVE ( 'NONE', #12265, #9206, #10547, .T. ) ;
#16793 = ORIENTED_EDGE ( 'NONE', *, *, #20152, .T. ) ;
#16795 = CYLINDRICAL_SURFACE ( 'NONE', #23132, 1.999999999999998224 ) ;
#16796 = AXIS2_PLACEMENT_3D ( 'NONE', #36390, #16496, #27929 ) ;
#16797 = VERTEX_POINT ( 'NONE', #6767 ) ;
#16798 = CARTESIAN_POINT ( 'NONE',  ( -1.443735181952766622, 4.939961795957295898, -5.918341802876230240 ) ) ;
#16799 = DIRECTION ( 'NONE',  ( -0.4999999999999977796, 0.8660254037844398178, 0.000000000000000000 ) ) ;
#16800 = CIRCLE ( 'NONE', #28163, 33.00000000000001421 ) ;
#16801 = ORIENTED_EDGE ( 'NONE', *, *, #24487, .T. ) ;
#16802 = DIRECTION ( 'NONE',  ( 0.000000000000000000, 0.000000000000000000, 1.000000000000000000 ) ) ;
#16803 = VECTOR ( 'NONE', #914, 1000.000000000000000 ) ;
#16804 = EDGE_CURVE ( 'NONE', #31233, #31147, #9359, .T. ) ;
#16805 = CARTESIAN_POINT ( 'NONE',  ( -27.00000337463121625, -77.94228634059963667, -9.999999999999998224 ) ) ;
#16806 = EDGE_CURVE ( 'NONE', #1952, #30663, #20126, .T. ) ;
#16807 = FACE_OUTER_BOUND ( 'NONE', #20597, .T. ) ;
#16808 = EDGE_CURVE ( 'NONE', #30244, #36248, #8169, .T. ) ;
#16809 = ORIENTED_EDGE ( 'NONE', *, *, #13309, .T. ) ;
#16810 = LINE ( 'NONE', #28044, #31143 ) ;
#16811 = DIRECTION ( 'NONE',  ( 0.000000000000000000, 0.000000000000000000, 1.000000000000000000 ) ) ;
#16812 = EDGE_CURVE ( 'NONE', #36782, #5705, #36898, .T. ) ;
#16813 = ORIENTED_EDGE ( 'NONE', *, *, #34196, .F. ) ;
#16814 = DIRECTION ( 'NONE',  ( 1.000000000000000000, 0.000000000000000000, 0.000000000000000000 ) ) ;
#16815 = CARTESIAN_POINT ( 'NONE',  ( -5.000000000000000888, 6.123233995736767268E-16, 13.31572692736085095 ) ) ;
#16816 = CARTESIAN_POINT ( 'NONE',  ( 5.029396762153802491, -2.903723574490945314, -4.151008977024209123 ) ) ;
#16817 = CARTESIAN_POINT ( 'NONE',  ( 0.000000000000000000, 0.000000000000000000, -5.000000000000000000 ) ) ;
#16818 = ORIENTED_EDGE ( 'NONE', *, *, #18603, .T. ) ;
#16819 = ORIENTED_EDGE ( 'NONE', *, *, #24538, .F. ) ;
#16820 = CARTESIAN_POINT ( 'NONE',  ( 2.500000000000021760, -4.330127018922177662, 0.000000000000000000 ) ) ;
#16821 = DIRECTION ( 'NONE',  ( -1.000000000000000000, 0.000000000000000000, 0.000000000000000000 ) ) ;
#16822 = VERTEX_POINT ( 'NONE', #19292 ) ;
#16823 = EDGE_LOOP ( 'NONE', ( #4565, #15329, #25873, #28252 ) ) ;
#16824 = CIRCLE ( 'NONE', #1851, 3.000000000000002665 ) ;
#16825 = CARTESIAN_POINT ( 'NONE',  ( 4.999999999999999112, -1.947799557644004809, -0.2684016432552360221 ) ) ;
#16826 = DIRECTION ( 'NONE',  ( -1.000000000000000000, 0.000000000000000000, 0.000000000000000000 ) ) ;
#16827 = DIRECTION ( 'NONE',  ( 0.000000000000000000, 0.000000000000000000, 1.000000000000000000 ) ) ;
#16828 = EDGE_CURVE ( 'NONE', #5222, #25776, #3959, .T. ) ;
#16829 = EDGE_LOOP ( 'NONE', ( #19272, #33866, #18328, #994 ) ) ;
#16830 = VERTEX_POINT ( 'NONE', #5026 ) ;
#16831 = DIRECTION ( 'NONE',  ( 0.000000000000000000, 0.000000000000000000, -1.000000000000000000 ) ) ;
#16832 = DIRECTION ( 'NONE',  ( 0.000000000000000000, 0.000000000000000000, 1.000000000000000000 ) ) ;
#16833 = ORIENTED_EDGE ( 'NONE', *, *, #24311, .T. ) ;
#16834 = DIRECTION ( 'NONE',  ( 1.000000000000000000, 0.000000000000000000, 0.000000000000000000 ) ) ;
#16835 = ORIENTED_EDGE ( 'NONE', *, *, #36133, .F. ) ;
#16836 = FACE_BOUND ( 'NONE', #25350, .T. ) ;
#16837 = CARTESIAN_POINT ( 'NONE',  ( -110.2237710830543733, -101.7384897088139724, 27.50000000000000000 ) ) ;
#16838 = ORIENTED_EDGE ( 'NONE', *, *, #24022, .T. ) ;
#16839 = DIRECTION ( 'NONE',  ( 0.000000000000000000, 0.000000000000000000, 1.000000000000000000 ) ) ;
#16840 = DIRECTION ( 'NONE',  ( 1.000000000000000000, 0.000000000000000000, 0.000000000000000000 ) ) ;
#16841 = CYLINDRICAL_SURFACE ( 'NONE', #19751, 2.000000000000001776 ) ;
#16842 = CARTESIAN_POINT ( 'NONE',  ( -43.00000337463111322, 77.94228634059959404, -5.000000000000000000 ) ) ;
#16843 = AXIS2_PLACEMENT_3D ( 'NONE', #4446, #9524, #23773 ) ;
#16844 = EDGE_CURVE ( 'NONE', #1473, #731, #3367, .T. ) ;
#16845 = ORIENTED_EDGE ( 'NONE', *, *, #35016, .T. ) ;
#16846 = DIRECTION ( 'NONE',  ( 0.000000000000000000, 0.000000000000000000, 1.000000000000000000 ) ) ;
#16847 = DIRECTION ( 'NONE',  ( 1.000000000000000000, 0.000000000000000000, 0.000000000000000000 ) ) ;
#16848 = CARTESIAN_POINT ( 'NONE',  ( 3.000000000000000888, 3.673940397442060854E-16, -5.674599999999998090 ) ) ;
#16849 = ORIENTED_EDGE ( 'NONE', *, *, #4652, .T. ) ;
#16850 = ORIENTED_EDGE ( 'NONE', *, *, #35016, .F. ) ;
#16851 = ORIENTED_EDGE ( 'NONE', *, *, #34447, .F. ) ;
#16852 = DIRECTION ( 'NONE',  ( 1.000000000000000000, 0.000000000000000000, 0.000000000000000000 ) ) ;
#16853 = CARTESIAN_POINT ( 'NONE',  ( 29.99999662536857770, -69.28203230275519786, -9.999999999999998224 ) ) ;
#16854 = CARTESIAN_POINT ( 'NONE',  ( -7.000003374631307729, 77.94228634059957983, -5.000000000000000000 ) ) ;
#16855 = CARTESIAN_POINT ( 'NONE',  ( 0.000000000000000000, 2.935248768560057453, -3.903127820947815962E-15 ) ) ;
#16856 = CARTESIAN_POINT ( 'NONE',  ( 49.99999662536846756, 51.96152422706637708, 17.49999999999999645 ) ) ;
#16857 = CARTESIAN_POINT ( 'NONE',  ( -90.52724777280822366, -71.16956570548431671, 32.50000000000000000 ) ) ;
#16858 = VECTOR ( 'NONE', #8048, 1000.000000000000000 ) ;
#16859 = DIRECTION ( 'NONE',  ( 0.000000000000000000, 0.000000000000000000, 1.000000000000000000 ) ) ;
#16860 = EDGE_CURVE ( 'NONE', #16037, #21975, #1577, .T. ) ;
#16861 = CARTESIAN_POINT ( 'NONE',  ( 0.000000000000000000, 0.000000000000000000, 0.000000000000000000 ) ) ;
#16862 = ORIENTED_EDGE ( 'NONE', *, *, #26001, .T. ) ;
#16863 = ORIENTED_EDGE ( 'NONE', *, *, #12525, .F. ) ;
#16864 = CARTESIAN_POINT ( 'NONE',  ( 3.000000000000000000, 2.935248768560057453, -3.903127820947815962E-15 ) ) ;
#16865 = LINE ( 'NONE', #25484, #7979 ) ;
#16866 = CARTESIAN_POINT ( 'NONE',  ( -37.00000337463116296, 60.62177826491077326, -9.999999999999998224 ) ) ;
#16867 = CARTESIAN_POINT ( 'NONE',  ( -102.5304832720503185, -102.5304832720485280, 32.50000000000000000 ) ) ;
#16868 = EDGE_CURVE ( 'NONE', #4982, #32183, #9281, .T. ) ;
#16869 = ORIENTED_EDGE ( 'NONE', *, *, #23524, .F. ) ;
#16870 = EDGE_CURVE ( 'NONE', #2491, #14355, #16464, .T. ) ;
#16871 = FACE_BOUND ( 'NONE', #7259, .T. ) ;
#16872 = VERTEX_POINT ( 'NONE', #30544 ) ;
#16873 = ORIENTED_EDGE ( 'NONE', *, *, #27653, .F. ) ;
#16874 =( REPRESENTATION_RELATIONSHIP ('NONE','NONE', #15268, #33015 ) REPRESENTATION_RELATIONSHIP_WITH_TRANSFORMATION ( #19245 )SHAPE_REPRESENTATION_RELATIONSHIP( ) );
#16875 = DIRECTION ( 'NONE',  ( 0.000000000000000000, -0.5000000000000011102, -0.8660254037844379305 ) ) ;
#16876 = EDGE_LOOP ( 'NONE', ( #31669, #17957, #6870, #26004 ) ) ;
#16877 = DIRECTION ( 'NONE',  ( 0.000000000000000000, 0.000000000000000000, 1.000000000000000000 ) ) ;
#16878 = CARTESIAN_POINT ( 'NONE',  ( -51.13139720814438505, -27.49999999999955591, -5.000000000000000888 ) ) ;
#16879 = VECTOR ( 'NONE', #2498, 1000.000000000000000 ) ;
#16880 = CARTESIAN_POINT ( 'NONE',  ( -25.00000337463120914, 77.94228634059957983, -5.000000000000000000 ) ) ;
#16881 = EDGE_CURVE ( 'NONE', #28072, #13035, #12310, .T. ) ;
#16882 = VERTEX_POINT ( 'NONE', #19660 ) ;
#16883 = ORIENTED_EDGE ( 'NONE', *, *, #11358, .T. ) ;
#16884 = ORIENTED_EDGE ( 'NONE', *, *, #1403, .T. ) ;
#16885 = VERTEX_POINT ( 'NONE', #16848 ) ;
#16886 = EDGE_LOOP ( 'NONE', ( #6798, #14867, #36777, #24190, #16700 ) ) ;
#16887 = FACE_OUTER_BOUND ( 'NONE', #12971, .T. ) ;
#16888 = CYLINDRICAL_SURFACE ( 'NONE', #34733, 2.000000000000000000 ) ;
#16889 = LINE ( 'NONE', #27951, #5277 ) ;
#16890 = CARTESIAN_POINT ( 'NONE',  ( 4.999996625368645198, 77.94228634059957983, 12.50000000000000000 ) ) ;
#16891 = CARTESIAN_POINT ( 'NONE',  ( -83.45172111230354517, 31.46585318596159553, 12.49999999999999822 ) ) ;
#16892 = VERTEX_POINT ( 'NONE', #22282 ) ;
#16893 = CARTESIAN_POINT ( 'NONE',  ( 67.99999662536836809, -34.64101615137759183, -5.000000000000000000 ) ) ;
#16894 = CARTESIAN_POINT ( 'NONE',  ( -145.0000000000000000, 6.000000000001517009, 27.50000000000000000 ) ) ;
#16895 = ADVANCED_FACE ( 'NONE', ( #2587 ), #13279, .F. ) ;
#16896 = CARTESIAN_POINT ( 'NONE',  ( 79.99999662536833966, 34.64101615137759183, 12.50000000000000000 ) ) ;
#16897 = ORIENTED_EDGE ( 'NONE', *, *, #25192, .F. ) ;
#16898 = DIRECTION ( 'NONE',  ( 1.000000000000000000, 0.000000000000000000, 0.000000000000000000 ) ) ;
#16899 = CARTESIAN_POINT ( 'NONE',  ( 57.99999662536842493, -51.96152422706639840, 17.49999999999999645 ) ) ;
#16900 = ORIENTED_EDGE ( 'NONE', *, *, #35489, .F. ) ;
#16901 = ORIENTED_EDGE ( 'NONE', *, *, #3531, .F. ) ;
#16902 = DIRECTION ( 'NONE',  ( 0.000000000000000000, 0.000000000000000000, 1.000000000000000000 ) ) ;
#16903 = CIRCLE ( 'NONE', #35471, 2.000000000000000000 ) ;
#16904 = DIRECTION ( 'NONE',  ( -0.000000000000000000, -0.000000000000000000, 1.000000000000000000 ) ) ;
#16905 = FACE_BOUND ( 'NONE', #13844, .T. ) ;
#16906 = DIRECTION ( 'NONE',  ( 1.000000000000000000, 0.000000000000000000, 0.000000000000000000 ) ) ;
#16907 = EDGE_CURVE ( 'NONE', #32711, #32590, #36550, .T. ) ;
#16908 = ORIENTED_EDGE ( 'NONE', *, *, #711, .T. ) ;
#16909 = VERTEX_POINT ( 'NONE', #8025 ) ;
#16910 = CARTESIAN_POINT ( 'NONE',  ( 64.99999662536839651, -43.30127018922199511, -9.999999999999998224 ) ) ;
#16911 = EDGE_CURVE ( 'NONE', #12612, #22847, #17739, .T. ) ;
#16912 = VERTEX_POINT ( 'NONE', #30709 ) ;
#16913 = CARTESIAN_POINT ( 'NONE',  ( 0.000000000000000000, 0.000000000000000000, -5.000000000000000000 ) ) ;
#16914 = ORIENTED_EDGE ( 'NONE', *, *, #13544, .T. ) ;
#16915 = ORIENTED_EDGE ( 'NONE', *, *, #23625, .F. ) ;
#16916 = PLANE ( 'NONE',  #17005 ) ;
#16917 = CARTESIAN_POINT ( 'NONE',  ( 31.99999662536856704, 69.28203230275518365, -9.999999999999998224 ) ) ;
#16918 = DIRECTION ( 'NONE',  ( 1.000000000000000000, 0.000000000000000000, 0.000000000000000000 ) ) ;
#16919 = VERTEX_POINT ( 'NONE', #22110 ) ;
#16920 = EDGE_LOOP ( 'NONE', ( #8075, #17496, #36070, #21537 ) ) ;
#16921 = DIRECTION ( 'NONE',  ( 0.000000000000000000, 0.000000000000000000, 1.000000000000000000 ) ) ;
#16922 = CYLINDRICAL_SURFACE ( 'NONE', #11151, 2.000000000000001776 ) ;
#16923 = CARTESIAN_POINT ( 'NONE',  ( -83.00000337463092137, 8.660254037844389075, -5.000000000000000000 ) ) ;
#16924 = DIRECTION ( 'NONE',  ( 0.000000000000000000, 0.000000000000000000, 1.000000000000000000 ) ) ;
#16925 = ADVANCED_FACE ( 'NONE', ( #2221 ), #13660, .F. ) ;
#16926 = ORIENTED_EDGE ( 'NONE', *, *, #32252, .F. ) ;
#16927 = DIRECTION ( 'NONE',  ( 1.000000000000000000, 0.000000000000000000, 0.000000000000000000 ) ) ;
#16928 = AXIS2_PLACEMENT_3D ( 'NONE', #11604, #8082, #22712 ) ;
#16929 = FACE_BOUND ( 'NONE', #33719, .T. ) ;
#16930 = VECTOR ( 'NONE', #29516, 1000.000000000000000 ) ;
#16931 = DIRECTION ( 'NONE',  ( 0.000000000000000000, 0.000000000000000000, -1.000000000000000000 ) ) ;
#16932 = CARTESIAN_POINT ( 'NONE',  ( -73.00000337463097821, 43.30127018922197379, -9.999999999999998224 ) ) ;
#16933 = DIRECTION ( 'NONE',  ( 0.000000000000000000, 0.000000000000000000, -1.000000000000000000 ) ) ;
#16934 = CARTESIAN_POINT ( 'NONE',  ( 0.000000000000000000, 0.000000000000000000, -5.000000000000000000 ) ) ;
#16935 = EDGE_CURVE ( 'NONE', #20017, #10138, #25286, .T. ) ;
#16936 = PRODUCT_DEFINITION_SHAPE ( 'NONE', 'NONE',  #9065 ) ;
#16937 = CARTESIAN_POINT ( 'NONE',  ( -23.49187026334539041, 103.5527527874234863, 27.49999400000000094 ) ) ;
#16938 = EDGE_CURVE ( 'NONE', #13323, #24795, #17135, .T. ) ;
#16939 = DIRECTION ( 'NONE',  ( -0.000000000000000000, 0.000000000000000000, -1.000000000000000000 ) ) ;
#16940 = VERTEX_POINT ( 'NONE', #5774 ) ;
#16941 = CARTESIAN_POINT ( 'NONE',  ( -58.00000337463104216, 34.64101615137757051, 17.49999999999999645 ) ) ;
#16942 = CARTESIAN_POINT ( 'NONE',  ( -45.00000337463111322, -77.94228634059960825, -9.999999999999998224 ) ) ;
#16943 = DIRECTION ( 'NONE',  ( 0.000000000000000000, 0.000000000000000000, 1.000000000000000000 ) ) ;
#16944 = ORIENTED_EDGE ( 'NONE', *, *, #4288, .F. ) ;
#16945 = CIRCLE ( 'NONE', #21731, 2.000000000000001776 ) ;
#16946 = ORIENTED_EDGE ( 'NONE', *, *, #19640, .F. ) ;
#16947 = ORIENTED_EDGE ( 'NONE', *, *, #21513, .T. ) ;
#16948 = DIRECTION ( 'NONE',  ( 0.000000000000000000, -0.8660254037844420383, -0.4999999999999945599 ) ) ;
#16949 = DIRECTION ( 'NONE',  ( 0.000000000000000000, 0.000000000000000000, 1.000000000000000000 ) ) ;
#16950 = VERTEX_POINT ( 'NONE', #8580 ) ;
#16951 = CARTESIAN_POINT ( 'NONE',  ( 51.13139720814400846, -27.50000000000022737, -15.00000000000000000 ) ) ;
#16952 = EDGE_CURVE ( 'NONE', #3252, #1861, #31483, .T. ) ;
#16953 = AXIS2_PLACEMENT_3D ( 'NONE', #36556, #22288, #16852 ) ;
#16954 = ORIENTED_EDGE ( 'NONE', *, *, #11490, .F. ) ;
#16955 = PLANE ( 'NONE',  #36551 ) ;
#16956 = ORIENTED_EDGE ( 'NONE', *, *, #26871, .T. ) ;
#16957 = DIRECTION ( 'NONE',  ( 0.000000000000000000, 0.000000000000000000, -1.000000000000000000 ) ) ;
#16958 = VERTEX_POINT ( 'NONE', #9124 ) ;
#16959 = ORIENTED_EDGE ( 'NONE', *, *, #5405, .F. ) ;
#16960 = DIRECTION ( 'NONE',  ( 1.000000000000000000, 0.000000000000000000, 0.000000000000000000 ) ) ;
#16961 = CARTESIAN_POINT ( 'NONE',  ( -43.00000337463111322, 60.62177826491077326, 17.49999999999999645 ) ) ;
#16962 = VERTEX_POINT ( 'NONE', #31262 ) ;
#16963 = CARTESIAN_POINT ( 'NONE',  ( 66.99999662536842493, 43.30127018922200222, -9.999999999999998224 ) ) ;
#16964 = AXIS2_PLACEMENT_3D ( 'NONE', #1185, #29473, #7186 ) ;
#16965 = DIRECTION ( 'NONE',  ( 0.000000000000000000, 0.000000000000000000, -1.000000000000000000 ) ) ;
#16966 = FACE_OUTER_BOUND ( 'NONE', #27619, .T. ) ;
#16967 = AXIS2_PLACEMENT_3D ( 'NONE', #10691, #33931, #5602 ) ;
#16968 = EDGE_CURVE ( 'NONE', #28919, #23645, #35093, .T. ) ;
#16969 = ORIENTED_EDGE ( 'NONE', *, *, #22316, .T. ) ;
#16970 = CARTESIAN_POINT ( 'NONE',  ( -30.89873480577614018, 67.49533652152319974, 12.50000000000000000 ) ) ;
#16971 = FACE_OUTER_BOUND ( 'NONE', #21787, .T. ) ;
#16972 = VERTEX_POINT ( 'NONE', #20206 ) ;
#16973 = EDGE_CURVE ( 'NONE', #14843, #8516, #19548, .T. ) ;
#16974 = DIRECTION ( 'NONE',  ( 1.000000000000000000, 0.000000000000000000, 0.000000000000000000 ) ) ;
#16975 = CARTESIAN_POINT ( 'NONE',  ( 29.99999662536856349, 69.28203230275518365, 17.49999999999999645 ) ) ;
#16976 = CARTESIAN_POINT ( 'NONE',  ( 57.99999662536843914, -34.64101615137759893, -9.999999999999998224 ) ) ;
#16977 = DIRECTION ( 'NONE',  ( -1.000000000000000000, 0.000000000000000000, -0.000000000000000000 ) ) ;
#16978 = AXIS2_PLACEMENT_3D ( 'NONE', #7618, #25239, #21675 ) ;
#16979 = EDGE_CURVE ( 'NONE', #5117, #3388, #36909, .T. ) ;
#16980 = EDGE_LOOP ( 'NONE', ( #22547, #23983 ) ) ;
#16981 = CIRCLE ( 'NONE', #21150, 2.000000000000001776 ) ;
#16982 = ORIENTED_EDGE ( 'NONE', *, *, #29260, .F. ) ;
#16983 = EDGE_CURVE ( 'NONE', #19499, #1659, #15331, .T. ) ;
#16984 = DIRECTION ( 'NONE',  ( 1.000000000000000000, 0.000000000000000000, -0.000000000000000000 ) ) ;
#16985 = LINE ( 'NONE', #11715, #20551 ) ;
#16986 = EDGE_CURVE ( 'NONE', #34280, #35776, #29696, .T. ) ;
#16987 = AXIS2_PLACEMENT_3D ( 'NONE', #6281, #279, #8728 ) ;
#16988 = ORIENTED_EDGE ( 'NONE', *, *, #35013, .F. ) ;
#16989 = ORIENTED_EDGE ( 'NONE', *, *, #33993, .F. ) ;
#16990 = DIRECTION ( 'NONE',  ( 1.000000000000000000, 0.000000000000000000, 0.000000000000000000 ) ) ;
#16991 = DIRECTION ( 'NONE',  ( 0.5000000000000039968, 0.8660254037844363761, 0.000000000000000000 ) ) ;
#16992 = DIRECTION ( 'NONE',  ( 0.000000000000000000, 0.000000000000000000, -1.000000000000000000 ) ) ;
#16993 = EDGE_CURVE ( 'NONE', #31042, #15896, #8754, .T. ) ;
#16994 = EDGE_LOOP ( 'NONE', ( #11877, #9863, #7580, #34577, #21829, #2458 ) ) ;
#16996 = ORIENTED_EDGE ( 'NONE', *, *, #28161, .T. ) ;
#16995 = EDGE_CURVE ( 'NONE', #26437, #32411, #9330, .T. ) ;
#16997 = DIRECTION ( 'NONE',  ( 0.000000000000000000, 0.000000000000000000, 1.000000000000000000 ) ) ;
#16998 = EDGE_CURVE ( 'NONE', #7037, #20745, #13536, .T. ) ;
#16999 = FACE_OUTER_BOUND ( 'NONE', #26392, .T. ) ;
#17001 = EDGE_CURVE ( 'NONE', #10417, #10952, #17562, .T. ) ;
#17000 = ORIENTED_EDGE ( 'NONE', *, *, #7610, .F. ) ;
#17002 = CARTESIAN_POINT ( 'NONE',  ( -68.00000337463100664, -17.32050807568882078, -9.999999999999998224 ) ) ;
#17003 = EDGE_LOOP ( 'NONE', ( #7052, #27609, #28620, #16959 ) ) ;
#17004 = FACE_BOUND ( 'NONE', #16010, .T. ) ;
#17005 = AXIS2_PLACEMENT_3D ( 'NONE', #16056, #8484, #19911 ) ;
#17006 = DIRECTION ( 'NONE',  ( 1.000000000000000000, 0.000000000000000000, 0.000000000000000000 ) ) ;
#17007 = ORIENTED_EDGE ( 'NONE', *, *, #19735, .F. ) ;
#17008 = DIRECTION ( 'NONE',  ( -2.775557561562894433E-17, 1.107409718022660616E-33, 1.000000000000000000 ) ) ;
#17009 = CARTESIAN_POINT ( 'NONE',  ( -52.39915983220772233, -35.19434990244957362, 12.49999999999999822 ) ) ;
#17010 = CARTESIAN_POINT ( 'NONE',  ( -63.00000337463102085, 43.30127018922198801, -5.000000000000000000 ) ) ;
#17011 = CARTESIAN_POINT ( 'NONE',  ( 17.99999662536858125, 86.60254037844397601, 17.49999999999999645 ) ) ;
#17012 = ORIENTED_EDGE ( 'NONE', *, *, #16013, .F. ) ;
#17013 = DIRECTION ( 'NONE',  ( 0.000000000000000000, 0.000000000000000000, 1.000000000000000000 ) ) ;
#17014 = CARTESIAN_POINT ( 'NONE',  ( -60.00000337463104216, 34.64101615137757051, -9.999999999999998224 ) ) ;
#17015 = DIRECTION ( 'NONE',  ( 0.000000000000000000, 0.000000000000000000, -1.000000000000000000 ) ) ;
#17016 = ORIENTED_EDGE ( 'NONE', *, *, #31052, .T. ) ;
#17017 = CIRCLE ( 'NONE', #33182, 2.000000000000001776 ) ;
#17018 = ORIENTED_EDGE ( 'NONE', *, *, #35131, .F. ) ;
#17019 = ORIENTED_EDGE ( 'NONE', *, *, #28842, .F. ) ;
#17020 = DIRECTION ( 'NONE',  ( -0.4999999999999980016, 0.8660254037844398178, 0.000000000000000000 ) ) ;
#17021 = CIRCLE ( 'NONE', #28972, 2.000000000000000000 ) ;
#17022 = DIRECTION ( 'NONE',  ( -1.000000000000000000, 0.000000000000000000, 0.000000000000000000 ) ) ;
#17023 = AXIS2_PLACEMENT_3D ( 'NONE', #32995, #13292, #18745 ) ;
#17024 = DIRECTION ( 'NONE',  ( 0.000000000000000000, 0.000000000000000000, 1.000000000000000000 ) ) ;
#17025 = CARTESIAN_POINT ( 'NONE',  ( 79.20390285583188472, -72.31905506802638683, 32.50000000000002132 ) ) ;
#17026 = FACE_BOUND ( 'NONE', #17092, .T. ) ;
#17027 = CYLINDRICAL_SURFACE ( 'NONE', #5841, 2.000000000000001776 ) ;
#17028 = CARTESIAN_POINT ( 'NONE',  ( 71.99999662536841072, 51.96152422706640550, -9.999999999999998224 ) ) ;
#17029 = ORIENTED_EDGE ( 'NONE', *, *, #24793, .F. ) ;
#17030 = ORIENTED_EDGE ( 'NONE', *, *, #15478, .T. ) ;
#17031 = DIRECTION ( 'NONE',  ( 1.000000000000000000, 0.000000000000000000, 0.000000000000000000 ) ) ;
#17032 = VECTOR ( 'NONE', #14813, 1000.000000000000000 ) ;
#17033 = LINE ( 'NONE', #5051, #13940 ) ;
#17034 = ADVANCED_FACE ( 'NONE', ( #26389 ), #37098, .F. ) ;
#17035 = DIRECTION ( 'NONE',  ( 0.000000000000000000, -0.8660254037844419273, 0.4999999999999945599 ) ) ;
#17036 = CIRCLE ( 'NONE', #9241, 33.00000000000002132 ) ;
#17037 = DIRECTION ( 'NONE',  ( 0.000000000000000000, 0.000000000000000000, 1.000000000000000000 ) ) ;
#17038 = VERTEX_POINT ( 'NONE', #17215 ) ;
#17039 = UNCERTAINTY_MEASURE_WITH_UNIT (LENGTH_MEASURE( 1.000000000000000082E-05 ), #10504, 'distance_accuracy_value', 'NONE');
#17040 = CIRCLE ( 'NONE', #36801, 2.000000000000001776 ) ;
#17041 = B_SPLINE_CURVE_WITH_KNOTS ( 'NONE', 3,
 ( #29018, #34856, #29220, #14426, #14790, #6343, #34307, #2813 ),
 .UNSPECIFIED., .F., .F.,
 ( 4, 2, 2, 4 ),
 ( 0.002921158011986708155, 0.003648658599403065313, 0.004376159186819422037, 0.005831160361652136352 ),
 .UNSPECIFIED. ) ;
#17042 = FACE_BOUND ( 'NONE', #1796, .T. ) ;
#17043 = ORIENTED_EDGE ( 'NONE', *, *, #2006, .F. ) ;
#17044 = ORIENTED_EDGE ( 'NONE', *, *, #13313, .F. ) ;
#17045 = ADVANCED_BREP_SHAPE_REPRESENTATION ( '', ( #20313, #21385 ), #22589 ) ;
#17046 = DIRECTION ( 'NONE',  ( 0.000000000000000000, 0.000000000000000000, 1.000000000000000000 ) ) ;
#17047 = ORIENTED_EDGE ( 'NONE', *, *, #13908, .F. ) ;
#17048 = DIRECTION ( 'NONE',  ( 0.000000000000000000, 0.000000000000000000, -1.000000000000000000 ) ) ;
#17049 = CIRCLE ( 'NONE', #36810, 27.00000000000001776 ) ;
#17050 = CIRCLE ( 'NONE', #22431, 1.999999999999998224 ) ;
#17051 = VECTOR ( 'NONE', #11178, 1000.000000000000000 ) ;
#17052 = DIRECTION ( 'NONE',  ( 0.000000000000000000, 0.000000000000000000, 1.000000000000000000 ) ) ;
#17053 = AXIS2_PLACEMENT_3D ( 'NONE', #136, #11029, #11408 ) ;
#17054 = FACE_OUTER_BOUND ( 'NONE', #35687, .T. ) ;
#17055 = ORIENTED_EDGE ( 'NONE', *, *, #23431, .T. ) ;
#17056 = ORIENTED_EDGE ( 'NONE', *, *, #7680, .F. ) ;
#17057 = VERTEX_POINT ( 'NONE', #25664 ) ;
#17058 = EDGE_CURVE ( 'NONE', #33801, #31156, #5173, .T. ) ;
#17059 = VERTEX_POINT ( 'NONE', #26203 ) ;
#17060 = EDGE_LOOP ( 'NONE', ( #35073, #30608 ) ) ;
#17062 = DIRECTION ( 'NONE',  ( -1.000000000000000000, 0.000000000000000000, 0.000000000000000000 ) ) ;
#17061 = VECTOR ( 'NONE', #11930, 1000.000000000000000 ) ;
#17063 = SURFACE_SIDE_STYLE ('',( #11981 ) ) ;
#17064 = AXIS2_PLACEMENT_3D ( 'NONE', #24828, #7574, #21259 ) ;
#17065 = DIRECTION ( 'NONE',  ( 0.000000000000000000, 0.4999999999999951150, -0.8660254037844414832 ) ) ;
#17066 = DIRECTION ( 'NONE',  ( 1.000000000000000000, 0.000000000000000000, 0.000000000000000000 ) ) ;
#17067 = DIRECTION ( 'NONE',  ( 1.000000000000000000, 0.000000000000000000, 0.000000000000000000 ) ) ;
#17068 = VERTEX_POINT ( 'NONE', #31443 ) ;
#17069 = CYLINDRICAL_SURFACE ( 'NONE', #15921, 3.000000000000006217 ) ;
#17070 = MECHANICAL_DESIGN_GEOMETRIC_PRESENTATION_REPRESENTATION (  '', ( #25451 ), #21865 ) ;
#17071 = CARTESIAN_POINT ( 'NONE',  ( 20.39230124433451152, -84.64139349818795210, -5.000000000000000000 ) ) ;
#17072 = EDGE_CURVE ( 'NONE', #2028, #27460, #14568, .T. ) ;
#17073 = CARTESIAN_POINT ( 'NONE',  ( 59.99999662536842493, 51.96152422706639129, -5.000000000000000000 ) ) ;
#17074 = VERTEX_POINT ( 'NONE', #311 ) ;
#17075 = FACE_OUTER_BOUND ( 'NONE', #16886, .T. ) ;
#17076 = DIRECTION ( 'NONE',  ( 0.000000000000000000, 0.000000000000000000, 1.000000000000000000 ) ) ;
#17077 = AXIS2_PLACEMENT_3D ( 'NONE', #123, #9301, #23202 ) ;
#17078 = VERTEX_POINT ( 'NONE', #694 ) ;
#17079 = VECTOR ( 'NONE', #7374, 1000.000000000000000 ) ;
#17080 = EDGE_LOOP ( 'NONE', ( #16659, #20498 ) ) ;
#17081 = DIRECTION ( 'NONE',  ( 1.000000000000000000, 0.000000000000000000, 0.000000000000000000 ) ) ;
#17082 = CARTESIAN_POINT ( 'NONE',  ( -0.8441225671312687640, 5.568793373802039426, -4.176900509772169201 ) ) ;
#17083 = ADVANCED_FACE ( 'NONE', ( #11399 ), #11748, .F. ) ;
#17084 = LINE ( 'NONE', #28164, #24162 ) ;
#17085 = APPLICATION_CONTEXT ( 'automotive_design' ) ;
#17086 = CARTESIAN_POINT ( 'NONE',  ( -74.30619744049063513, -84.18124734178186941, 32.50000000000000000 ) ) ;
#17087 = ORIENTED_EDGE ( 'NONE', *, *, #19421, .F. ) ;
#17088 = EDGE_LOOP ( 'NONE', ( #12210, #4447 ) ) ;
#17089 = DIRECTION ( 'NONE',  ( 1.000000000000000000, 0.000000000000000000, 0.000000000000000000 ) ) ;
#17090 = DIRECTION ( 'NONE',  ( 1.000000000000000000, 0.000000000000000000, -0.000000000000000000 ) ) ;
#17091 = CIRCLE ( 'NONE', #11666, 2.000000000000000000 ) ;
#17092 = EDGE_LOOP ( 'NONE', ( #22287, #4069 ) ) ;
#17093 = CIRCLE ( 'NONE', #11090, 95.00000000000001421 ) ;
#17094 = CARTESIAN_POINT ( 'NONE',  ( 0.000000000000000000, 0.000000000000000000, 12.49999999999999822 ) ) ;
#17095 = EDGE_LOOP ( 'NONE', ( #78, #6172, #18232, #19301, #33941 ) ) ;
#17096 = AXIS2_PLACEMENT_3D ( 'NONE', #33884, #22435, #30325 ) ;
#17097 = DIRECTION ( 'NONE',  ( 0.000000000000000000, 0.000000000000000000, 1.000000000000000000 ) ) ;
#17098 = AXIS2_PLACEMENT_3D ( 'NONE', #9663, #29515, #34976 ) ;
#17099 = FACE_OUTER_BOUND ( 'NONE', #26646, .T. ) ;
#17100 = FACE_OUTER_BOUND ( 'NONE', #32871, .T. ) ;
#17101 = CIRCLE ( 'NONE', #928, 2.000000000000001776 ) ;
#17102 = EDGE_CURVE ( 'NONE', #5705, #18862, #16551, .T. ) ;
#17103 = CARTESIAN_POINT ( 'NONE',  ( 59.99999662536845335, 34.64101615137759893, -9.999999999999998224 ) ) ;
#17104 = VERTEX_POINT ( 'NONE', #34830 ) ;
#17105 = VERTEX_POINT ( 'NONE', #14958 ) ;
#17106 = CARTESIAN_POINT ( 'NONE',  ( -33.00000337463116296, 60.62177826491077326, -9.999999999999998224 ) ) ;
#17107 = CARTESIAN_POINT ( 'NONE',  ( -7.000003374631269537, -77.94228634059960825, -9.999999999999998224 ) ) ;
#17108 = ADVANCED_FACE ( 'NONE', ( #19841 ), #30347, .F. ) ;
#17109 = AXIS2_PLACEMENT_3D ( 'NONE', #22060, #2367, #7809 ) ;
#17110 = CARTESIAN_POINT ( 'NONE',  ( -77.00000337463097821, 8.660254037844374864, -9.999999999999998224 ) ) ;
#17111 = AXIS2_PLACEMENT_3D ( 'NONE', #10432, #13252, #21872 ) ;
#17112 = CARTESIAN_POINT ( 'NONE',  ( 20.00000000000001066, 89.94802294027088863, 27.49999999999999645 ) ) ;
#17113 = ORIENTED_EDGE ( 'NONE', *, *, #3628, .F. ) ;
#17114 = CARTESIAN_POINT ( 'NONE',  ( 51.99999662536848888, -51.96152422706640550, -9.999999999999998224 ) ) ;
#17115 = FACE_BOUND ( 'NONE', #35345, .T. ) ;
#17116 = EDGE_CURVE ( 'NONE', #9729, #5735, #988, .T. ) ;
#17117 = FACE_OUTER_BOUND ( 'NONE', #16624, .T. ) ;
#17118 = PLANE ( 'NONE',  #30655 ) ;
#17119 = FACE_OUTER_BOUND ( 'NONE', #14896, .T. ) ;
#17120 = CARTESIAN_POINT ( 'NONE',  ( -39.27785635698568711, 86.50000000000001421, 27.50000000000000000 ) ) ;
#17121 = CARTESIAN_POINT ( 'NONE',  ( -12.25360682529215772, 116.9391560352561896, 27.49998800000000188 ) ) ;
#17122 = EDGE_CURVE ( 'NONE', #20328, #9458, #35408, .T. ) ;
#17123 = CIRCLE ( 'NONE', #35082, 2.000000000000001776 ) ;
#17124 = CARTESIAN_POINT ( 'NONE',  ( 4.999999999999999112, -1.924500897298765612, -3.818275046351163660 ) ) ;
#17125 = ORIENTED_EDGE ( 'NONE', *, *, #26726, .T. ) ;
#17127 = VECTOR ( 'NONE', #36414, 1000.000000000000000 ) ;
#17126 = DIRECTION ( 'NONE',  ( 1.000000000000000000, 0.000000000000000000, 0.000000000000000000 ) ) ;
#17128 = DIRECTION ( 'NONE',  ( -1.000000000000000000, 0.000000000000000000, 0.000000000000000000 ) ) ;
#17129 = DIRECTION ( 'NONE',  ( 1.000000000000000000, 0.000000000000000000, 0.000000000000000000 ) ) ;
#17130 = CIRCLE ( 'NONE', #954, 2.000000000000001776 ) ;
#17131 = AXIS2_PLACEMENT_3D ( 'NONE', #18189, #27009, #29620 ) ;
#17132 = AXIS2_PLACEMENT_3D ( 'NONE', #1237, #23938, #34989 ) ;
#17133 = ORIENTED_EDGE ( 'NONE', *, *, #36124, .F. ) ;
#17134 = ORIENTED_EDGE ( 'NONE', *, *, #13799, .F. ) ;
#17135 = CIRCLE ( 'NONE', #32700, 95.00000000000000000 ) ;
#17136 = ORIENTED_EDGE ( 'NONE', *, *, #2, .F. ) ;
#17137 = DIRECTION ( 'NONE',  ( 0.000000000000000000, 0.000000000000000000, -1.000000000000000000 ) ) ;
#17138 = CARTESIAN_POINT ( 'NONE',  ( 0.000000000000000000, 0.000000000000000000, 0.000000000000000000 ) ) ;
#17139 = FACE_OUTER_BOUND ( 'NONE', #25236, .T. ) ;
#17140 = EDGE_LOOP ( 'NONE', ( #28596, #26441 ) ) ;
#17141 = AXIS2_PLACEMENT_3D ( 'NONE', #28427, #13996, #117 ) ;
#17142 = CARTESIAN_POINT ( 'NONE',  ( 0.000000000000000000, 0.000000000000000000, -5.674599999999998090 ) ) ;
#17143 = EDGE_CURVE ( 'NONE', #33988, #20247, #34535, .T. ) ;
#17144 = VERTEX_POINT ( 'NONE', #29380 ) ;
#17145 = FACE_OUTER_BOUND ( 'NONE', #23806, .T. ) ;
#17146 = ORIENTED_EDGE ( 'NONE', *, *, #5044, .F. ) ;
#17147 = CARTESIAN_POINT ( 'NONE',  ( -67.00000337463102085, 43.30127018922198801, -9.999999999999998224 ) ) ;
#17148 = ORIENTED_EDGE ( 'NONE', *, *, #3107, .F. ) ;
#17149 = AXIS2_PLACEMENT_3D ( 'NONE', #32501, #20695, #17901 ) ;
#17150 = ORIENTED_EDGE ( 'NONE', *, *, #1588, .F. ) ;
#17151 = EDGE_CURVE ( 'NONE', #30760, #859, #5788, .T. ) ;
#17152 = DIRECTION ( 'NONE',  ( 0.000000000000000000, 0.4999999999999953926, 0.8660254037844412611 ) ) ;
#17153 = CARTESIAN_POINT ( 'NONE',  ( 0.000000000000000000, 85.61789592134881843, -27.49999999999990408 ) ) ;
#17154 = AXIS2_PLACEMENT_3D ( 'NONE', #12759, #36215, #4534 ) ;
#17155 = EDGE_CURVE ( 'NONE', #8160, #31719, #9515, .T. ) ;
#17156 = ORIENTED_EDGE ( 'NONE', *, *, #16312, .F. ) ;
#17157 = AXIS2_PLACEMENT_3D ( 'NONE', #14390, #25108, #25278 ) ;
#17158 = DIRECTION ( 'NONE',  ( 1.000000000000000000, 0.000000000000000000, 0.000000000000000000 ) ) ;
#17159 = AXIS2_PLACEMENT_3D ( 'NONE', #989, #28756, #236 ) ;
#17160 = AXIS2_PLACEMENT_3D ( 'NONE', #24642, #10371, #21804 ) ;
#17161 = CONTEXT_DEPENDENT_SHAPE_REPRESENTATION ( #24556, #12468 ) ;
#17162 = VECTOR ( 'NONE', #18591, 1000.000000000000000 ) ;
#17163 = AXIS2_PLACEMENT_3D ( 'NONE', #33780, #2084, #22723 ) ;
#17164 = DIRECTION ( 'NONE',  ( -0.000000000000000000, -0.000000000000000000, 1.000000000000000000 ) ) ;
#17165 = DIRECTION ( 'NONE',  ( 0.000000000000000000, 0.000000000000000000, 1.000000000000000000 ) ) ;
#17166 = AXIS2_PLACEMENT_3D ( 'NONE', #28049, #21864, #33310 ) ;
#17167 = ORIENTED_EDGE ( 'NONE', *, *, #6046, .F. ) ;
#17168 = DIRECTION ( 'NONE',  ( 0.000000000000000000, 0.000000000000000000, 1.000000000000000000 ) ) ;
#17169 = CARTESIAN_POINT ( 'NONE',  ( -47.63139720814380951, 27.50000000000055422, -10.00000000000000000 ) ) ;
#17170 = ORIENTED_EDGE ( 'NONE', *, *, #21716, .F. ) ;
#17171 = DIRECTION ( 'NONE',  ( 0.000000000000000000, 0.000000000000000000, 1.000000000000000000 ) ) ;
#17172 = FACE_OUTER_BOUND ( 'NONE', #909, .T. ) ;
#17173 = CARTESIAN_POINT ( 'NONE',  ( 0.000000000000000000, 89.94802294027088863, -19.99999999999999645 ) ) ;
#17174 = DIRECTION ( 'NONE',  ( -0.000000000000000000, -0.000000000000000000, 1.000000000000000000 ) ) ;
#17175 = CIRCLE ( 'NONE', #3996, 2.000000000000001776 ) ;
#17176 = ORIENTED_EDGE ( 'NONE', *, *, #33516, .T. ) ;
#17177 = EDGE_CURVE ( 'NONE', #2812, #20017, #33334, .T. ) ;
#17178 = ORIENTED_EDGE ( 'NONE', *, *, #6914, .F. ) ;
#17179 = DIRECTION ( 'NONE',  ( -1.000000000000000000, 8.994862468027885935E-16, 0.000000000000000000 ) ) ;
#17180 = DIRECTION ( 'NONE',  ( 0.8660254037844344888, -0.5000000000000071054, 0.000000000000000000 ) ) ;
#17181 = CIRCLE ( 'NONE', #35732, 5.999999999999999112 ) ;
#17182 = ORIENTED_EDGE ( 'NONE', *, *, #13797, .F. ) ;
#17183 = ORIENTED_EDGE ( 'NONE', *, *, #13796, .F. ) ;
#17184 = CIRCLE ( 'NONE', #25557, 27.00000000000001066 ) ;
#17185 = CARTESIAN_POINT ( 'NONE',  ( -25.00000337463121980, -77.94228634059963667, 17.49999999999999645 ) ) ;
#17186 = DIRECTION ( 'NONE',  ( 1.000000000000000000, 0.000000000000000000, 0.000000000000000000 ) ) ;
#17187 = AXIS2_PLACEMENT_3D ( 'NONE', #1604, #30098, #7607 ) ;
#17188 = VECTOR ( 'NONE', #9375, 1000.000000000000000 ) ;
#17189 = EDGE_LOOP ( 'NONE', ( #27843, #11818 ) ) ;
#17190 = AXIS2_PLACEMENT_3D ( 'NONE', #26703, #18260, #23712 ) ;
#17191 = EDGE_CURVE ( 'NONE', #23997, #10138, #3403, .T. ) ;
#17192 = LINE ( 'NONE', #14548, #6929 ) ;
#17193 = VERTEX_POINT ( 'NONE', #23958 ) ;
#17194 = ADVANCED_FACE ( 'NONE', ( #1068 ), #26943, .F. ) ;
#17195 = LINE ( 'NONE', #22265, #2365 ) ;
#17196 = ORIENTED_EDGE ( 'NONE', *, *, #19474, .T. ) ;
#17197 = DIRECTION ( 'NONE',  ( -1.000000000000000000, 0.000000000000000000, 0.000000000000000000 ) ) ;
#17198 = AXIS2_PLACEMENT_3D ( 'NONE', #10747, #2307, #5486 ) ;
#17199 = EDGE_CURVE ( 'NONE', #530, #28731, #20757, .T. ) ;
#17200 = FACE_OUTER_BOUND ( 'NONE', #15634, .T. ) ;
#17201 = CARTESIAN_POINT ( 'NONE',  ( 34.99999662536855283, -77.94228634059960825, 12.50000000000000000 ) ) ;
#17202 = EDGE_CURVE ( 'NONE', #12874, #12408, #7257, .T. ) ;
#17203 = CIRCLE ( 'NONE', #26194, 2.000000000000001776 ) ;
#17204 = ORIENTED_EDGE ( 'NONE', *, *, #23617, .T. ) ;
#17205 = EDGE_CURVE ( 'NONE', #8894, #8910, #36337, .T. ) ;
#17206 = CARTESIAN_POINT ( 'NONE',  ( 47.63139720814418610, 27.49999999999988987, 10.70000000000000107 ) ) ;
#17207 = AXIS2_PLACEMENT_3D ( 'NONE', #3565, #3180, #32019 ) ;
#17208 = DIRECTION ( 'NONE',  ( 1.000000000000000000, 0.000000000000000000, 0.000000000000000000 ) ) ;
#17209 = AXIS2_PLACEMENT_3D ( 'NONE', #18266, #1392, #35721 ) ;
#17210 = DIRECTION ( 'NONE',  ( -0.000000000000000000, 0.8660254037844420383, -0.4999999999999945599 ) ) ;
#17211 = CARTESIAN_POINT ( 'NONE',  ( -110.2237710830522559, 101.7384897088162745, 32.55002500000000509 ) ) ;
#17212 = VERTEX_POINT ( 'NONE', #35215 ) ;
#17213 = DIRECTION ( 'NONE',  ( 1.000000000000000000, 0.000000000000000000, 0.000000000000000000 ) ) ;
#17214 = DIRECTION ( 'NONE',  ( -1.000000000000000000, 0.000000000000000000, 0.000000000000000000 ) ) ;
#17215 = CARTESIAN_POINT ( 'NONE',  ( 71.99999662536839651, -17.32050807568879947, 17.49999999999999645 ) ) ;
#17216 = EDGE_CURVE ( 'NONE', #31694, #18695, #29737, .T. ) ;
#17217 = AXIS2_PLACEMENT_3D ( 'NONE', #3643, #28768, #31917 ) ;
#17218 = AXIS2_PLACEMENT_3D ( 'NONE', #28279, #13296, #19309 ) ;
#17219 = EDGE_CURVE ( 'NONE', #18518, #6148, #18516, .T. ) ;
#17220 = ORIENTED_EDGE ( 'NONE', *, *, #22499, .T. ) ;
#17221 = AXIS2_PLACEMENT_3D ( 'NONE', #34597, #6805, #35148 ) ;
#17222 = EDGE_LOOP ( 'NONE', ( #30226, #8682 ) ) ;
#17223 = EDGE_CURVE ( 'NONE', #30348, #4797, #3989, .T. ) ;
#17225 = EDGE_CURVE ( 'NONE', #1819, #30350, #26738, .T. ) ;
#17224 = EDGE_LOOP ( 'NONE', ( #1347, #32037 ) ) ;
#17226 = AXIS2_PLACEMENT_3D ( 'NONE', #24307, #9695, #12673 ) ;
#17227 = DIRECTION ( 'NONE',  ( 1.000000000000000000, 0.000000000000000000, 0.000000000000000000 ) ) ;
#17228 = VECTOR ( 'NONE', #9058, 1000.000000000000000 ) ;
#17229 = CARTESIAN_POINT ( 'NONE',  ( -5.000000000000000888, -2.886751345948150860, -0.5999999999999998668 ) ) ;
#17230 = CARTESIAN_POINT ( 'NONE',  ( 107.1113102691238907, -50.40388046061509897, 32.50000000000000000 ) ) ;
#17231 = DIRECTION ( 'NONE',  ( 1.000000000000000000, 0.000000000000000000, 0.000000000000000000 ) ) ;
#17232 = CARTESIAN_POINT ( 'NONE',  ( 72.72667006429044534, -101.6652913307183610, 27.50000000000000000 ) ) ;
#17233 = CIRCLE ( 'NONE', #4062, 27.00000000000001421 ) ;
#17234 = FACE_OUTER_BOUND ( 'NONE', #24256, .T. ) ;
#17235 = ORIENTED_EDGE ( 'NONE', *, *, #6450, .T. ) ;
#17236 = AXIS2_PLACEMENT_3D ( 'NONE', #29080, #26291, #36356 ) ;
#17237 = EDGE_LOOP ( 'NONE', ( #3001, #26636, #26143, #35638 ) ) ;
#17238 = DIRECTION ( 'NONE',  ( 0.000000000000000000, 0.000000000000000000, 1.000000000000000000 ) ) ;
#17239 = EDGE_CURVE ( 'NONE', #6061, #28630, #24363, .T. ) ;
#17240 = CIRCLE ( 'NONE', #14816, 3.000000000000002665 ) ;
#17241 = DIRECTION ( 'NONE',  ( 0.000000000000000000, 0.000000000000000000, 1.000000000000000000 ) ) ;
#17242 = DIRECTION ( 'NONE',  ( 0.000000000000000000, 0.000000000000000000, -1.000000000000000000 ) ) ;
#17243 = DIRECTION ( 'NONE',  ( 1.000000000000000000, 0.000000000000000000, 0.000000000000000000 ) ) ;
#17244 = ORIENTED_EDGE ( 'NONE', *, *, #15929, .F. ) ;
#17245 = AXIS2_PLACEMENT_3D ( 'NONE', #10485, #19310, #33374 ) ;
#17246 = FACE_BOUND ( 'NONE', #33313, .T. ) ;
#17247 = ORIENTED_EDGE ( 'NONE', *, *, #7907, .F. ) ;
#17248 = ORIENTED_EDGE ( 'NONE', *, *, #17869, .T. ) ;
#17249 = EDGE_CURVE ( 'NONE', #16094, #15689, #10577, .T. ) ;
#17250 = DIRECTION ( 'NONE',  ( 0.000000000000000000, 0.000000000000000000, 1.000000000000000000 ) ) ;
#17251 = ORIENTED_EDGE ( 'NONE', *, *, #8934, .F. ) ;
#17252 = SURFACE_STYLE_USAGE ( .BOTH. , #13870 ) ;
#17253 = LINE ( 'NONE', #19326, #31958 ) ;
#17254 = VECTOR ( 'NONE', #35095, 1000.000000000000000 ) ;
#17255 = DIRECTION ( 'NONE',  ( 1.000000000000000000, 0.000000000000000000, 0.000000000000000000 ) ) ;
#17256 = VERTEX_POINT ( 'NONE', #3698 ) ;
#17257 = VERTEX_POINT ( 'NONE', #15125 ) ;
#17258 = AXIS2_PLACEMENT_3D ( 'NONE', #20925, #32353, #6669 ) ;
#17259 = AXIS2_PLACEMENT_3D ( 'NONE', #12189, #23659, #12587 ) ;
#17260 = ORIENTED_EDGE ( 'NONE', *, *, #21818, .F. ) ;
#17261 = VECTOR ( 'NONE', #29736, 1000.000000000000000 ) ;
#17262 = EDGE_CURVE ( 'NONE', #18637, #14854, #8201, .T. ) ;
#17263 = ORIENTED_EDGE ( 'NONE', *, *, #9736, .T. ) ;
#17264 = ORIENTED_EDGE ( 'NONE', *, *, #23944, .T. ) ;
#17265 = ADVANCED_FACE ( 'NONE', ( #5380 ), #24515, .F. ) ;
#17266 = DIRECTION ( 'NONE',  ( 0.000000000000000000, 0.000000000000000000, 1.000000000000000000 ) ) ;
#17267 = ADVANCED_FACE ( 'NONE', ( #16618 ), #36123, .F. ) ;
#17268 = B_SPLINE_CURVE_WITH_KNOTS ( 'NONE', 3,
 ( #36368, #35821, #7866, #21364, #27557, #24926, #13288, #10476, #26988, #9918, #1679, #12715, #18570, #24170 ),
 .UNSPECIFIED., .F., .F.,
 ( 4, 2, 2, 2, 2, 2, 4 ),
 ( 0.01481111731982464805, 0.01564725794959783214, 0.01648339857937101624, 0.01690146889425760829, 0.01731953920914420034, 0.01773760952403079239, 0.01815567983891738443 ),
 .UNSPECIFIED. ) ;
#17269 = CARTESIAN_POINT ( 'NONE',  ( 3.000000000000000000, -2.935248768560059229, 3.469446951953614189E-15 ) ) ;
#17270 = PLANE ( 'NONE',  #7940 ) ;
#17271 = DIRECTION ( 'NONE',  ( 0.000000000000000000, 0.000000000000000000, 1.000000000000000000 ) ) ;
#17272 = EDGE_LOOP ( 'NONE', ( #27034, #22411, #23313, #29879 ) ) ;
#17273 = CARTESIAN_POINT ( 'NONE',  ( 66.99999662536839651, -43.30127018922199511, -9.999999999999998224 ) ) ;
#17274 = CIRCLE ( 'NONE', #10689, 33.00000000000002132 ) ;
#17275 = CARTESIAN_POINT ( 'NONE',  ( 86.99999662536832545, 25.98076211353319565, -9.999999999999998224 ) ) ;
#17276 = DIRECTION ( 'NONE',  ( -0.000000000000000000, -0.000000000000000000, 1.000000000000000000 ) ) ;
#17277 = EDGE_LOOP ( 'NONE', ( #6340, #18400 ) ) ;
#17278 = LINE ( 'NONE', #20068, #26244 ) ;
#17279 = CARTESIAN_POINT ( 'NONE',  ( -32.00000337463118427, 69.28203230275516944, 17.49999999999999645 ) ) ;
#17280 = CIRCLE ( 'NONE', #33447, 2.000000000000000000 ) ;
#17281 = ORIENTED_EDGE ( 'NONE', *, *, #26970, .F. ) ;
#17282 = VERTEX_POINT ( 'NONE', #30502 ) ;
#17283 = DIRECTION ( 'NONE',  ( 1.000000000000000000, 0.000000000000000000, 0.000000000000000000 ) ) ;
#17284 = CIRCLE ( 'NONE', #32221, 2.000000000000001776 ) ;
#17285 = CARTESIAN_POINT ( 'NONE',  ( 69.99999662536838230, -51.96152422706639840, -9.999999999999998224 ) ) ;
#17286 = DIRECTION ( 'NONE',  ( 1.000000000000000000, 0.000000000000000000, 0.000000000000000000 ) ) ;
#17287 = DIRECTION ( 'NONE',  ( 0.000000000000000000, 0.000000000000000000, 1.000000000000000000 ) ) ;
#17288 = ORIENTED_EDGE ( 'NONE', *, *, #17534, .T. ) ;
#17289 = VERTEX_POINT ( 'NONE', #33112 ) ;
#17290 = CIRCLE ( 'NONE', #19091, 27.00000000000001066 ) ;
#17291 = ADVANCED_FACE ( 'NONE', ( #7626 ), #28234, .T. ) ;
#17292 = CARTESIAN_POINT ( 'NONE',  ( 108.3061974404897825, -19.22934205795014151, 32.50000000000000000 ) ) ;
#17293 = CARTESIAN_POINT ( 'NONE',  ( -47.00000337463112743, -60.62177826491080168, -9.999999999999998224 ) ) ;
#17294 = DIRECTION ( 'NONE',  ( 0.000000000000000000, 0.000000000000000000, 1.000000000000000000 ) ) ;
#17295 = CIRCLE ( 'NONE', #5922, 2.000000000000001776 ) ;
#17296 = ORIENTED_EDGE ( 'NONE', *, *, #17832, .F. ) ;
#17297 = CARTESIAN_POINT ( 'NONE',  ( -10.00000337463125000, -86.60254037844400443, 12.50000000000000000 ) ) ;
#17298 = ORIENTED_EDGE ( 'NONE', *, *, #5790, .F. ) ;
#17299 = CIRCLE ( 'NONE', #20875, 3.500000000000003109 ) ;
#17300 = ORIENTED_EDGE ( 'NONE', *, *, #25973, .F. ) ;
#17301 = CARTESIAN_POINT ( 'NONE',  ( 0.000000000000000000, 0.000000000000000000, -5.974599999999999689 ) ) ;
#17302 = DIRECTION ( 'NONE',  ( 0.000000000000000000, 0.000000000000000000, 1.000000000000000000 ) ) ;
#17303 = VERTEX_POINT ( 'NONE', #22414 ) ;
#17304 = EDGE_LOOP ( 'NONE', ( #14759, #11212 ) ) ;
#17305 = DIRECTION ( 'NONE',  ( 0.000000000000000000, 0.000000000000000000, 1.000000000000000000 ) ) ;
#17306 = PLANE ( 'NONE',  #25622 ) ;
#17307 = DIRECTION ( 'NONE',  ( 1.000000000000000000, 0.000000000000000000, 0.000000000000000000 ) ) ;
#17308 = ORIENTED_EDGE ( 'NONE', *, *, #33665, .F. ) ;
#17309 = FACE_OUTER_BOUND ( 'NONE', #25859, .T. ) ;
#17310 = AXIS2_PLACEMENT_3D ( 'NONE', #18728, #19461, #16460 ) ;
#17311 = ADVANCED_FACE ( 'NONE', ( #7433 ), #13811, .T. ) ;
#17312 = FACE_BOUND ( 'NONE', #35376, .T. ) ;
#17313 = CARTESIAN_POINT ( 'NONE',  ( -47.00000337463111322, 60.62177826491077326, -5.000000000000000000 ) ) ;
#17314 = CARTESIAN_POINT ( 'NONE',  ( 22.99999662536857059, 77.94228634059957983, 17.49999999999999645 ) ) ;
#17315 = DIRECTION ( 'NONE',  ( 0.000000000000000000, 0.000000000000000000, 1.000000000000000000 ) ) ;
#17316 = CARTESIAN_POINT ( 'NONE',  ( 44.99999662536849598, 60.62177826491077326, 12.50000000000000000 ) ) ;
#17317 = DIRECTION ( 'NONE',  ( 0.000000000000000000, 0.000000000000000000, 1.000000000000000000 ) ) ;
#17318 = AXIS2_PLACEMENT_3D ( 'NONE', #33280, #7596, #16231 ) ;
#17319 = LINE ( 'NONE', #14663, #35545 ) ;
#17320 = ORIENTED_EDGE ( 'NONE', *, *, #33462, .F. ) ;
#17321 = APPLICATION_CONTEXT ( 'automotive_design' ) ;
#17322 = LINE ( 'NONE', #5512, #16040 ) ;
#17323 = CARTESIAN_POINT ( 'NONE',  ( -3.060208875726633693, 4.280211771583961600, -4.057749648769094719 ) ) ;
#17324 = DIRECTION ( 'NONE',  ( 1.000000000000000000, 0.000000000000000000, 0.000000000000000000 ) ) ;
#17325 = VERTEX_POINT ( 'NONE', #21682 ) ;
#17326 = ORIENTED_EDGE ( 'NONE', *, *, #16519, .F. ) ;
#17327 = AXIS2_PLACEMENT_3D ( 'NONE', #3161, #34484, #20409 ) ;
#17328 = ORIENTED_EDGE ( 'NONE', *, *, #1879, .F. ) ;
#17329 = DIRECTION ( 'NONE',  ( -1.000000000000000000, 0.000000000000000000, 0.000000000000000000 ) ) ;
#17330 = CARTESIAN_POINT ( 'NONE',  ( -72.72667006429185221, -101.6652913307173662, 32.50000000000000000 ) ) ;
#17331 = CIRCLE ( 'NONE', #32904, 1.999999999999998224 ) ;
#17332 = CARTESIAN_POINT ( 'NONE',  ( -5.750000000000000000, 89.94802294027094547, 32.49999999999999289 ) ) ;
#17333 = ORIENTED_EDGE ( 'NONE', *, *, #21242, .F. ) ;
#17334 = EDGE_CURVE ( 'NONE', #3043, #33094, #27941, .T. ) ;
#17335 = DIRECTION ( 'NONE',  ( 0.000000000000000000, 0.000000000000000000, -1.000000000000000000 ) ) ;
#17336 = CIRCLE ( 'NONE', #2225, 2.000000000000001776 ) ;
#17337 = VECTOR ( 'NONE', #35003, 1000.000000000000000 ) ;
#17338 = ORIENTED_EDGE ( 'NONE', *, *, #2252, .F. ) ;
#17339 = DIRECTION ( 'NONE',  ( 0.000000000000000000, -1.000000000000000000, 0.000000000000000000 ) ) ;
#17340 = VERTEX_POINT ( 'NONE', #4634 ) ;
#17341 = CIRCLE ( 'NONE', #19721, 2.000000000000001776 ) ;
#17342 = CARTESIAN_POINT ( 'NONE',  ( 77.99999662536832545, -17.32050807568879591, 17.49999999999999645 ) ) ;
#17343 = VERTEX_POINT ( 'NONE', #25249 ) ;
#17344 = VERTEX_POINT ( 'NONE', #27500 ) ;
#17345 = EDGE_CURVE ( 'NONE', #20978, #21059, #29138, .T. ) ;
#17346 = LINE ( 'NONE', #14517, #5227 ) ;
#17347 = DIRECTION ( 'NONE',  ( 0.000000000000000000, 0.000000000000000000, 1.000000000000000000 ) ) ;
#17348 = CARTESIAN_POINT ( 'NONE',  ( 3.401922400366481192, 3.809401878282541176, -3.971474537231019397 ) ) ;
#17349 = ORIENTED_EDGE ( 'NONE', *, *, #25467, .T. ) ;
#17350 = DIRECTION ( 'NONE',  ( 0.000000000000000000, 0.000000000000000000, 1.000000000000000000 ) ) ;
#17351 = DIRECTION ( 'NONE',  ( 1.000000000000000000, 0.000000000000000000, 0.000000000000000000 ) ) ;
#17352 = CARTESIAN_POINT ( 'NONE',  ( 11.99999662536862566, 86.60254037844397601, -9.999999999999998224 ) ) ;
#17353 = AXIS2_PLACEMENT_3D ( 'NONE', #15295, #26928, #26545 ) ;
#17354 = ORIENTED_EDGE ( 'NONE', *, *, #26308, .F. ) ;
#17355 = CARTESIAN_POINT ( 'NONE',  ( 59.99999662536842493, 51.96152422706639129, -9.999999999999998224 ) ) ;
#17356 = DIRECTION ( 'NONE',  ( 1.000000000000000000, 0.000000000000000000, 0.000000000000000000 ) ) ;
#17357 = EDGE_LOOP ( 'NONE', ( #25144, #1020, #14923, #6757 ) ) ;
#17358 = EDGE_CURVE ( 'NONE', #12964, #21989, #12972, .T. ) ;
#17359 = FACE_OUTER_BOUND ( 'NONE', #35544, .T. ) ;
#17360 = FACE_OUTER_BOUND ( 'NONE', #9535, .T. ) ;
#17361 = AXIS2_PLACEMENT_3D ( 'NONE', #18034, #12756, #9772 ) ;
#17362 = DIRECTION ( 'NONE',  ( 0.000000000000000000, 0.000000000000000000, 1.000000000000000000 ) ) ;
#17363 = CARTESIAN_POINT ( 'NONE',  ( 6.249999999999998224, 0.000000000000000000, 0.000000000000000000 ) ) ;
#17364 = DIRECTION ( 'NONE',  ( 0.000000000000000000, 0.000000000000000000, 1.000000000000000000 ) ) ;
#17365 = ORIENTED_EDGE ( 'NONE', *, *, #31595, .F. ) ;
#17366 = AXIS2_PLACEMENT_3D ( 'NONE', #510, #26747, #1250 ) ;
#17367 = DIRECTION ( 'NONE',  ( -0.5000000000000051070, 1.060575238724903217E-16, -0.8660254037844355990 ) ) ;
#17368 = CARTESIAN_POINT ( 'NONE',  ( 64.99999662536839651, -43.30127018922199511, -5.000000000000000000 ) ) ;
#17370 = EDGE_CURVE ( 'NONE', #13211, #34185, #774, .T. ) ;
#17369 = ORIENTED_EDGE ( 'NONE', *, *, #137, .T. ) ;
#17371 = ORIENTED_EDGE ( 'NONE', *, *, #18867, .F. ) ;
#17372 = ORIENTED_EDGE ( 'NONE', *, *, #12494, .T. ) ;
#17373 = ADVANCED_FACE ( 'NONE', ( #33680 ), #2547, .F. ) ;
#17374 = FILL_AREA_STYLE_COLOUR ( '', #9218 ) ;
#17375 = CARTESIAN_POINT ( 'NONE',  ( -47.63139720814380951, 27.50000000000055422, -5.000000000000000888 ) ) ;
#17376 = DIRECTION ( 'NONE',  ( 0.000000000000000000, 0.000000000000000000, 1.000000000000000000 ) ) ;
#17377 = AXIS2_PLACEMENT_3D ( 'NONE', #21586, #33009, #28763 ) ;
#17378 = EDGE_CURVE ( 'NONE', #23671, #24284, #19075, .T. ) ;
#17379 = DIRECTION ( 'NONE',  ( -1.000000000000000000, 0.000000000000000000, 0.000000000000000000 ) ) ;
#17380 = ORIENTED_EDGE ( 'NONE', *, *, #29349, .F. ) ;
#17381 = LINE ( 'NONE', #3126, #31100 ) ;
#17382 = EDGE_CURVE ( 'NONE', #36317, #1952, #10624, .T. ) ;
#17383 = ORIENTED_EDGE ( 'NONE', *, *, #24523, .T. ) ;
#17385 = AXIS2_PLACEMENT_3D ( 'NONE', #8622, #20255, #22709 ) ;
#17384 = FACE_BOUND ( 'NONE', #3376, .T. ) ;
#17386 = EDGE_CURVE ( 'NONE', #17794, #12035, #23748, .T. ) ;
#17387 = DIRECTION ( 'NONE',  ( 1.000000000000000000, 0.000000000000000000, 0.000000000000000000 ) ) ;
#17388 = VECTOR ( 'NONE', #2001, 1000.000000000000000 ) ;
#17389 = CYLINDRICAL_SURFACE ( 'NONE', #3529, 2.000000000000001776 ) ;
#17390 = DIRECTION ( 'NONE',  ( -1.000000000000000000, 0.000000000000000000, 0.000000000000000000 ) ) ;
#17391 = CARTESIAN_POINT ( 'NONE',  ( -37.49999999999998579, 103.4105893997321601, -26.00000000000000000 ) ) ;
#17392 = CARTESIAN_POINT ( 'NONE',  ( -65.00000337463102085, 25.98076211353317433, -9.999999999999998224 ) ) ;
#17393 = CARTESIAN_POINT ( 'NONE',  ( 48.49678893472093932, 67.96280274017779277, 12.50000000000000000 ) ) ;
#17394 = CARTESIAN_POINT ( 'NONE',  ( -35.00000337463116296, 77.94228634059957983, 17.49999999999999645 ) ) ;
#17395 = ORIENTED_EDGE ( 'NONE', *, *, #21162, .T. ) ;
#17396 = AXIS2_PLACEMENT_3D ( 'NONE', #28751, #3076, #14497 ) ;
#17397 = DIRECTION ( 'NONE',  ( 1.000000000000000000, 0.000000000000000000, 0.000000000000000000 ) ) ;
#17398 = DIRECTION ( 'NONE',  ( -0.000000000000000000, -0.8660254037844414832, -0.4999999999999953371 ) ) ;
#17399 = DIRECTION ( 'NONE',  ( 0.000000000000000000, 0.000000000000000000, -1.000000000000000000 ) ) ;
#17400 = EDGE_LOOP ( 'NONE', ( #23498, #987 ) ) ;
#17401 = EDGE_CURVE ( 'NONE', #8449, #30786, #6985, .T. ) ;
#17402 = ORIENTED_EDGE ( 'NONE', *, *, #31222, .F. ) ;
#17403 = AXIS2_PLACEMENT_3D ( 'NONE', #26660, #18786, #7531 ) ;
#17404 = B_SPLINE_CURVE_WITH_KNOTS ( 'NONE', 3,
 ( #26893, #22006, #33064, #30791, #24458, #7765 ),
 .UNSPECIFIED., .F., .F.,
 ( 4, 2, 4 ),
 ( 0.003058795990767257302, 0.004586520967003302265, 0.006114245943239346795 ),
 .UNSPECIFIED. ) ;
#17405 = ORIENTED_EDGE ( 'NONE', *, *, #26768, .F. ) ;
#17406 = ADVANCED_FACE ( 'NONE', ( #25077 ), #19255, .F. ) ;
#17407 = PLANE ( 'NONE',  #2471 ) ;
#17408 = EDGE_CURVE ( 'NONE', #14195, #34040, #31397, .T. ) ;
#17409 = DIRECTION ( 'NONE',  ( -1.000000000000000000, -0.000000000000000000, -0.000000000000000000 ) ) ;
#17410 = DIRECTION ( 'NONE',  ( 1.000000000000000000, 0.000000000000000000, 0.000000000000000000 ) ) ;
#17411 = DIRECTION ( 'NONE',  ( 3.469446951953612611E-15, 1.000000000000000000, 0.000000000000000000 ) ) ;
#17412 = CARTESIAN_POINT ( 'NONE',  ( 64.99999662536841072, -25.98076211353320275, -9.999999999999998224 ) ) ;
#17413 = ORIENTED_EDGE ( 'NONE', *, *, #18943, .F. ) ;
#17414 = ORIENTED_EDGE ( 'NONE', *, *, #33140, .T. ) ;
#17415 = DIRECTION ( 'NONE',  ( 0.000000000000000000, 0.000000000000000000, 1.000000000000000000 ) ) ;
#17416 = CARTESIAN_POINT ( 'NONE',  ( 76.99999662536836809, 8.660254037844394404, -9.999999999999998224 ) ) ;
#17417 = DIRECTION ( 'NONE',  ( -1.000000000000000000, 0.000000000000000000, 0.000000000000000000 ) ) ;
#17418 = ORIENTED_EDGE ( 'NONE', *, *, #26552, .T. ) ;
#17419 = ADVANCED_FACE ( 'NONE', ( #6272 ), #100, .F. ) ;
#17420 = FACE_BOUND ( 'NONE', #8993, .T. ) ;
#17421 = EDGE_LOOP ( 'NONE', ( #1624, #32103, #17900, #11697 ) ) ;
#17422 = ORIENTED_EDGE ( 'NONE', *, *, #24954, .F. ) ;
#17423 = AXIS2_PLACEMENT_3D ( 'NONE', #19475, #25470, #10299 ) ;
#17424 = DIRECTION ( 'NONE',  ( 0.000000000000000000, 0.000000000000000000, 1.000000000000000000 ) ) ;
#17425 = ORIENTED_EDGE ( 'NONE', *, *, #13246, .T. ) ;
#17426 = DIRECTION ( 'NONE',  ( 1.000000000000000000, 0.000000000000000000, 0.000000000000000000 ) ) ;
#17427 = CARTESIAN_POINT ( 'NONE',  ( -10.00000337463127842, -69.28203230275519786, 12.50000000000000000 ) ) ;
#17428 = EDGE_LOOP ( 'NONE', ( #26243, #32468 ) ) ;
#17429 = ORIENTED_EDGE ( 'NONE', *, *, #23389, .T. ) ;
#17430 = EDGE_LOOP ( 'NONE', ( #34012, #15658 ) ) ;
#17431 = ORIENTED_EDGE ( 'NONE', *, *, #27292, .T. ) ;
#17432 = ADVANCED_FACE ( 'NONE', ( #8374 ), #3276, .T. ) ;
#17433 = ORIENTED_EDGE ( 'NONE', *, *, #34840, .T. ) ;
#17434 = DIRECTION ( 'NONE',  ( 1.000000000000000000, 0.000000000000000000, 0.000000000000000000 ) ) ;
#17435 = ADVANCED_FACE ( 'NONE', ( #25418 ), #19976, .T. ) ;
#17436 = VECTOR ( 'NONE', #2248, 1000.000000000000000 ) ;
#17437 = CARTESIAN_POINT ( 'NONE',  ( 49.99999662536848177, -51.96152422706640550, 17.49999999999999645 ) ) ;
#17438 = DIRECTION ( 'NONE',  ( 0.000000000000000000, 0.000000000000000000, 1.000000000000000000 ) ) ;
#17439 = CARTESIAN_POINT ( 'NONE',  ( 0.000000000000000000, 0.000000000000000000, 32.50000000000000000 ) ) ;
#17440 = ORIENTED_EDGE ( 'NONE', *, *, #17249, .F. ) ;
#17441 = CARTESIAN_POINT ( 'NONE',  ( 9.999996625368625658, 86.60254037844397601, -9.999999999999998224 ) ) ;
#17442 = EDGE_CURVE ( 'NONE', #24345, #12378, #17763, .T. ) ;
#17443 = CYLINDRICAL_SURFACE ( 'NONE', #4220, 65.00000000000000000 ) ;
#17444 = CARTESIAN_POINT ( 'NONE',  ( 82.99999662536832545, 25.98076211353319565, 12.50000000000000000 ) ) ;
#17445 = ORIENTED_EDGE ( 'NONE', *, *, #23159, .T. ) ;
#17446 = DIRECTION ( 'NONE',  ( 1.000000000000000000, 0.000000000000000000, 0.000000000000000000 ) ) ;
#17447 = EDGE_CURVE ( 'NONE', #17289, #23885, #14532, .T. ) ;
#17448 = FACE_OUTER_BOUND ( 'NONE', #32414, .T. ) ;
#17449 = ADVANCED_FACE ( 'NONE', ( #22611 ), #19807, .F. ) ;
#17450 = EDGE_LOOP ( 'NONE', ( #4260, #22179, #5823, #5842 ) ) ;
#17451 = ORIENTED_EDGE ( 'NONE', *, *, #20538, .T. ) ;
#17452 = CARTESIAN_POINT ( 'NONE',  ( 0.000000000000000000, 81.28776890242660613, -29.99999999999987566 ) ) ;
#17453 = DIRECTION ( 'NONE',  ( 0.000000000000000000, 0.000000000000000000, -1.000000000000000000 ) ) ;
#17454 = CARTESIAN_POINT ( 'NONE',  ( 34.99999662536855283, -77.94228634059960825, -9.999999999999998224 ) ) ;
#17455 = CARTESIAN_POINT ( 'NONE',  ( -2.775557561562891351E-14, 19.94802294027085310, 27.49999999999999645 ) ) ;
#17456 = ORIENTED_EDGE ( 'NONE', *, *, #12812, .F. ) ;
#17457 = EDGE_CURVE ( 'NONE', #29052, #5247, #12369, .T. ) ;
#17458 = DIRECTION ( 'NONE',  ( -0.000000000000000000, -0.000000000000000000, 1.000000000000000000 ) ) ;
#17459 = CARTESIAN_POINT ( 'NONE',  ( 52.99999662536846046, -43.30127018922200222, 12.50000000000000000 ) ) ;
#17460 = ADVANCED_FACE ( 'NONE', ( #272 ), #8545, .F. ) ;
#17461 = CYLINDRICAL_SURFACE ( 'NONE', #36883, 30.00000000000000000 ) ;
#17462 = ADVANCED_FACE ( 'NONE', ( #25806 ), #28402, .F. ) ;
#17463 = VERTEX_POINT ( 'NONE', #14713 ) ;
#17464 = VECTOR ( 'NONE', #23906, 1000.000000000000000 ) ;
#17465 = EDGE_CURVE ( 'NONE', #27468, #27651, #14795, .T. ) ;
#17466 = AXIS2_PLACEMENT_3D ( 'NONE', #26270, #1315, #3939 ) ;
#17467 = DIRECTION ( 'NONE',  ( 1.000000000000000000, -3.846960960290410782E-15, 0.000000000000000000 ) ) ;
#17468 = ORIENTED_EDGE ( 'NONE', *, *, #36399, .F. ) ;
#17469 = CARTESIAN_POINT ( 'NONE',  ( 0.000000000000000000, 0.000000000000000000, 15.00000000000000000 ) ) ;
#17470 = CYLINDRICAL_SURFACE ( 'NONE', #33189, 2.000000000000001776 ) ;
#17471 = DIRECTION ( 'NONE',  ( 0.000000000000000000, -0.000000000000000000, -1.000000000000000000 ) ) ;
#17472 = ORIENTED_EDGE ( 'NONE', *, *, #11911, .F. ) ;
#17473 = ORIENTED_EDGE ( 'NONE', *, *, #37031, .F. ) ;
#17474 = DIRECTION ( 'NONE',  ( 0.000000000000000000, 0.000000000000000000, 1.000000000000000000 ) ) ;
#17475 = DIRECTION ( 'NONE',  ( -1.000000000000000000, 0.000000000000000000, 0.000000000000000000 ) ) ;
#17476 = CARTESIAN_POINT ( 'NONE',  ( -20.00000337463123756, -86.60254037844400443, -5.000000000000000000 ) ) ;
#17477 = ORIENTED_EDGE ( 'NONE', *, *, #21775, .F. ) ;
#17478 = DIRECTION ( 'NONE',  ( 1.000000000000000000, 0.000000000000000000, 0.000000000000000000 ) ) ;
#17479 = FACE_BOUND ( 'NONE', #18442, .T. ) ;
#17480 = DIRECTION ( 'NONE',  ( -0.4999999999999980016, 0.8660254037844398178, 0.000000000000000000 ) ) ;
#17481 = DIRECTION ( 'NONE',  ( -1.000000000000000000, 0.000000000000000000, 0.000000000000000000 ) ) ;
#17482 = CARTESIAN_POINT ( 'NONE',  ( -10.00000337463125000, -86.60254037844400443, -5.000000000000000000 ) ) ;
#17483 = CARTESIAN_POINT ( 'NONE',  ( 72.99999662536835388, -43.30127018922199511, -9.999999999999998224 ) ) ;
#17484 = AXIS2_PLACEMENT_3D ( 'NONE', #3425, #3776, #15604 ) ;
#17485 = DIRECTION ( 'NONE',  ( -1.000000000000000000, 0.000000000000000000, 0.000000000000000000 ) ) ;
#17486 = ORIENTED_EDGE ( 'NONE', *, *, #29385, .F. ) ;
#17487 = DIRECTION ( 'NONE',  ( -0.000000000000000000, -0.000000000000000000, -1.000000000000000000 ) ) ;
#17488 = DIRECTION ( 'NONE',  ( 0.000000000000000000, 0.000000000000000000, 1.000000000000000000 ) ) ;
#17489 = FACE_OUTER_BOUND ( 'NONE', #33076, .T. ) ;
#17490 = ORIENTED_EDGE ( 'NONE', *, *, #30434, .F. ) ;
#17491 = ORIENTED_EDGE ( 'NONE', *, *, #14831, .F. ) ;
#17492 = ORIENTED_EDGE ( 'NONE', *, *, #23035, .F. ) ;
#17493 = CARTESIAN_POINT ( 'NONE',  ( -53.00000337463109190, -60.62177826491083010, 12.50000000000000000 ) ) ;
#17494 = DIRECTION ( 'NONE',  ( 1.000000000000000000, 0.000000000000000000, 0.000000000000000000 ) ) ;
#17495 = DIRECTION ( 'NONE',  ( 0.000000000000000000, 0.000000000000000000, 1.000000000000000000 ) ) ;
#17496 = ORIENTED_EDGE ( 'NONE', *, *, #34112, .T. ) ;
#17497 = B_SPLINE_CURVE_WITH_KNOTS ( 'NONE', 3,
 ( #33648, #19385, #30804, #10581, #28014, #4401 ),
 .UNSPECIFIED., .F., .F.,
 ( 4, 2, 4 ),
 ( 0.005150343764683549923, 0.006610526168996381374, 0.008070708573309213693 ),
 .UNSPECIFIED. ) ;
#17498 = AXIS2_PLACEMENT_3D ( 'NONE', #4719, #10706, #27185 ) ;
#17499 = FACE_OUTER_BOUND ( 'NONE', #30611, .T. ) ;
#17500 = AXIS2_PLACEMENT_3D ( 'NONE', #2093, #16540, #30970 ) ;
#17501 = EDGE_LOOP ( 'NONE', ( #25775, #12898, #11874, #14367 ) ) ;
#17502 = EDGE_CURVE ( 'NONE', #10128, #36402, #25600, .T. ) ;
#17503 = DIRECTION ( 'NONE',  ( 0.000000000000000000, 0.000000000000000000, 1.000000000000000000 ) ) ;
#17504 = ORIENTED_EDGE ( 'NONE', *, *, #25263, .T. ) ;
#17505 = CARTESIAN_POINT ( 'NONE',  ( 56.67878100130369035, -27.78182860042797131, -4.999999999999997335 ) ) ;
#17506 = ORIENTED_EDGE ( 'NONE', *, *, #9640, .F. ) ;
#17507 = EDGE_LOOP ( 'NONE', ( #17689, #10955, #20798, #14140 ) ) ;
#17508 = FACE_OUTER_BOUND ( 'NONE', #34806, .T. ) ;
#17509 = LINE ( 'NONE', #26333, #25020 ) ;
#17510 = AXIS2_PLACEMENT_3D ( 'NONE', #12149, #15004, #14810 ) ;
#17511 = CARTESIAN_POINT ( 'NONE',  ( -72.72667006429185221, -101.6652913307173662, 32.50002500000000083 ) ) ;
#17512 = ADVANCED_BREP_SHAPE_REPRESENTATION ( '', ( #6859, #21385 ), #2251 ) ;
#17513 = ORIENTED_EDGE ( 'NONE', *, *, #22726, .F. ) ;
#17514 = LINE ( 'NONE', #3815, #25090 ) ;
#17515 = FACE_OUTER_BOUND ( 'NONE', #16021, .T. ) ;
#17516 = DIRECTION ( 'NONE',  ( -0.4999999999999980016, 0.8660254037844398178, 0.000000000000000000 ) ) ;
#17517 = ORIENTED_EDGE ( 'NONE', *, *, #15397, .T. ) ;
#17518 = CYLINDRICAL_SURFACE ( 'NONE', #5776, 1.999999999999998224 ) ;
#17519 = CARTESIAN_POINT ( 'NONE',  ( -50.00000337463110611, -69.28203230275519786, 12.50000000000000000 ) ) ;
#17520 = ORIENTED_EDGE ( 'NONE', *, *, #27375, .F. ) ;
#17521 = DIRECTION ( 'NONE',  ( 0.000000000000000000, 0.000000000000000000, 1.000000000000000000 ) ) ;
#17522 = DIRECTION ( 'NONE',  ( -1.000000000000000000, 0.000000000000000000, 0.000000000000000000 ) ) ;
#17523 = DIRECTION ( 'NONE',  ( 1.000000000000000000, 0.000000000000000000, 0.000000000000000000 ) ) ;
#17524 = ADVANCED_FACE ( 'NONE', ( #11897 ), #29147, .F. ) ;
#17525 = EDGE_CURVE ( 'NONE', #19938, #18000, #35212, .T. ) ;
#17526 = CARTESIAN_POINT ( 'NONE',  ( 0.000000000000000000, 0.000000000000000000, 2.266666666666999674 ) ) ;
#17527 = AXIS2_PLACEMENT_3D ( 'NONE', #19490, #27922, #10866 ) ;
#17528 = CARTESIAN_POINT ( 'NONE',  ( -42.00000337463114164, 69.28203230275516944, -5.000000000000000000 ) ) ;
#17529 = VERTEX_POINT ( 'NONE', #36854 ) ;
#17530 = CYLINDRICAL_SURFACE ( 'NONE', #12962, 3.500000000000003109 ) ;
#17531 = DIRECTION ( 'NONE',  ( 1.000000000000000000, 0.000000000000000000, 0.000000000000000000 ) ) ;
#17532 = DIRECTION ( 'NONE',  ( -0.4999999999999979461, 0.8660254037844397068, 0.000000000000000000 ) ) ;
#17533 = EDGE_LOOP ( 'NONE', ( #21172, #27400 ) ) ;
#17534 = EDGE_CURVE ( 'NONE', #10828, #18808, #2726, .T. ) ;
#17536 = VERTEX_POINT ( 'NONE', #35167 ) ;
#17535 = EDGE_CURVE ( 'NONE', #33756, #32159, #9421, .T. ) ;
#17537 = ORIENTED_EDGE ( 'NONE', *, *, #21226, .T. ) ;
#17538 = CIRCLE ( 'NONE', #6748, 3.000000000000002665 ) ;
#17539 = CARTESIAN_POINT ( 'NONE',  ( 72.99999662536836809, 25.98076211353319565, -9.999999999999998224 ) ) ;
#17540 = FACE_OUTER_BOUND ( 'NONE', #32973, .T. ) ;
#17541 = DIRECTION ( 'NONE',  ( 1.000000000000000000, 0.000000000000000000, 0.000000000000000000 ) ) ;
#17542 = CARTESIAN_POINT ( 'NONE',  ( -70.00000337463099243, 51.96152422706637708, -9.999999999999998224 ) ) ;
#17543 = EDGE_LOOP ( 'NONE', ( #8256, #14812 ) ) ;
#17544 = ADVANCED_FACE ( 'NONE', ( #12449 ), #1216, .F. ) ;
#17545 = CARTESIAN_POINT ( 'NONE',  ( -83.00000337463092137, 8.660254037844389075, -9.999999999999998224 ) ) ;
#17546 = VERTEX_POINT ( 'NONE', #6476 ) ;
#17547 = FACE_BOUND ( 'NONE', #23298, .T. ) ;
#17548 = AXIS2_PLACEMENT_3D ( 'NONE', #28923, #20320, #31555 ) ;
#17549 = CIRCLE ( 'NONE', #33736, 2.000000000000001776 ) ;
#17550 = DIRECTION ( 'NONE',  ( 0.000000000000000000, 0.000000000000000000, 1.000000000000000000 ) ) ;
#17551 = DIRECTION ( 'NONE',  ( 1.000000000000000000, 0.000000000000000000, 0.000000000000000000 ) ) ;
#17552 = CARTESIAN_POINT ( 'NONE',  ( 54.99999662536846046, -43.30127018922200222, -9.999999999999998224 ) ) ;
#17553 = PRODUCT_CONTEXT ( 'NONE', #5099, 'mechanical' ) ;
#17554 = DIRECTION ( 'NONE',  ( 1.000000000000000000, 0.000000000000000000, 0.000000000000000000 ) ) ;
#17555 = CIRCLE ( 'NONE', #12755, 20.00000000000001066 ) ;
#17556 = DIRECTION ( 'NONE',  ( 0.000000000000000000, 0.000000000000000000, 1.000000000000000000 ) ) ;
#17557 = CARTESIAN_POINT ( 'NONE',  ( -73.00000337463097821, 8.660254037844374864, -9.999999999999998224 ) ) ;
#17558 = EDGE_CURVE ( 'NONE', #26515, #8511, #28552, .T. ) ;
#17559 = EDGE_LOOP ( 'NONE', ( #10095, #5848 ) ) ;
#17560 = DIRECTION ( 'NONE',  ( 0.000000000000000000, 0.000000000000000000, 1.000000000000000000 ) ) ;
#17561 = DIRECTION ( 'NONE',  ( 0.000000000000000000, 0.000000000000000000, 1.000000000000000000 ) ) ;
#17562 = LINE ( 'NONE', #516, #28493 ) ;
#17563 = VERTEX_POINT ( 'NONE', #32695 ) ;
#17564 = ORIENTED_EDGE ( 'NONE', *, *, #13088, .F. ) ;
#17565 = ORIENTED_EDGE ( 'NONE', *, *, #261, .F. ) ;
#17566 = ADVANCED_FACE ( 'NONE', ( #26518 ), #21460, .F. ) ;
#17567 = AXIS2_PLACEMENT_3D ( 'NONE', #22176, #7541, #1535 ) ;
#17568 = DIRECTION ( 'NONE',  ( 0.000000000000000000, 0.000000000000000000, 1.000000000000000000 ) ) ;
#17569 = VECTOR ( 'NONE', #31812, 1000.000000000000000 ) ;
#17570 = CARTESIAN_POINT ( 'NONE',  ( -65.00000337463106348, -60.62177826491083010, -5.000000000000000000 ) ) ;
#17571 = ADVANCED_FACE ( 'NONE', ( #27074 ), #23915, .F. ) ;
#17572 = ORIENTED_EDGE ( 'NONE', *, *, #10739, .T. ) ;
#17573 = CARTESIAN_POINT ( 'NONE',  ( -90.00000337463090716, -1.040834085586084257E-14, -9.999999999999998224 ) ) ;
#17574 = FACE_OUTER_BOUND ( 'NONE', #9637, .T. ) ;
#17575 = CARTESIAN_POINT ( 'NONE',  ( 7.999996625368625658, 86.60254037844397601, -9.999999999999998224 ) ) ;
#17576 = CYLINDRICAL_SURFACE ( 'NONE', #26961, 2.000000000000000000 ) ;
#17577 = ORIENTED_EDGE ( 'NONE', *, *, #14247, .F. ) ;
#17578 = CIRCLE ( 'NONE', #16393, 1.999999999999998224 ) ;
#17579 = ORIENTED_EDGE ( 'NONE', *, *, #26581, .T. ) ;
#17580 = DIRECTION ( 'NONE',  ( -1.000000000000000000, -0.000000000000000000, -0.000000000000000000 ) ) ;
#17581 = AXIS2_PLACEMENT_3D ( 'NONE', #19528, #36047, #22164 ) ;
#17582 = CARTESIAN_POINT ( 'NONE',  ( -63.00000337463104927, -43.30127018922202353, -9.999999999999998224 ) ) ;
#17583 = CARTESIAN_POINT ( 'NONE',  ( 26.99999662536856704, 77.94228634059957983, -9.999999999999998224 ) ) ;
#17584 = ORIENTED_EDGE ( 'NONE', *, *, #33196, .T. ) ;
#17585 = EDGE_CURVE ( 'NONE', #17896, #8583, #11210, .T. ) ;
#17586 = FACE_BOUND ( 'NONE', #5810, .T. ) ;
#17587 = ORIENTED_EDGE ( 'NONE', *, *, #24600, .F. ) ;
#17588 = ORIENTED_EDGE ( 'NONE', *, *, #32975, .T. ) ;
#17589 = DIRECTION ( 'NONE',  ( 1.000000000000000000, 0.000000000000000000, 0.000000000000000000 ) ) ;
#17590 = VERTEX_POINT ( 'NONE', #17907 ) ;
#17591 = ADVANCED_FACE ( 'NONE', ( #20909 ), #12637, .F. ) ;
#17592 = AXIS2_PLACEMENT_3D ( 'NONE', #6668, #15667, #5096 ) ;
#17593 = DIRECTION ( 'NONE',  ( -1.000000000000000000, 0.000000000000000000, 0.000000000000000000 ) ) ;
#17594 = CARTESIAN_POINT ( 'NONE',  ( 19.99999662536861678, -86.60254037844400443, -9.999999999999998224 ) ) ;
#17595 = ADVANCED_FACE ( 'NONE', ( #4024 ), #12805, .T. ) ;
#17596 = ORIENTED_EDGE ( 'NONE', *, *, #26073, .F. ) ;
#17597 = ORIENTED_EDGE ( 'NONE', *, *, #12086, .T. ) ;
#17598 = ORIENTED_EDGE ( 'NONE', *, *, #32963, .F. ) ;
#17599 = AXIS2_PLACEMENT_3D ( 'NONE', #15203, #21021, #18197 ) ;
#17600 = ORIENTED_EDGE ( 'NONE', *, *, #26073, .T. ) ;
#17601 = ORIENTED_EDGE ( 'NONE', *, *, #10835, .T. ) ;
#17602 = CARTESIAN_POINT ( 'NONE',  ( 67.99999662536839651, 51.96152422706640550, -9.999999999999998224 ) ) ;
#17603 = CIRCLE ( 'NONE', #24201, 3.000000000000000000 ) ;
#17604 = ORIENTED_EDGE ( 'NONE', *, *, #35294, .T. ) ;
#17605 = FACE_OUTER_BOUND ( 'NONE', #27788, .T. ) ;
#17606 = CARTESIAN_POINT ( 'NONE',  ( 90.51346025932915040, 71.13874598957531248, 32.50000000000000711 ) ) ;
#17607 = FACE_OUTER_BOUND ( 'NONE', #24236, .T. ) ;
#17608 = VERTEX_POINT ( 'NONE', #32897 ) ;
#17609 = CARTESIAN_POINT ( 'NONE',  ( 86.99999662536832545, 25.98076211353319565, -5.000000000000000000 ) ) ;
#17610 = CARTESIAN_POINT ( 'NONE',  ( -4.379424050594066919, -3.527728022193163504, -4.190801088233101268 ) ) ;
#17611 = EDGE_CURVE ( 'NONE', #5777, #28672, #417, .T. ) ;
#17612 = DIRECTION ( 'NONE',  ( 1.000000000000000000, 0.000000000000000000, 0.000000000000000000 ) ) ;
#17613 = ORIENTED_EDGE ( 'NONE', *, *, #13781, .F. ) ;
#17614 = FACE_OUTER_BOUND ( 'NONE', #23211, .T. ) ;
#17615 = CIRCLE ( 'NONE', #22418, 3.499999999999996003 ) ;
#17616 = CARTESIAN_POINT ( 'NONE',  ( -40.98360655737705827, 111.1639425680974398, -19.99999999999999645 ) ) ;
#17617 = VERTEX_POINT ( 'NONE', #18083 ) ;
#17618 = VECTOR ( 'NONE', #7316, 1000.000000000000000 ) ;
#17619 = ORIENTED_EDGE ( 'NONE', *, *, #28372, .F. ) ;
#17620 = DIRECTION ( 'NONE',  ( 0.000000000000000000, 0.000000000000000000, 1.000000000000000000 ) ) ;
#17621 = DIRECTION ( 'NONE',  ( 1.000000000000000000, 0.000000000000000000, 0.000000000000000000 ) ) ;
#17622 = CARTESIAN_POINT ( 'NONE',  ( 79.99999662536832545, -34.64101615137759183, -5.000000000000000000 ) ) ;
#17623 = FACE_OUTER_BOUND ( 'NONE', #30735, .T. ) ;
#17624 = VERTEX_POINT ( 'NONE', #7024 ) ;
#17625 = AXIS2_PLACEMENT_3D ( 'NONE', #26237, #17789, #29224 ) ;
#17626 = DIRECTION ( 'NONE',  ( 0.000000000000000000, 0.000000000000000000, 1.000000000000000000 ) ) ;
#17627 = FACE_BOUND ( 'NONE', #31087, .T. ) ;
#17628 = CIRCLE ( 'NONE', #24855, 27.00000000000001066 ) ;
#17629 = CARTESIAN_POINT ( 'NONE',  ( -85.00000337463092137, -8.660254037844422825, -9.999999999999998224 ) ) ;
#17630 = EDGE_CURVE ( 'NONE', #20697, #25448, #35160, .T. ) ;
#17631 = AXIS2_PLACEMENT_3D ( 'NONE', #22234, #4980, #36668 ) ;
#17632 = ORIENTED_EDGE ( 'NONE', *, *, #16716, .F. ) ;
#17633 = EDGE_CURVE ( 'NONE', #8115, #8678, #29168, .T. ) ;
#17634 = DIRECTION ( 'NONE',  ( 0.000000000000000000, 0.000000000000000000, -1.000000000000000000 ) ) ;
#17635 = ORIENTED_EDGE ( 'NONE', *, *, #9928, .T. ) ;
#17636 = CARTESIAN_POINT ( 'NONE',  ( -80.00000337463096400, -34.64101615137762025, -9.999999999999998224 ) ) ;
#17637 = EDGE_CURVE ( 'NONE', #25578, #6350, #13002, .T. ) ;
#17638 = CARTESIAN_POINT ( 'NONE',  ( -51.67317684408315870, -68.18636331025710717, -5.000000000000000000 ) ) ;
#17639 = VECTOR ( 'NONE', #21730, 1000.000000000000000 ) ;
#17640 = CARTESIAN_POINT ( 'NONE',  ( 17.55872235085560007, 89.94802294027088863, 30.49999999999999289 ) ) ;
#17641 = ORIENTED_EDGE ( 'NONE', *, *, #12109, .F. ) ;
#17642 = AXIS2_PLACEMENT_3D ( 'NONE', #15090, #26519, #9476 ) ;
#17643 = ORIENTED_EDGE ( 'NONE', *, *, #32436, .T. ) ;
#17644 = EDGE_CURVE ( 'NONE', #14287, #22341, #3478, .T. ) ;
#17645 = DIRECTION ( 'NONE',  ( 0.000000000000000000, 0.000000000000000000, -1.000000000000000000 ) ) ;
#17646 = EDGE_CURVE ( 'NONE', #10475, #2491, #33982, .T. ) ;
#17647 = CARTESIAN_POINT ( 'NONE',  ( -65.00000337463106348, -60.62177826491083010, -9.999999999999998224 ) ) ;
#17648 = CARTESIAN_POINT ( 'NONE',  ( -20.00000000000001066, 89.94802294027088863, -19.99999999999999645 ) ) ;
#17649 = CIRCLE ( 'NONE', #2671, 27.00000000000001421 ) ;
#17650 = ORIENTED_EDGE ( 'NONE', *, *, #25742, .T. ) ;
#17651 = CYLINDRICAL_SURFACE ( 'NONE', #15975, 2.000000000000001776 ) ;
#17652 = FACE_BOUND ( 'NONE', #30195, .T. ) ;
#17653 = CARTESIAN_POINT ( 'NONE',  ( 37.50000000000000000, 103.4105893997321743, 32.50000000000000000 ) ) ;
#17654 = DIRECTION ( 'NONE',  ( 1.000000000000000000, 0.000000000000000000, 0.000000000000000000 ) ) ;
#17655 = CARTESIAN_POINT ( 'NONE',  ( 37.50000000000000000, 103.4105893997321743, 27.50000000000000000 ) ) ;
#17656 = EDGE_CURVE ( 'NONE', #15620, #2172, #8802, .T. ) ;
#17657 = DIRECTION ( 'NONE',  ( 1.000000000000000000, 0.000000000000000000, 0.000000000000000000 ) ) ;
#17658 = CIRCLE ( 'NONE', #32006, 2.000000000000000000 ) ;
#17659 = ADVANCED_FACE ( 'NONE', ( #12241 ), #3826, .F. ) ;
#17660 = FACE_OUTER_BOUND ( 'NONE', #33809, .T. ) ;
#17661 = ADVANCED_FACE ( 'NONE', ( #10932 ), #21813, .F. ) ;
#17662 = EDGE_CURVE ( 'NONE', #15434, #14832, #30452, .T. ) ;
#17663 = CARTESIAN_POINT ( 'NONE',  ( -65.00000337463106348, -60.62177826491083010, 17.49999999999999645 ) ) ;
#17664 = ORIENTED_EDGE ( 'NONE', *, *, #6151, .F. ) ;
#17665 = EDGE_CURVE ( 'NONE', #34583, #3159, #36262, .T. ) ;
#17666 = CARTESIAN_POINT ( 'NONE',  ( 145.0000000000000853, 5.999999999999493738, 32.55002500000000509 ) ) ;
#17667 = CARTESIAN_POINT ( 'NONE',  ( -42.97377950131527058, 96.90768712682508124, 27.49999999999999645 ) ) ;
#17668 = DIRECTION ( 'NONE',  ( 1.000000000000000000, 0.000000000000000000, 0.000000000000000000 ) ) ;
#17669 = ORIENTED_EDGE ( 'NONE', *, *, #17386, .F. ) ;
#17670 = ORIENTED_EDGE ( 'NONE', *, *, #23863, .T. ) ;
#17671 = ORIENTED_EDGE ( 'NONE', *, *, #19293, .T. ) ;
#17672 = CIRCLE ( 'NONE', #16476, 3.000000000000000000 ) ;
#17673 = CARTESIAN_POINT ( 'NONE',  ( -70.00000337463100664, -17.32050807568882078, 12.50000000000000000 ) ) ;
#17674 = DIRECTION ( 'NONE',  ( 1.000000000000000000, 0.000000000000000000, 0.000000000000000000 ) ) ;
#17675 = CIRCLE ( 'NONE', #23676, 2.000000000000001776 ) ;
#17676 = DIRECTION ( 'NONE',  ( 1.000000000000000000, 0.000000000000000000, 0.000000000000000000 ) ) ;
#17677 = VERTEX_POINT ( 'NONE', #13368 ) ;
#17678 = EDGE_LOOP ( 'NONE', ( #102, #34075 ) ) ;
#17679 = CIRCLE ( 'NONE', #33267, 2.000000000000001776 ) ;
#17680 = AXIS2_PLACEMENT_3D ( 'NONE', #8203, #16832, #8006 ) ;
#17681 = VECTOR ( 'NONE', #2992, 1000.000000000000114 ) ;
#17682 = CARTESIAN_POINT ( 'NONE',  ( -48.00000337463112032, -51.96152422706641971, 17.49999999999999645 ) ) ;
#17683 = EDGE_LOOP ( 'NONE', ( #33019, #4790 ) ) ;
#17684 = DIRECTION ( 'NONE',  ( 0.000000000000000000, 0.000000000000000000, 1.000000000000000000 ) ) ;
#17685 = EDGE_LOOP ( 'NONE', ( #20987, #18140 ) ) ;
#17686 = CARTESIAN_POINT ( 'NONE',  ( -75.00000337463099243, -25.98076211353322051, -5.000000000000000000 ) ) ;
#17687 = EDGE_LOOP ( 'NONE', ( #36586, #5934 ) ) ;
#17688 = VECTOR ( 'NONE', #11154, 1000.000000000000000 ) ;
#17689 = ORIENTED_EDGE ( 'NONE', *, *, #18404, .F. ) ;
#17690 = AXIS2_PLACEMENT_3D ( 'NONE', #8645, #22739, #17089 ) ;
#17691 = DIRECTION ( 'NONE',  ( 1.000000000000000000, 0.000000000000000000, 0.000000000000000000 ) ) ;
#17692 = CARTESIAN_POINT ( 'NONE',  ( 1.898848305348270982, -4.677202111653177674, -0.6020238742160556322 ) ) ;
#17693 = CARTESIAN_POINT ( 'NONE',  ( 27.78182860042856461, 56.67878100130339902, -4.999999999999997335 ) ) ;
#17694 = EDGE_LOOP ( 'NONE', ( #29565, #33012, #23379, #6659, #14761 ) ) ;
#17695 = DIRECTION ( 'NONE',  ( 1.000000000000000000, 0.000000000000000000, 0.000000000000000000 ) ) ;
#17696 = DIRECTION ( 'NONE',  ( -0.000000000000000000, -0.000000000000000000, -1.000000000000000000 ) ) ;
#17697 = CARTESIAN_POINT ( 'NONE',  ( -5.000000000000463629, -1.027024708428717181, -3.969883389773432025 ) ) ;
#17698 = AXIS2_PLACEMENT_3D ( 'NONE', #17482, #29641, #23481 ) ;
#17699 = EDGE_LOOP ( 'NONE', ( #3368, #32634 ) ) ;
#17700 = CARTESIAN_POINT ( 'NONE',  ( -80.00000337463096400, -34.64101615137762025, -9.999999999999998224 ) ) ;
#17701 = DIRECTION ( 'NONE',  ( 0.000000000000000000, 0.000000000000000000, 1.000000000000000000 ) ) ;
#17702 = ORIENTED_EDGE ( 'NONE', *, *, #16633, .F. ) ;
#17703 = DIRECTION ( 'NONE',  ( 0.000000000000000000, 0.000000000000000000, 1.000000000000000000 ) ) ;
#17704 = AXIS2_PLACEMENT_3D ( 'NONE', #32646, #6970, #35663 ) ;
#17705 = CARTESIAN_POINT ( 'NONE',  ( 4.999996625368645198, 77.94228634059957983, -5.000000000000000000 ) ) ;
#17706 = CARTESIAN_POINT ( 'NONE',  ( -5.253368672218638125, -3.033033817057809500, -4.359491423763659945 ) ) ;
#17707 = AXIS2_PLACEMENT_3D ( 'NONE', #18136, #6704, #27312 ) ;
#17708 = AXIS2_PLACEMENT_3D ( 'NONE', #35468, #3759, #1143 ) ;
#17709 = CIRCLE ( 'NONE', #26088, 3.500000000000003109 ) ;
#17710 = DIRECTION ( 'NONE',  ( -1.000000000000000000, 0.000000000000000000, 0.000000000000000000 ) ) ;
#17711 = VECTOR ( 'NONE', #33130, 999.9999999999998863 ) ;
#17712 = ADVANCED_FACE ( 'NONE', ( #33814 ), #4394, .F. ) ;
#17713 = DIRECTION ( 'NONE',  ( 0.000000000000000000, 0.000000000000000000, -1.000000000000000000 ) ) ;
#17714 = EDGE_CURVE ( 'NONE', #19610, #7234, #20184, .T. ) ;
#17715 = LINE ( 'NONE', #6276, #8573 ) ;
#17716 = ORIENTED_EDGE ( 'NONE', *, *, #31504, .F. ) ;
#17717 = CARTESIAN_POINT ( 'NONE',  ( 0.000000000000000000, 0.000000000000000000, 27.50000000000000000 ) ) ;
#17718 = DIRECTION ( 'NONE',  ( -1.000000000000000000, 0.000000000000000000, 0.000000000000000000 ) ) ;
#17719 = CYLINDRICAL_SURFACE ( 'NONE', #16987, 2.000000000000001776 ) ;
#17720 = VERTEX_POINT ( 'NONE', #30068 ) ;
#17721 = AXIS2_PLACEMENT_3D ( 'NONE', #30133, #15897, #27331 ) ;
#17722 = EDGE_LOOP ( 'NONE', ( #24054, #22330, #17133, #27045, #10115 ) ) ;
#17723 = VERTEX_POINT ( 'NONE', #24650 ) ;
#17724 = CARTESIAN_POINT ( 'NONE',  ( 0.000000000000000000, 0.000000000000000000, -5.000000000000000888 ) ) ;
#17725 = DIRECTION ( 'NONE',  ( 0.8191520442889917986, 0.000000000000000000, 0.5735764363510460484 ) ) ;
#17726 = LINE ( 'NONE', #23936, #31419 ) ;
#17727 = AXIS2_PLACEMENT_3D ( 'NONE', #37050, #34411, #34240 ) ;
#17728 = AXIS2_PLACEMENT_3D ( 'NONE', #1340, #6968, #18781 ) ;
#17729 = CARTESIAN_POINT ( 'NONE',  ( -83.00000337463092137, -8.660254037844422825, 12.50000000000000000 ) ) ;
#17730 = VERTEX_POINT ( 'NONE', #27248 ) ;
#17731 = CARTESIAN_POINT ( 'NONE',  ( 4.999996625368645198, 77.94228634059957983, 12.50000000000000000 ) ) ;
#17732 = ORIENTED_EDGE ( 'NONE', *, *, #35813, .F. ) ;
#17733 = FACE_BOUND ( 'NONE', #23158, .T. ) ;
#17734 = CIRCLE ( 'NONE', #18956, 3.000000000000001332 ) ;
#17735 = VECTOR ( 'NONE', #26761, 1000.000000000000000 ) ;
#17736 = AXIS2_PLACEMENT_3D ( 'NONE', #9130, #17958, #31980 ) ;
#17737 = EDGE_CURVE ( 'NONE', #9159, #34784, #13597, .T. ) ;
#17738 = AXIS2_PLACEMENT_3D ( 'NONE', #29296, #17865, #22937 ) ;
#17739 = CIRCLE ( 'NONE', #12944, 2.000000000000001776 ) ;
#17740 = DIRECTION ( 'NONE',  ( -1.000000000000000000, -0.000000000000000000, -0.000000000000000000 ) ) ;
#17741 = CARTESIAN_POINT ( 'NONE',  ( 27.99999662536857414, -69.28203230275519786, -5.000000000000000000 ) ) ;
#17742 = EDGE_LOOP ( 'NONE', ( #9082, #33607, #14925, #12400 ) ) ;
#17743 = CARTESIAN_POINT ( 'NONE',  ( -43.00000337463111322, -77.94228634059960825, -9.999999999999998224 ) ) ;
#17744 = APPLICATION_PROTOCOL_DEFINITION ( 'draft international standard', 'automotive_design', 1998, #316 ) ;
#17745 = CIRCLE ( 'NONE', #28531, 2.000000000000001776 ) ;
#17746 = DIRECTION ( 'NONE',  ( -1.000000000000000000, 0.000000000000000000, 0.000000000000000000 ) ) ;
#17747 = LINE ( 'NONE', #34651, #19195 ) ;
#17748 = DIRECTION ( 'NONE',  ( -1.000000000000000000, 0.000000000000000000, -0.000000000000000000 ) ) ;
#17749 = EDGE_LOOP ( 'NONE', ( #26675, #12979, #9648, #6884, #18331 ) ) ;
#17750 = DIRECTION ( 'NONE',  ( 0.000000000000000000, 0.000000000000000000, 1.000000000000000000 ) ) ;
#17751 = DIRECTION ( 'NONE',  ( 1.000000000000000000, 0.000000000000000000, 0.000000000000000000 ) ) ;
#17752 = CARTESIAN_POINT ( 'NONE',  ( -80.00000337463094979, -17.32050807568882078, -9.999999999999998224 ) ) ;
#17753 = VERTEX_POINT ( 'NONE', #1571 ) ;
#17754 = ORIENTED_EDGE ( 'NONE', *, *, #32404, .F. ) ;
#17755 = CIRCLE ( 'NONE', #2807, 2.000000000000000000 ) ;
#17756 = EDGE_CURVE ( 'NONE', #31614, #12842, #29751, .T. ) ;
#17757 = ORIENTED_EDGE ( 'NONE', *, *, #8672, .T. ) ;
#17758 = MECHANICAL_DESIGN_GEOMETRIC_PRESENTATION_REPRESENTATION (  '', ( #33323 ), #20750 ) ;
#17759 = DIRECTION ( 'NONE',  ( 0.000000000000000000, 0.000000000000000000, 1.000000000000000000 ) ) ;
#17760 = CIRCLE ( 'NONE', #8774, 2.000000000000000000 ) ;
#17761 = CIRCLE ( 'NONE', #4013, 2.000000000000001776 ) ;
#17762 = CYLINDRICAL_SURFACE ( 'NONE', #7238, 2.000000000000001776 ) ;
#17763 = CIRCLE ( 'NONE', #27354, 20.00000000000001066 ) ;
#17764 = CARTESIAN_POINT ( 'NONE',  ( -80.00000337463094979, -17.32050807568882078, 17.49999999999999645 ) ) ;
#17765 = DIRECTION ( 'NONE',  ( 0.000000000000000000, 0.000000000000000000, 1.000000000000000000 ) ) ;
#17766 = DIRECTION ( 'NONE',  ( 0.000000000000000000, 0.000000000000000000, 1.000000000000000000 ) ) ;
#17767 = CYLINDRICAL_SURFACE ( 'NONE', #6, 3.500000000000003109 ) ;
#17768 = EDGE_LOOP ( 'NONE', ( #14848, #29763 ) ) ;
#17769 = VECTOR ( 'NONE', #27982, 1000.000000000000114 ) ;
#17770 = ORIENTED_EDGE ( 'NONE', *, *, #12027, .F. ) ;
#17771 = CARTESIAN_POINT ( 'NONE',  ( -31.74999999999995737, 0.000000000000000000, 0.000000000000000000 ) ) ;
#17772 = EDGE_CURVE ( 'NONE', #7403, #35706, #18397, .T. ) ;
#17773 = DIRECTION ( 'NONE',  ( -1.000000000000000000, 0.000000000000000000, 0.000000000000000000 ) ) ;
#17774 = PLANE ( 'NONE',  #12509 ) ;
#17775 = VERTEX_POINT ( 'NONE', #35907 ) ;
#17777 = ADVANCED_FACE ( 'NONE', ( #2330, #24826, #22012, #10216, #27803, #10766, #1770, #4582, #13759 ), #7943, .F. ) ;
#17776 = CIRCLE ( 'NONE', #12986, 3.500000000000003109 ) ;
#17778 = AXIS2_PLACEMENT_3D ( 'NONE', #16718, #2461, #11261 ) ;
#17779 = CIRCLE ( 'NONE', #34587, 1.999999999999998224 ) ;
#17780 = FACE_BOUND ( 'NONE', #17277, .T. ) ;
#17781 = ORIENTED_EDGE ( 'NONE', *, *, #25467, .F. ) ;
#17782 = ORIENTED_EDGE ( 'NONE', *, *, #14115, .T. ) ;
#17783 = ADVANCED_FACE ( 'NONE', ( #30796 ), #19023, .F. ) ;
#17784 = VECTOR ( 'NONE', #35987, 1000.000000000000000 ) ;
#17785 = DIRECTION ( 'NONE',  ( 0.000000000000000000, 0.000000000000000000, -1.000000000000000000 ) ) ;
#17786 = VERTEX_POINT ( 'NONE', #16214 ) ;
#17787 = MECHANICAL_DESIGN_GEOMETRIC_PRESENTATION_REPRESENTATION (  '', ( #413 ), #1630 ) ;
#17788 = CIRCLE ( 'NONE', #21387, 2.000000000000001776 ) ;
#17789 = DIRECTION ( 'NONE',  ( 0.000000000000000000, 0.000000000000000000, 1.000000000000000000 ) ) ;
#17790 = EDGE_CURVE ( 'NONE', #8725, #10442, #21390, .T. ) ;
#17791 = FACE_OUTER_BOUND ( 'NONE', #2849, .T. ) ;
#17792 = FACE_BOUND ( 'NONE', #33761, .T. ) ;
#17793 = EDGE_LOOP ( 'NONE', ( #21347, #3079 ) ) ;
#17794 = VERTEX_POINT ( 'NONE', #19216 ) ;
#17795 = VECTOR ( 'NONE', #7623, 1000.000000000000000 ) ;
#17796 = EDGE_LOOP ( 'NONE', ( #433, #30438, #24623, #32547 ) ) ;
#17797 = EDGE_LOOP ( 'NONE', ( #17320, #3686, #33382, #16915 ) ) ;
#17798 = VERTEX_POINT ( 'NONE', #33641 ) ;
#17799 = DIRECTION ( 'NONE',  ( 0.000000000000000000, 0.000000000000000000, 1.000000000000000000 ) ) ;
#17800 = VECTOR ( 'NONE', #29474, 1000.000000000000000 ) ;
#17801 = EDGE_CURVE ( 'NONE', #31731, #36755, #32445, .T. ) ;
#17802 = DIRECTION ( 'NONE',  ( 1.000000000000000000, 0.000000000000000000, 0.000000000000000000 ) ) ;
#17803 = VERTEX_POINT ( 'NONE', #16932 ) ;
#17805 = VECTOR ( 'NONE', #30067, 1000.000000000000000 ) ;
#17804 = CARTESIAN_POINT ( 'NONE',  ( -20.00000337463123756, -69.28203230275522628, -5.000000000000000000 ) ) ;
#17806 = CARTESIAN_POINT ( 'NONE',  ( 105.1747985409462700, 37.32408539865060249, 32.49999999999999289 ) ) ;
#17807 = DIRECTION ( 'NONE',  ( -1.000000000000000000, 1.082992363797667670E-14, 0.000000000000000000 ) ) ;
#17808 = VERTEX_POINT ( 'NONE', #17314 ) ;
#17809 = CYLINDRICAL_SURFACE ( 'NONE', #16452, 2.000000000000001776 ) ;
#17810 = VECTOR ( 'NONE', #19658, 1000.000000000000000 ) ;
#17811 = DIRECTION ( 'NONE',  ( -0.000000000000000000, -0.000000000000000000, 1.000000000000000000 ) ) ;
#17812 = CYLINDRICAL_SURFACE ( 'NONE', #15828, 2.000000000000001776 ) ;
#17813 = ORIENTED_EDGE ( 'NONE', *, *, #34334, .T. ) ;
#17814 = LINE ( 'NONE', #6186, #29211 ) ;
#17815 = CARTESIAN_POINT ( 'NONE',  ( -10.00000337463128197, 86.60254037844397601, -9.999999999999998224 ) ) ;
#17816 = ORIENTED_EDGE ( 'NONE', *, *, #7239, .T. ) ;
#17817 = ADVANCED_FACE ( 'NONE', ( #6056 ), #11650, .F. ) ;
#17818 = CIRCLE ( 'NONE', #9419, 2.000000000000001776 ) ;
#17819 = ORIENTED_EDGE ( 'NONE', *, *, #16679, .F. ) ;
#17820 = CIRCLE ( 'NONE', #1662, 2.000000000000001776 ) ;
#17821 = CARTESIAN_POINT ( 'NONE',  ( -45.00000337463111322, 60.62177826491077326, 12.50000000000000000 ) ) ;
#17822 = ADVANCED_FACE ( 'NONE', ( #25564 ), #36807, .F. ) ;
#17823 = CARTESIAN_POINT ( 'NONE',  ( -75.00000337463099243, -25.98076211353322051, 12.50000000000000000 ) ) ;
#17824 = DIRECTION ( 'NONE',  ( 0.000000000000000000, 0.8660254037844380415, -0.5000000000000012212 ) ) ;
#17825 = CYLINDRICAL_SURFACE ( 'NONE', #11870, 2.000000000000001776 ) ;
#17826 = ORIENTED_EDGE ( 'NONE', *, *, #35108, .F. ) ;
#17827 = AXIS2_PLACEMENT_3D ( 'NONE', #4022, #9820, #7570 ) ;
#17828 = FACE_BOUND ( 'NONE', #17189, .T. ) ;
#17829 = CARTESIAN_POINT ( 'NONE',  ( 24.99999662536857059, 77.94228634059957983, -9.999999999999998224 ) ) ;
#17830 = AXIS2_PLACEMENT_3D ( 'NONE', #17103, #31339, #25362 ) ;
#17831 = ORIENTED_EDGE ( 'NONE', *, *, #6192, .T. ) ;
#17832 = EDGE_CURVE ( 'NONE', #26576, #6626, #9704, .T. ) ;
#17833 = CIRCLE ( 'NONE', #3476, 3.500000000000003109 ) ;
#17834 = CIRCLE ( 'NONE', #2268, 8.500000000000003553 ) ;
#17835 = DIRECTION ( 'NONE',  ( 1.000000000000000000, 0.000000000000000000, 0.000000000000000000 ) ) ;
#17836 = ORIENTED_EDGE ( 'NONE', *, *, #13040, .T. ) ;
#17837 = AXIS2_PLACEMENT_3D ( 'NONE', #30501, #1429, #18692 ) ;
#17838 = LINE ( 'NONE', #12009, #28467 ) ;
#17839 = DIRECTION ( 'NONE',  ( -0.000000000000000000, -0.000000000000000000, 1.000000000000000000 ) ) ;
#17840 = EDGE_CURVE ( 'NONE', #20086, #13680, #15105, .T. ) ;
#17841 = CARTESIAN_POINT ( 'NONE',  ( -20.00000337463123756, -69.28203230275522628, -9.999999999999998224 ) ) ;
#17842 = EDGE_LOOP ( 'NONE', ( #33306, #21024, #4914, #33277, #19204 ) ) ;
#17843 = ORIENTED_EDGE ( 'NONE', *, *, #1961, .T. ) ;
#17844 = CARTESIAN_POINT ( 'NONE',  ( 64.99999662536842493, 43.30127018922200222, -9.999999999999998224 ) ) ;
#17845 = DIRECTION ( 'NONE',  ( 0.000000000000000000, -1.224646799147353207E-16, 1.000000000000000000 ) ) ;
#17846 = DIRECTION ( 'NONE',  ( -0.000000000000000000, -0.000000000000000000, 1.000000000000000000 ) ) ;
#17847 = AXIS2_PLACEMENT_3D ( 'NONE', #2241, #21929, #29997 ) ;
#17848 = ORIENTED_EDGE ( 'NONE', *, *, #22659, .T. ) ;
#17849 = DIRECTION ( 'NONE',  ( 0.000000000000000000, 0.000000000000000000, 1.000000000000000000 ) ) ;
#17850 = FACE_BOUND ( 'NONE', #28501, .T. ) ;
#17851 = DIRECTION ( 'NONE',  ( 0.000000000000000000, 0.000000000000000000, 1.000000000000000000 ) ) ;
#17852 = DIRECTION ( 'NONE',  ( 0.000000000000000000, 0.000000000000000000, 1.000000000000000000 ) ) ;
#17853 = AXIS2_PLACEMENT_3D ( 'NONE', #27541, #1853, #19657 ) ;
#17854 = DIRECTION ( 'NONE',  ( 0.000000000000000000, 0.000000000000000000, -1.000000000000000000 ) ) ;
#17855 = VERTEX_POINT ( 'NONE', #13929 ) ;
#17856 = CARTESIAN_POINT ( 'NONE',  ( 0.000000000000000000, 0.000000000000000000, 32.50000000000000000 ) ) ;
#17857 = PRODUCT_DEFINITION_SHAPE ( 'NONE', 'NONE',  #2674 ) ;
#17858 = EDGE_CURVE ( 'NONE', #25623, #27946, #7915, .T. ) ;
#17859 =( NAMED_UNIT ( * ) PLANE_ANGLE_UNIT ( ) SI_UNIT ( $, .RADIAN. ) );
#17860 = CIRCLE ( 'NONE', #7082, 2.000000000000001776 ) ;
#17861 = LINE ( 'NONE', #9779, #15181 ) ;
#17862 = ORIENTED_EDGE ( 'NONE', *, *, #4264, .F. ) ;
#17863 = DIRECTION ( 'NONE',  ( -1.000000000000000000, 0.000000000000000000, 0.000000000000000000 ) ) ;
#17864 = CIRCLE ( 'NONE', #23874, 2.000000000000001776 ) ;
#17865 = DIRECTION ( 'NONE',  ( 0.000000000000000000, 0.000000000000000000, 1.000000000000000000 ) ) ;
#17866 = DIRECTION ( 'NONE',  ( 1.000000000000000000, 0.000000000000000000, 0.000000000000000000 ) ) ;
#17867 = VECTOR ( 'NONE', #9474, 1000.000000000000000 ) ;
#17868 = ORIENTED_EDGE ( 'NONE', *, *, #12302, .F. ) ;
#17869 = EDGE_CURVE ( 'NONE', #12378, #20688, #8529, .T. ) ;
#17870 = VERTEX_POINT ( 'NONE', #28903 ) ;
#17871 = VERTEX_POINT ( 'NONE', #14488 ) ;
#17872 = AXIS2_PLACEMENT_3D ( 'NONE', #16856, #2237, #19479 ) ;
#17873 = EDGE_CURVE ( 'NONE', #32213, #4038, #21074, .T. ) ;
#17874 = DIRECTION ( 'NONE',  ( -1.000000000000000000, 0.000000000000000000, 0.000000000000000000 ) ) ;
#17875 = CARTESIAN_POINT ( 'NONE',  ( -44.13139720814439215, -27.49999999999955591, -5.000000000000000000 ) ) ;
#17876 = ADVANCED_FACE ( 'NONE', ( #22559 ), #34559, .T. ) ;
#17877 = CARTESIAN_POINT ( 'NONE',  ( 72.99999662536836809, 25.98076211353319565, -5.000000000000000000 ) ) ;
#17878 = ORIENTED_EDGE ( 'NONE', *, *, #12525, .T. ) ;
#17879 = ORIENTED_EDGE ( 'NONE', *, *, #11086, .T. ) ;
#17880 = ORIENTED_EDGE ( 'NONE', *, *, #9426, .F. ) ;
#17881 = AXIS2_PLACEMENT_3D ( 'NONE', #9021, #3042, #22734 ) ;
#17882 = AXIS2_PLACEMENT_3D ( 'NONE', #29499, #3818, #15257 ) ;
#17883 = DIRECTION ( 'NONE',  ( 0.000000000000000000, 0.000000000000000000, 1.000000000000000000 ) ) ;
#17884 = ORIENTED_EDGE ( 'NONE', *, *, #27274, .T. ) ;
#17885 = DIRECTION ( 'NONE',  ( 0.000000000000000000, 0.000000000000000000, 1.000000000000000000 ) ) ;
#17886 = ORIENTED_EDGE ( 'NONE', *, *, #36022, .T. ) ;
#17887 = CARTESIAN_POINT ( 'NONE',  ( 74.99999662536836809, -8.660254037844401509, 17.49999999999999645 ) ) ;
#17888 = EDGE_LOOP ( 'NONE', ( #29450, #2771, #2961, #9408, #19804, #3185 ) ) ;
#17889 = ORIENTED_EDGE ( 'NONE', *, *, #33732, .T. ) ;
#17890 = DIRECTION ( 'NONE',  ( 0.000000000000000000, 0.000000000000000000, 1.000000000000000000 ) ) ;
#17891 = DIRECTION ( 'NONE',  ( 1.000000000000000000, 0.000000000000000000, 0.000000000000000000 ) ) ;
#17892 = ADVANCED_FACE ( 'NONE', ( #14110 ), #17118, .T. ) ;
#17893 = CIRCLE ( 'NONE', #11280, 2.000000000000001776 ) ;
#17894 = DIRECTION ( 'NONE',  ( 0.000000000000000000, 0.000000000000000000, 1.000000000000000000 ) ) ;
#17895 = EDGE_LOOP ( 'NONE', ( #22515, #24359, #18623 ) ) ;
#17896 = VERTEX_POINT ( 'NONE', #31002 ) ;
#17897 = CARTESIAN_POINT ( 'NONE',  ( 0.000000000000000000, 0.000000000000000000, 2.266666666666999674 ) ) ;
#17898 = CARTESIAN_POINT ( 'NONE',  ( 37.99999662536853151, 69.28203230275518365, 17.49999999999999645 ) ) ;
#17899 = CARTESIAN_POINT ( 'NONE',  ( 44.13139720814401556, -27.50000000000022737, -5.000000000000000000 ) ) ;
#17900 = ORIENTED_EDGE ( 'NONE', *, *, #25538, .F. ) ;
#17901 = DIRECTION ( 'NONE',  ( 1.000000000000000000, 0.000000000000000000, 0.000000000000000000 ) ) ;
#17902 = DIRECTION ( 'NONE',  ( -1.000000000000000000, 0.000000000000000000, 0.000000000000000000 ) ) ;
#17903 = CIRCLE ( 'NONE', #3533, 2.000000000000001776 ) ;
#17904 = VERTEX_POINT ( 'NONE', #22763 ) ;
#17905 = CARTESIAN_POINT ( 'NONE',  ( -25.00000337463121980, -77.94228634059963667, -9.999999999999998224 ) ) ;
#17906 = LINE ( 'NONE', #22978, #17867 ) ;
#17907 = CARTESIAN_POINT ( 'NONE',  ( -44.13139720814380240, 27.50000000000055422, -5.000000000000000888 ) ) ;
#17908 = AXIS2_PLACEMENT_3D ( 'NONE', #34683, #23230, #1093 ) ;
#17909 = DIRECTION ( 'NONE',  ( -0.000000000000000000, -0.000000000000000000, 1.000000000000000000 ) ) ;
#17910 = AXIS2_PLACEMENT_3D ( 'NONE', #30136, #13439, #10450 ) ;
#17911 = EDGE_CURVE ( 'NONE', #11966, #31223, #14314, .T. ) ;
#17912 = CARTESIAN_POINT ( 'NONE',  ( 84.99999662536832545, 25.98076211353319565, -9.999999999999998224 ) ) ;
#17913 = DIRECTION ( 'NONE',  ( 0.000000000000000000, 0.000000000000000000, 1.000000000000000000 ) ) ;
#17914 = AXIS2_PLACEMENT_3D ( 'NONE', #3662, #6274, #35170 ) ;
#17915 = EDGE_LOOP ( 'NONE', ( #31825, #12575 ) ) ;
#17916 = ADVANCED_FACE ( 'NONE', ( #5336 ), #2883, .T. ) ;
#17917 = DIRECTION ( 'NONE',  ( -0.000000000000000000, -0.000000000000000000, 1.000000000000000000 ) ) ;
#17918 = CARTESIAN_POINT ( 'NONE',  ( 61.99999662536842493, 51.96152422706639129, 12.50000000000000000 ) ) ;
#17919 = CYLINDRICAL_SURFACE ( 'NONE', #35578, 33.00000000000001421 ) ;
#17920 = EDGE_LOOP ( 'NONE', ( #7535, #16728, #28527, #4295 ) ) ;
#17921 = ORIENTED_EDGE ( 'NONE', *, *, #32007, .T. ) ;
#17922 = VERTEX_POINT ( 'NONE', #28740 ) ;
#17923 = AXIS2_PLACEMENT_3D ( 'NONE', #7855, #16658, #27539 ) ;
#17924 = CARTESIAN_POINT ( 'NONE',  ( -5.750000000000036415, 83.21147890756139986, -24.99999999999999645 ) ) ;
#17925 = DIRECTION ( 'NONE',  ( 0.000000000000000000, 0.000000000000000000, 1.000000000000000000 ) ) ;
#17926 = EDGE_CURVE ( 'NONE', #28198, #31907, #33067, .T. ) ;
#17927 = VECTOR ( 'NONE', #4112, 1000.000000000000000 ) ;
#17928 = CARTESIAN_POINT ( 'NONE',  ( 44.99999662536849598, -77.94228634059960825, -5.000000000000000000 ) ) ;
#17929 = DIRECTION ( 'NONE',  ( 1.000000000000000000, 0.000000000000000000, 0.000000000000000000 ) ) ;
#17930 = FACE_OUTER_BOUND ( 'NONE', #9819, .T. ) ;
#17931 = VERTEX_POINT ( 'NONE', #19570 ) ;
#17932 = CIRCLE ( 'NONE', #29291, 2.000000000000001776 ) ;
#17933 = CARTESIAN_POINT ( 'NONE',  ( -63.00000337463102085, 60.62177826491077326, 17.49999999999999645 ) ) ;
#17934 = ORIENTED_EDGE ( 'NONE', *, *, #18033, .F. ) ;
#17935 = FACE_BOUND ( 'NONE', #26690, .T. ) ;
#17936 = AXIS2_PLACEMENT_3D ( 'NONE', #36880, #28074, #5951 ) ;
#17937 = ADVANCED_FACE ( 'NONE', ( #8669 ), #8329, .F. ) ;
#17938 = ADVANCED_FACE ( 'NONE', ( #3068 ), #25923, .F. ) ;
#17939 = AXIS2_PLACEMENT_3D ( 'NONE', #20730, #21108, #7057 ) ;
#17940 = DIRECTION ( 'NONE',  ( 0.000000000000000000, 0.000000000000000000, 1.000000000000000000 ) ) ;
#17941 = EDGE_CURVE ( 'NONE', #22919, #34990, #609, .T. ) ;
#17942 = EDGE_CURVE ( 'NONE', #34090, #35050, #18036, .T. ) ;
#17943 = FACE_BOUND ( 'NONE', #24111, .T. ) ;
#17944 = EDGE_LOOP ( 'NONE', ( #10446, #2898 ) ) ;
#17945 = LINE ( 'NONE', #26548, #9860 ) ;
#17946 = CARTESIAN_POINT ( 'NONE',  ( -20.00000337463123756, -86.60254037844400443, -9.999999999999998224 ) ) ;
#17947 = AXIS2_PLACEMENT_3D ( 'NONE', #11393, #8575, #3315 ) ;
#17948 = DIRECTION ( 'NONE',  ( 0.000000000000000000, 0.000000000000000000, -1.000000000000000000 ) ) ;
#17949 = DIRECTION ( 'NONE',  ( -0.000000000000000000, -0.000000000000000000, 1.000000000000000000 ) ) ;
#17950 = ORIENTED_EDGE ( 'NONE', *, *, #27648, .F. ) ;
#17951 = CARTESIAN_POINT ( 'NONE',  ( 0.000000000000000000, 0.000000000000000000, 12.49999999999999822 ) ) ;
#17952 = CIRCLE ( 'NONE', #32918, 2.000000000000001776 ) ;
#17953 = CARTESIAN_POINT ( 'NONE',  ( -65.00000337463102085, 60.62177826491077326, -9.999999999999998224 ) ) ;
#17954 = DIRECTION ( 'NONE',  ( 1.000000000000000000, 0.000000000000000000, 0.000000000000000000 ) ) ;
#17955 = VERTEX_POINT ( 'NONE', #12023 ) ;
#17956 = VERTEX_POINT ( 'NONE', #29088 ) ;
#17957 = ORIENTED_EDGE ( 'NONE', *, *, #18622, .T. ) ;
#17958 = DIRECTION ( 'NONE',  ( 0.000000000000000000, 0.000000000000000000, 1.000000000000000000 ) ) ;
#17959 = DIRECTION ( 'NONE',  ( 0.000000000000000000, 0.000000000000000000, -1.000000000000000000 ) ) ;
#17960 = ADVANCED_FACE ( 'NONE', ( #26300 ), #15042, .F. ) ;
#17961 = DIRECTION ( 'NONE',  ( 1.000000000000000000, 0.000000000000000000, 0.000000000000000000 ) ) ;
#17962 = CIRCLE ( 'NONE', #3517, 1.999999999999998224 ) ;
#17963 = AXIS2_PLACEMENT_3D ( 'NONE', #9778, #30029, #12399 ) ;
#17964 = DIRECTION ( 'NONE',  ( -1.000000000000000000, 0.000000000000000000, 0.000000000000000000 ) ) ;
#17965 = CARTESIAN_POINT ( 'NONE',  ( -107.2243249565953533, -49.31268038019268118, 32.50000000000000711 ) ) ;
#17966 = VECTOR ( 'NONE', #22155, 1000.000000000000000 ) ;
#17967 = DIRECTION ( 'NONE',  ( 0.000000000000000000, 0.000000000000000000, -1.000000000000000000 ) ) ;
#17968 = EDGE_LOOP ( 'NONE', ( #30584, #12330, #20662, #24994, #26772 ) ) ;
#17969 = ORIENTED_EDGE ( 'NONE', *, *, #21761, .F. ) ;
#17970 = CYLINDRICAL_SURFACE ( 'NONE', #12886, 2.000000000000000000 ) ;
#17971 = CIRCLE ( 'NONE', #19166, 2.000000000000001776 ) ;
#17972 = CYLINDRICAL_SURFACE ( 'NONE', #8585, 2.000000000000001776 ) ;
#17973 = ORIENTED_EDGE ( 'NONE', *, *, #26296, .F. ) ;
#17974 = CARTESIAN_POINT ( 'NONE',  ( 4.999996625368645198, 77.94228634059957983, -5.000000000000000000 ) ) ;
#17975 = VERTEX_POINT ( 'NONE', #32283 ) ;
#17976 = AXIS2_PLACEMENT_3D ( 'NONE', #10805, #14158, #17168 ) ;
#17977 = FACE_BOUND ( 'NONE', #19512, .T. ) ;
#17978 = VERTEX_POINT ( 'NONE', #29458 ) ;
#17979 = VERTEX_POINT ( 'NONE', #23480 ) ;
#17980 = EDGE_CURVE ( 'NONE', #12977, #5893, #19298, .T. ) ;
#17981 = AXIS2_PLACEMENT_3D ( 'NONE', #26479, #15426, #27564 ) ;
#17982 = DIRECTION ( 'NONE',  ( 0.000000000000000000, 0.000000000000000000, 1.000000000000000000 ) ) ;
#17983 = ORIENTED_EDGE ( 'NONE', *, *, #24667, .T. ) ;
#17984 = DIRECTION ( 'NONE',  ( 1.000000000000000000, 0.000000000000000000, 0.000000000000000000 ) ) ;
#17985 = CARTESIAN_POINT ( 'NONE',  ( 2.500000000000005773, 4.330127018922191873, -6.000000000000000000 ) ) ;
#17986 = DIRECTION ( 'NONE',  ( 0.000000000000000000, 0.000000000000000000, 1.000000000000000000 ) ) ;
#17987 = AXIS2_PLACEMENT_3D ( 'NONE', #366, #23262, #31849 ) ;
#17988 = ORIENTED_EDGE ( 'NONE', *, *, #35261, .T. ) ;
#17989 = ORIENTED_EDGE ( 'NONE', *, *, #32564, .F. ) ;
#17990 = ORIENTED_EDGE ( 'NONE', *, *, #20162, .F. ) ;
#17991 = ORIENTED_EDGE ( 'NONE', *, *, #9739, .F. ) ;
#17992 = ORIENTED_EDGE ( 'NONE', *, *, #13228, .F. ) ;
#17993 = CARTESIAN_POINT ( 'NONE',  ( 4.279621169095998212, -62.97617850287780072, -49.86561046011506448 ) ) ;
#17994 = CARTESIAN_POINT ( 'NONE',  ( 5.999999999999998224, 145.0000000000000568, 32.55002500000000509 ) ) ;
#17995 = ORIENTED_EDGE ( 'NONE', *, *, #5057, .T. ) ;
#17996 = CARTESIAN_POINT ( 'NONE',  ( -27.00000337463120914, 77.94228634059957983, 17.49999999999999645 ) ) ;
#17997 = CARTESIAN_POINT ( 'NONE',  ( 96.68597835076329261, 67.93726906584150527, 32.49999999999999289 ) ) ;
#17998 = DIRECTION ( 'NONE',  ( 0.000000000000000000, 0.000000000000000000, 1.000000000000000000 ) ) ;
#17999 = EDGE_CURVE ( 'NONE', #14051, #15920, #32642, .T. ) ;
#18000 = VERTEX_POINT ( 'NONE', #6608 ) ;
#18001 = CARTESIAN_POINT ( 'NONE',  ( 31.46585318596250502, 86.45172111230321832, -4.999999999999997335 ) ) ;
#18002 = ADVANCED_FACE ( 'NONE', ( #15214 ), #12758, .T. ) ;
#18003 = CARTESIAN_POINT ( 'NONE',  ( 35.19434990244975126, -52.39915983220758022, -49.22241343995298024 ) ) ;
#18004 = CARTESIAN_POINT ( 'NONE',  ( -70.00000337463102085, -51.96152422706641971, 17.49999999999999645 ) ) ;
#18005 = ORIENTED_EDGE ( 'NONE', *, *, #18624, .T. ) ;
#18006 = CARTESIAN_POINT ( 'NONE',  ( -25.00000337463120914, 77.94228634059957983, -9.999999999999998224 ) ) ;
#18007 = EDGE_CURVE ( 'NONE', #1000, #30871, #26226, .T. ) ;
#18008 = DIRECTION ( 'NONE',  ( 0.000000000000000000, 0.000000000000000000, -1.000000000000000000 ) ) ;
#18009 = VERTEX_POINT ( 'NONE', #26468 ) ;
#18010 = VERTEX_POINT ( 'NONE', #21032 ) ;
#18011 = ADVANCED_FACE ( 'NONE', ( #6967, #18418 ), #6414, .F. ) ;
#18012 = LINE ( 'NONE', #9578, #16456 ) ;
#18013 = FACE_OUTER_BOUND ( 'NONE', #29332, .T. ) ;
#18014 = CIRCLE ( 'NONE', #14425, 2.000000000000001776 ) ;
#18015 = CARTESIAN_POINT ( 'NONE',  ( -4.279621169095561228, 62.97617850287782915, -49.86561046011506448 ) ) ;
#18016 = DIRECTION ( 'NONE',  ( 0.000000000000000000, 0.000000000000000000, 1.000000000000000000 ) ) ;
#18017 = VERTEX_POINT ( 'NONE', #26654 ) ;
#18018 = FACE_BOUND ( 'NONE', #13081, .T. ) ;
#18019 = DIRECTION ( 'NONE',  ( 0.000000000000000000, 0.000000000000000000, 1.000000000000000000 ) ) ;
#18020 = VERTEX_POINT ( 'NONE', #1168 ) ;
#18021 = EDGE_CURVE ( 'NONE', #26481, #31719, #33668, .T. ) ;
#18022 = DIRECTION ( 'NONE',  ( -1.000000000000000000, 0.000000000000000000, 0.000000000000000000 ) ) ;
#18023 = VERTEX_POINT ( 'NONE', #971 ) ;
#18024 = LINE ( 'NONE', #29446, #13912 ) ;
#18025 = DIRECTION ( 'NONE',  ( -1.000000000000000000, -2.569960705150823820E-15, 0.000000000000000000 ) ) ;
#18026 = DIRECTION ( 'NONE',  ( 1.000000000000000000, 0.000000000000000000, 0.000000000000000000 ) ) ;
#18027 = EDGE_LOOP ( 'NONE', ( #19649, #25863, #24970, #7181, #31500 ) ) ;
#18028 = ORIENTED_EDGE ( 'NONE', *, *, #32366, .F. ) ;
#18029 = CARTESIAN_POINT ( 'NONE',  ( -83.00000337463092137, -25.98076211353322051, -9.999999999999998224 ) ) ;
#18030 = CARTESIAN_POINT ( 'NONE',  ( -73.00000337463097821, 8.660254037844374864, -9.999999999999998224 ) ) ;
#18031 = ORIENTED_EDGE ( 'NONE', *, *, #27682, .T. ) ;
#18032 = CARTESIAN_POINT ( 'NONE',  ( 6.999996625368645198, 77.94228634059957983, 12.50000000000000000 ) ) ;
#18033 = EDGE_CURVE ( 'NONE', #26254, #30697, #6702, .T. ) ;
#18034 = CARTESIAN_POINT ( 'NONE',  ( 39.99999662536853151, 69.28203230275518365, -9.999999999999998224 ) ) ;
#18035 = DIRECTION ( 'NONE',  ( -0.7650473262243671080, -0.6439740589782688707, 0.000000000000000000 ) ) ;
#18036 = LINE ( 'NONE', #35313, #19897 ) ;
#18037 = DIRECTION ( 'NONE',  ( -1.000000000000000000, 0.000000000000000000, 0.000000000000000000 ) ) ;
#18038 = ORIENTED_EDGE ( 'NONE', *, *, #9110, .T. ) ;
#18039 = CARTESIAN_POINT ( 'NONE',  ( -70.00000337463099243, 51.96152422706637708, -9.999999999999998224 ) ) ;
#18040 = PRESENTATION_STYLE_ASSIGNMENT (( #8675 ) ) ;
#18041 = CYLINDRICAL_SURFACE ( 'NONE', #22386, 3.000000000000002665 ) ;
#18042 = ORIENTED_EDGE ( 'NONE', *, *, #22280, .F. ) ;
#18043 = DIRECTION ( 'NONE',  ( 0.000000000000000000, 1.000000000000000000, -1.034244904716769672E-15 ) ) ;
#18044 = EDGE_CURVE ( 'NONE', #5564, #34031, #112, .T. ) ;
#18045 = FACE_OUTER_BOUND ( 'NONE', #11382, .T. ) ;
#18046 = LINE ( 'NONE', #20861, #27572 ) ;
#18047 = ORIENTED_EDGE ( 'NONE', *, *, #7581, .F. ) ;
#18048 = ORIENTED_EDGE ( 'NONE', *, *, #5259, .F. ) ;
#18049 = EDGE_CURVE ( 'NONE', #11321, #35086, #14492, .T. ) ;
#18050 = AXIS2_PLACEMENT_3D ( 'NONE', #13196, #24643, #10372 ) ;
#18051 = CARTESIAN_POINT ( 'NONE',  ( 2.714587707229039193, -4.206234748388752998, -2.383804823457777444E-14 ) ) ;
#18052 = DIRECTION ( 'NONE',  ( 1.000000000000000000, 0.000000000000000000, 0.000000000000000000 ) ) ;
#18053 = CARTESIAN_POINT ( 'NONE',  ( 4.999996625368645198, 77.94228634059957983, 12.50000000000000000 ) ) ;
#18054 = ORIENTED_EDGE ( 'NONE', *, *, #19574, .T. ) ;
#18055 = CIRCLE ( 'NONE', #1898, 2.000000000000001776 ) ;
#18056 = ORIENTED_EDGE ( 'NONE', *, *, #18993, .F. ) ;
#18057 = ORIENTED_EDGE ( 'NONE', *, *, #18812, .T. ) ;
#18058 = FACE_OUTER_BOUND ( 'NONE', #33704, .T. ) ;
#18059 = EDGE_LOOP ( 'NONE', ( #27569, #21691, #9149 ) ) ;
#18060 = CARTESIAN_POINT ( 'NONE',  ( -16.35104710633394376, -113.9564291516891927, 32.50000000000000000 ) ) ;
#18061 = ORIENTED_EDGE ( 'NONE', *, *, #6656, .F. ) ;
#18062 = DIRECTION ( 'NONE',  ( 0.000000000000000000, 0.000000000000000000, 1.000000000000000000 ) ) ;
#18063 = ORIENTED_EDGE ( 'NONE', *, *, #2780, .F. ) ;
#18064 = EDGE_LOOP ( 'NONE', ( #30949, #32657 ) ) ;
#18065 = EDGE_CURVE ( 'NONE', #17340, #36526, #16903, .T. ) ;
#18066 = DIRECTION ( 'NONE',  ( 1.000000000000000000, 0.000000000000000000, 0.000000000000000000 ) ) ;
#18067 = DIRECTION ( 'NONE',  ( 0.1391731009600657432, -1.704378926181559679E-17, 0.9902680687415703620 ) ) ;
#18068 = ORIENTED_EDGE ( 'NONE', *, *, #2164, .F. ) ;
#18069 = ORIENTED_EDGE ( 'NONE', *, *, #12735, .F. ) ;
#18070 = DIRECTION ( 'NONE',  ( 0.000000000000000000, 0.000000000000000000, 1.000000000000000000 ) ) ;
#18071 = DIRECTION ( 'NONE',  ( 0.000000000000000000, 0.000000000000000000, -1.000000000000000000 ) ) ;
#18072 = EDGE_CURVE ( 'NONE', #26842, #35523, #722, .T. ) ;
#18073 = CARTESIAN_POINT ( 'NONE',  ( 5.000000000000000000, -2.886751345948134428, -6.000000000000000000 ) ) ;
#18074 = CARTESIAN_POINT ( 'NONE',  ( -5.000000000000000888, -3.131509683642110353, -4.027949516396631680 ) ) ;
#18075 = ORIENTED_EDGE ( 'NONE', *, *, #26763, .T. ) ;
#18076 = CARTESIAN_POINT ( 'NONE',  ( -34.00000000000027711, -58.88972745734168512, 12.49999999999999822 ) ) ;
#18077 = CARTESIAN_POINT ( 'NONE',  ( 71.99999662536838230, -34.64101615137759183, -9.999999999999998224 ) ) ;
#18078 = AXIS2_PLACEMENT_3D ( 'NONE', #16767, #19760, #24211 ) ;
#18080 = ORIENTED_EDGE ( 'NONE', *, *, #5921, .F. ) ;
#18079 = EDGE_CURVE ( 'NONE', #24231, #27194, #3728, .T. ) ;
#18081 = DIRECTION ( 'NONE',  ( 1.000000000000000000, 0.000000000000000000, 0.000000000000000000 ) ) ;
#18082 = CARTESIAN_POINT ( 'NONE',  ( 39.27785635698568711, 86.50000000000001421, 27.50000000000000000 ) ) ;
#18083 = CARTESIAN_POINT ( 'NONE',  ( -52.00000337463110611, -69.28203230275519786, -5.000000000000000000 ) ) ;
#18084 = DIRECTION ( 'NONE',  ( -1.000000000000000000, 0.000000000000000000, 0.000000000000000000 ) ) ;
#18085 = CARTESIAN_POINT ( 'NONE',  ( -55.88972745734203329, -33.99999999999965894, -49.86561046011506448 ) ) ;
#18086 = CARTESIAN_POINT ( 'NONE',  ( 5.000000000000000000, 6.074766241781102566E-16, -0.5080592402122449114 ) ) ;
#18087 = ORIENTED_EDGE ( 'NONE', *, *, #28257, .T. ) ;
#18088 = DIRECTION ( 'NONE',  ( 0.000000000000000000, 0.000000000000000000, -1.000000000000000000 ) ) ;
#18089 = CARTESIAN_POINT ( 'NONE',  ( -27.00000337463120914, 77.94228634059957983, -5.000000000000000000 ) ) ;
#18090 = LINE ( 'NONE', #26910, #16930 ) ;
#18091 = ORIENTED_EDGE ( 'NONE', *, *, #13643, .F. ) ;
#18092 = EDGE_LOOP ( 'NONE', ( #1520, #16956, #18497, #10238 ) ) ;
#18093 = ORIENTED_EDGE ( 'NONE', *, *, #36714, .T. ) ;
#18094 = EDGE_CURVE ( 'NONE', #15624, #17979, #20471, .T. ) ;
#18095 = DIRECTION ( 'NONE',  ( 0.000000000000000000, 0.000000000000000000, 1.000000000000000000 ) ) ;
#18096 = CARTESIAN_POINT ( 'NONE',  ( 0.000000000000000000, 0.000000000000000000, -5.000000000000000000 ) ) ;
#18097 = DIRECTION ( 'NONE',  ( 0.000000000000000000, 0.000000000000000000, 1.000000000000000000 ) ) ;
#18098 = DIRECTION ( 'NONE',  ( -1.000000000000000000, 0.000000000000000000, 0.000000000000000000 ) ) ;
#18099 = CIRCLE ( 'NONE', #1938, 3.499999999999987566 ) ;
#18100 = CARTESIAN_POINT ( 'NONE',  ( 86.99999662536832545, 25.98076211353319565, -9.999999999999998224 ) ) ;
#18101 = VERTEX_POINT ( 'NONE', #5081 ) ;
#18102 = DIRECTION ( 'NONE',  ( 0.7071067811865389130, -0.7071067811865561215, 0.000000000000000000 ) ) ;
#18103 = ORIENTED_EDGE ( 'NONE', *, *, #19958, .F. ) ;
#18104 = FACE_BOUND ( 'NONE', #18433, .T. ) ;
#18105 = EDGE_CURVE ( 'NONE', #30085, #13632, #4330, .T. ) ;
#18106 = FACE_OUTER_BOUND ( 'NONE', #4917, .T. ) ;
#18107 = DIRECTION ( 'NONE',  ( -1.000000000000000000, 0.000000000000000000, -0.000000000000000000 ) ) ;
#18108 = ADVANCED_FACE ( 'NONE', ( #16521 ), #10316, .T. ) ;
#18109 = ORIENTED_EDGE ( 'NONE', *, *, #1746, .F. ) ;
#18110 = DIRECTION ( 'NONE',  ( 1.000000000000000000, 0.000000000000000000, 0.000000000000000000 ) ) ;
#18111 = PRODUCT_CONTEXT ( 'NONE', #26899, 'mechanical' ) ;
#18112 = EDGE_CURVE ( 'NONE', #18239, #36735, #2996, .T. ) ;
#18113 = CYLINDRICAL_SURFACE ( 'NONE', #14072, 1.750000000000015765 ) ;
#18114 = AXIS2_PLACEMENT_3D ( 'NONE', #20481, #6433, #8881 ) ;
#18115 = CARTESIAN_POINT ( 'NONE',  ( 36.99999662536855283, -60.62177826491080168, -5.000000000000000000 ) ) ;
#18116 = DIRECTION ( 'NONE',  ( 0.000000000000000000, 0.000000000000000000, 1.000000000000000000 ) ) ;
#18117 = ORIENTED_EDGE ( 'NONE', *, *, #10347, .T. ) ;
#18118 = DIRECTION ( 'NONE',  ( 0.000000000000000000, 0.000000000000000000, 1.000000000000000000 ) ) ;
#18119 = EDGE_CURVE ( 'NONE', #2201, #8255, #29464, .T. ) ;
#18120 = DIRECTION ( 'NONE',  ( 0.000000000000000000, 0.000000000000000000, 1.000000000000000000 ) ) ;
#18121 = CARTESIAN_POINT ( 'NONE',  ( 0.000000000000000000, 0.000000000000000000, -5.974599999999999689 ) ) ;
#18122 = EDGE_CURVE ( 'NONE', #8851, #30126, #7902, .T. ) ;
#18123 = VERTEX_POINT ( 'NONE', #33407 ) ;
#18124 = ORIENTED_EDGE ( 'NONE', *, *, #11240, .F. ) ;
#18125 = AXIS2_PLACEMENT_3D ( 'NONE', #27759, #2074, #19337 ) ;
#18126 = ORIENTED_EDGE ( 'NONE', *, *, #6993, .T. ) ;
#18127 = CIRCLE ( 'NONE', #28900, 33.00000000000001421 ) ;
#18128 = CARTESIAN_POINT ( 'NONE',  ( -45.00000337463111322, 60.62177826491077326, 12.50000000000000000 ) ) ;
#18129 = LINE ( 'NONE', #35223, #17735 ) ;
#18130 = ADVANCED_FACE ( 'NONE', ( #33599 ), #13327, .T. ) ;
#18131 = EDGE_CURVE ( 'NONE', #30229, #25550, #9103, .T. ) ;
#18132 = DIRECTION ( 'NONE',  ( -1.000000000000000000, 0.000000000000000000, 0.000000000000000000 ) ) ;
#18133 = ADVANCED_FACE ( 'NONE', ( #4346 ), #21603, .F. ) ;
#18134 = ADVANCED_FACE ( 'NONE', ( #15970 ), #30758, .F. ) ;
#18135 = CARTESIAN_POINT ( 'NONE',  ( 84.99999662536832545, 8.660254037844394404, -5.000000000000000000 ) ) ;
#18136 = CARTESIAN_POINT ( 'NONE',  ( 52.39915983220795681, 35.19434990244919703, -4.999999999999997335 ) ) ;
#18137 = EDGE_CURVE ( 'NONE', #6640, #2842, #32466, .T. ) ;
#18138 = DIRECTION ( 'NONE',  ( -1.000000000000000000, 0.000000000000000000, 0.000000000000000000 ) ) ;
#18139 = ORIENTED_EDGE ( 'NONE', *, *, #12131, .T. ) ;
#18140 = ORIENTED_EDGE ( 'NONE', *, *, #24105, .T. ) ;
#18141 = AXIS2_PLACEMENT_3D ( 'NONE', #25892, #34523, #21576 ) ;
#18142 = DIRECTION ( 'NONE',  ( 1.000000000000000000, 0.000000000000000000, 0.000000000000000000 ) ) ;
#18143 = DIRECTION ( 'NONE',  ( 0.000000000000000000, 0.000000000000000000, 1.000000000000000000 ) ) ;
#18144 = EDGE_LOOP ( 'NONE', ( #874, #29384, #16264, #9098 ) ) ;
#18145 = CARTESIAN_POINT ( 'NONE',  ( 64.99999662536839651, -60.62177826491080168, -5.000000000000000000 ) ) ;
#18146 = ORIENTED_EDGE ( 'NONE', *, *, #21568, .T. ) ;
#18147 = CARTESIAN_POINT ( 'NONE',  ( -66.86787810013036903, 2.778182860042780700, -4.999999999999997335 ) ) ;
#18148 = VERTEX_POINT ( 'NONE', #27405 ) ;
#18149 = CIRCLE ( 'NONE', #32491, 3.000000000000002665 ) ;
#18150 = ORIENTED_EDGE ( 'NONE', *, *, #3904, .T. ) ;
#18151 = DIRECTION ( 'NONE',  ( 1.000000000000000000, 0.000000000000000000, 0.000000000000000000 ) ) ;
#18152 = ORIENTED_EDGE ( 'NONE', *, *, #26945, .T. ) ;
#18153 =( NAMED_UNIT ( * ) PLANE_ANGLE_UNIT ( ) SI_UNIT ( $, .RADIAN. ) );
#18154 = DIRECTION ( 'NONE',  ( 0.000000000000000000, 0.000000000000000000, -1.000000000000000000 ) ) ;
#18155 = CARTESIAN_POINT ( 'NONE',  ( 66.99999662536839651, -60.62177826491080168, 17.49999999999999645 ) ) ;
#18156 = CARTESIAN_POINT ( 'NONE',  ( -2.775557561562891351E-14, 19.94802294027085310, -11.00000000000000000 ) ) ;
#18157 = ORIENTED_EDGE ( 'NONE', *, *, #2954, .F. ) ;
#18158 = VERTEX_POINT ( 'NONE', #36214 ) ;
#18159 = CIRCLE ( 'NONE', #9157, 2.000000000000001776 ) ;
#18160 = ORIENTED_EDGE ( 'NONE', *, *, #10813, .F. ) ;
#18161 = ORIENTED_EDGE ( 'NONE', *, *, #25158, .F. ) ;
#18162 = AXIS2_PLACEMENT_3D ( 'NONE', #30129, #15143, #21700 ) ;
#18163 = ORIENTED_EDGE ( 'NONE', *, *, #18094, .T. ) ;
#18164 = CARTESIAN_POINT ( 'NONE',  ( 0.000000000000000000, 0.000000000000000000, 32.50000000000000000 ) ) ;
#18165 = DIRECTION ( 'NONE',  ( 1.000000000000000000, -3.554796214472773777E-16, 0.000000000000000000 ) ) ;
#18166 = EDGE_LOOP ( 'NONE', ( #4362, #7315 ) ) ;
#18167 = CARTESIAN_POINT ( 'NONE',  ( 3.000000000000000000, 2.935248768560057453, -3.903127820947815962E-15 ) ) ;
#18168 = CARTESIAN_POINT ( 'NONE',  ( 98.28784258493033121, 106.7731239591685437, 27.50000000000000000 ) ) ;
#18169 = CARTESIAN_POINT ( 'NONE',  ( -40.99999999999999289, -103.4105893997321743, 32.50000000000000000 ) ) ;
#18170 = ORIENTED_EDGE ( 'NONE', *, *, #27137, .F. ) ;
#18171 = CARTESIAN_POINT ( 'NONE',  ( -83.10591231744739105, 8.018055418181152305, -5.000000000000000000 ) ) ;
#18172 = CIRCLE ( 'NONE', #2012, 2.000000000000001776 ) ;
#18173 = CARTESIAN_POINT ( 'NONE',  ( 56.74224907229030634, -68.66839587347224949, -4.999999999999997335 ) ) ;
#18174 = CIRCLE ( 'NONE', #180, 2.000000000000001776 ) ;
#18175 = EDGE_CURVE ( 'NONE', #18010, #22677, #29489, .T. ) ;
#18176 = FACE_OUTER_BOUND ( 'NONE', #21930, .T. ) ;
#18177 = ORIENTED_EDGE ( 'NONE', *, *, #18949, .T. ) ;
#18178 = DIRECTION ( 'NONE',  ( 1.000000000000000000, 0.000000000000000000, 0.000000000000000000 ) ) ;
#18179 = CARTESIAN_POINT ( 'NONE',  ( 24.99999662536859546, -77.94228634059960825, 12.50000000000000000 ) ) ;
#18180 = AXIS2_PLACEMENT_3D ( 'NONE', #17368, #11907, #23369 ) ;
#18181 = ORIENTED_EDGE ( 'NONE', *, *, #4190, .F. ) ;
#18182 = VERTEX_POINT ( 'NONE', #7171 ) ;
#18183 = CARTESIAN_POINT ( 'NONE',  ( 65.00000000000000000, 7.960204194457797252E-15, 17.49999999999999645 ) ) ;
#18184 = DIRECTION ( 'NONE',  ( 0.000000000000000000, 0.000000000000000000, 1.000000000000000000 ) ) ;
#18185 = CARTESIAN_POINT ( 'NONE',  ( -68.00000337463100664, -17.32050807568882078, -5.000000000000000000 ) ) ;
#18186 = CARTESIAN_POINT ( 'NONE',  ( -3.368272016354703968, 101.4480229402710592, -25.00000000000000000 ) ) ;
#18187 = ORIENTED_EDGE ( 'NONE', *, *, #24410, .T. ) ;
#18188 = FACE_BOUND ( 'NONE', #33476, .T. ) ;
#18189 = CARTESIAN_POINT ( 'NONE',  ( -75.00000337463097821, 8.660254037844374864, -9.999999999999998224 ) ) ;
#18190 = CIRCLE ( 'NONE', #22994, 2.000000000000000000 ) ;
#18191 = ORIENTED_EDGE ( 'NONE', *, *, #18273, .F. ) ;
#18192 = DIRECTION ( 'NONE',  ( 0.000000000000000000, 0.000000000000000000, -1.000000000000000000 ) ) ;
#18193 = ORIENTED_EDGE ( 'NONE', *, *, #3879, .F. ) ;
#18194 = EDGE_CURVE ( 'NONE', #13427, #17922, #12955, .T. ) ;
#18195 = CARTESIAN_POINT ( 'NONE',  ( 0.000000000000000000, 0.000000000000000000, 12.49999999999999822 ) ) ;
#18196 = CONICAL_SURFACE ( 'NONE', #854, 5.000000000000000888, 1.047197551196596299 ) ;
#18197 = DIRECTION ( 'NONE',  ( -1.000000000000000000, 0.000000000000000000, 0.000000000000000000 ) ) ;
#18198 = COLOUR_RGB ( '', 0.40784314, 0.44705882, 0.49803922) ;
#18199 = CARTESIAN_POINT ( 'NONE',  ( 3.101151694651712809, 3.983051926191225611, -0.6020238742160355372 ) ) ;
#18200 = ORIENTED_EDGE ( 'NONE', *, *, #30380, .F. ) ;
#18201 = VERTEX_POINT ( 'NONE', #9964 ) ;
#18202 = DIRECTION ( 'NONE',  ( 1.000000000000000000, 0.000000000000000000, 0.000000000000000000 ) ) ;
#18203 = ORIENTED_EDGE ( 'NONE', *, *, #22250, .F. ) ;
#18204 = CARTESIAN_POINT ( 'NONE',  ( 9.999996625368655856, -86.60254037844400443, -9.999999999999998224 ) ) ;
#18205 = FACE_BOUND ( 'NONE', #16043, .T. ) ;
#18206 = DIRECTION ( 'NONE',  ( 0.000000000000000000, 0.000000000000000000, -1.000000000000000000 ) ) ;
#18207 = CARTESIAN_POINT ( 'NONE',  ( -70.00000337463102085, -51.96152422706641971, -9.999999999999998224 ) ) ;
#18208 = LINE ( 'NONE', #23862, #8130 ) ;
#18209 = EDGE_LOOP ( 'NONE', ( #26686, #32554 ) ) ;
#18210 = CARTESIAN_POINT ( 'NONE',  ( -55.27226924886021919, 77.26562141134635908, 27.50000000000000000 ) ) ;
#18211 = CIRCLE ( 'NONE', #6225, 3.500000000000003109 ) ;
#18212 = CARTESIAN_POINT ( 'NONE',  ( -3.499999999999987566, -55.00000000000000000, -10.00000000000000178 ) ) ;
#18213 = EDGE_CURVE ( 'NONE', #23401, #21975, #30400, .T. ) ;
#18214 = FACE_OUTER_BOUND ( 'NONE', #9200, .T. ) ;
#18215 = ORIENTED_EDGE ( 'NONE', *, *, #33218, .T. ) ;
#18216 = CARTESIAN_POINT ( 'NONE',  ( 86.99999662536831124, -25.98076211353319565, -9.999999999999998224 ) ) ;
#18217 = CARTESIAN_POINT ( 'NONE',  ( -6.216324218022825094E-15, 6.066067634115565710, -4.359491423763658169 ) ) ;
#18218 = DIRECTION ( 'NONE',  ( 1.000000000000000000, 0.000000000000000000, 0.000000000000000000 ) ) ;
#18219 = VECTOR ( 'NONE', #24551, 1000.000000000000000 ) ;
#18220 = ORIENTED_EDGE ( 'NONE', *, *, #26953, .T. ) ;
#18221 = VECTOR ( 'NONE', #31292, 1000.000000000000000 ) ;
#18222 = VERTEX_POINT ( 'NONE', #27199 ) ;
#18223 = AXIS2_PLACEMENT_3D ( 'NONE', #34329, #14068, #31494 ) ;
#18224 = DIRECTION ( 'NONE',  ( 0.000000000000000000, 0.000000000000000000, 1.000000000000000000 ) ) ;
#18225 = DIRECTION ( 'NONE',  ( 1.000000000000000000, 0.000000000000000000, 0.000000000000000000 ) ) ;
#18226 = DIRECTION ( 'NONE',  ( 1.000000000000000000, 0.000000000000000000, 0.000000000000000000 ) ) ;
#18227 = ORIENTED_EDGE ( 'NONE', *, *, #1295, .T. ) ;
#18228 = VERTEX_POINT ( 'NONE', #24416 ) ;
#18229 = ORIENTED_EDGE ( 'NONE', *, *, #11475, .T. ) ;
#18230 = CARTESIAN_POINT ( 'NONE',  ( 66.00000000000000000, 3.334407072378456173E-16, -2.445500000000000007 ) ) ;
#18231 = AXIS2_PLACEMENT_3D ( 'NONE', #32854, #21211, #24615 ) ;
#18232 = ORIENTED_EDGE ( 'NONE', *, *, #31674, .F. ) ;
#18233 = EDGE_CURVE ( 'NONE', #24614, #28371, #33029, .T. ) ;
#18234 = AXIS2_PLACEMENT_3D ( 'NONE', #28852, #20427, #31838 ) ;
#18235 = ORIENTED_EDGE ( 'NONE', *, *, #24026, .T. ) ;
#18236 = LINE ( 'NONE', #4000, #5821 ) ;
#18237 = VERTEX_POINT ( 'NONE', #19711 ) ;
#18238 = EDGE_CURVE ( 'NONE', #8351, #26162, #24724, .T. ) ;
#18239 = VERTEX_POINT ( 'NONE', #2464 ) ;
#18240 = AXIS2_PLACEMENT_3D ( 'NONE', #34172, #16902, #31501 ) ;
#18241 = CARTESIAN_POINT ( 'NONE',  ( -18.00000337463123756, -69.28203230275522628, -9.999999999999998224 ) ) ;
#18242 = CYLINDRICAL_SURFACE ( 'NONE', #27240, 2.000000000000001776 ) ;
#18243 = ORIENTED_EDGE ( 'NONE', *, *, #16762, .T. ) ;
#18244 = EDGE_CURVE ( 'NONE', #33756, #14593, #31683, .T. ) ;
#18245 = ORIENTED_EDGE ( 'NONE', *, *, #31331, .F. ) ;
#18246 = FACE_OUTER_BOUND ( 'NONE', #15597, .T. ) ;
#18247 = DIRECTION ( 'NONE',  ( -1.000000000000000000, -0.000000000000000000, -0.000000000000000000 ) ) ;
#18248 = CIRCLE ( 'NONE', #13455, 2.000000000000001776 ) ;
#18249 = CARTESIAN_POINT ( 'NONE',  ( 1.999996625368696490, -86.60254037844400443, 17.49999999999999645 ) ) ;
#18250 = CIRCLE ( 'NONE', #23043, 95.00000000000001421 ) ;
#18251 = DIRECTION ( 'NONE',  ( 0.000000000000000000, 0.000000000000000000, 1.000000000000000000 ) ) ;
#18252 = VECTOR ( 'NONE', #13986, 1000.000000000000000 ) ;
#18253 = EDGE_CURVE ( 'NONE', #13437, #13179, #2560, .T. ) ;
#18254 = ORIENTED_EDGE ( 'NONE', *, *, #19242, .F. ) ;
#18255 = CARTESIAN_POINT ( 'NONE',  ( -47.63139720814438505, -27.49999999999955591, -5.000000000000000000 ) ) ;
#18256 = FACE_OUTER_BOUND ( 'NONE', #10032, .T. ) ;
#18257 = VERTEX_POINT ( 'NONE', #6018 ) ;
#18258 = DIRECTION ( 'NONE',  ( 0.000000000000000000, 0.000000000000000000, 1.000000000000000000 ) ) ;
#18259 = CARTESIAN_POINT ( 'NONE',  ( 58.88972745734226066, 33.99999999999924682, -49.86561046011506448 ) ) ;
#18260 = DIRECTION ( 'NONE',  ( 0.000000000000000000, 0.000000000000000000, 1.000000000000000000 ) ) ;
#18261 = CARTESIAN_POINT ( 'NONE',  ( -72.00000337463100664, 17.32050807568877460, -9.999999999999998224 ) ) ;
#18262 = DIRECTION ( 'NONE',  ( 1.000000000000000000, 0.000000000000000000, 0.000000000000000000 ) ) ;
#18263 = CIRCLE ( 'NONE', #23030, 3.000000000000002665 ) ;
#18264 = CYLINDRICAL_SURFACE ( 'NONE', #33716, 8.500000000000000000 ) ;
#18265 = ORIENTED_EDGE ( 'NONE', *, *, #2455, .F. ) ;
#18267 = AXIS2_PLACEMENT_3D ( 'NONE', #6824, #12242, #6100 ) ;
#18266 = CARTESIAN_POINT ( 'NONE',  ( -25.00000337463120914, 77.94228634059957983, -5.000000000000000000 ) ) ;
#18268 = LINE ( 'NONE', #21826, #36302 ) ;
#18269 = LINE ( 'NONE', #6833, #21718 ) ;
#18270 = CIRCLE ( 'NONE', #9299, 2.000000000000001776 ) ;
#18271 = ORIENTED_EDGE ( 'NONE', *, *, #44, .F. ) ;
#18272 = AXIS2_PLACEMENT_3D ( 'NONE', #890, #20766, #23974 ) ;
#18273 = EDGE_CURVE ( 'NONE', #11585, #30663, #33089, .T. ) ;
#18274 = ORIENTED_EDGE ( 'NONE', *, *, #9881, .T. ) ;
#18275 = EDGE_LOOP ( 'NONE', ( #25363, #9095 ) ) ;
#18276 = CARTESIAN_POINT ( 'NONE',  ( 34.46585318596250858, 86.45172111230321832, -4.999999999999997335 ) ) ;
#18277 = PLANE ( 'NONE',  #5276 ) ;
#18278 = CARTESIAN_POINT ( 'NONE',  ( 56.74224907229030634, -68.66839587347224949, 12.49999999999999645 ) ) ;
#18279 = VECTOR ( 'NONE', #11915, 1000.000000000000000 ) ;
#18280 = AXIS2_PLACEMENT_3D ( 'NONE', #25238, #8364, #33850 ) ;
#18281 = ADVANCED_FACE ( 'NONE', ( #14444 ), #22328, .F. ) ;
#18282 = CIRCLE ( 'NONE', #2116, 27.00000000000001421 ) ;
#18283 = FACE_OUTER_BOUND ( 'NONE', #23592, .T. ) ;
#18284 = FACE_OUTER_BOUND ( 'NONE', #16783, .T. ) ;
#18285 = ORIENTED_EDGE ( 'NONE', *, *, #15967, .F. ) ;
#18286 = ADVANCED_FACE ( 'NONE', ( #25878 ), #36959, .F. ) ;
#18287 =( REPRESENTATION_RELATIONSHIP ('NONE','NONE', #15268, #22738 ) REPRESENTATION_RELATIONSHIP_WITH_TRANSFORMATION ( #10964 )SHAPE_REPRESENTATION_RELATIONSHIP( ) );
#18288 = DIRECTION ( 'NONE',  ( 1.000000000000000000, 0.000000000000000000, 0.000000000000000000 ) ) ;
#18289 = ORIENTED_EDGE ( 'NONE', *, *, #29591, .T. ) ;
#18290 = FACE_BOUND ( 'NONE', #2543, .T. ) ;
#18291 = DIRECTION ( 'NONE',  ( 0.000000000000000000, 0.000000000000000000, 1.000000000000000000 ) ) ;
#18292 = CARTESIAN_POINT ( 'NONE',  ( -145.0000000000001137, -5.999999999998481215, 32.55002500000000509 ) ) ;
#18293 = AXIS2_PLACEMENT_3D ( 'NONE', #19964, #36841, #34051 ) ;
#18294 = LINE ( 'NONE', #35564, #34969 ) ;
#18295 = AXIS2_PLACEMENT_3D ( 'NONE', #17316, #7945, #20111 ) ;
#18296 = EDGE_LOOP ( 'NONE', ( #25665, #27867, #35977, #22804 ) ) ;
#18297 = CARTESIAN_POINT ( 'NONE',  ( 5.000000000000000000, 1.947085426416884202, -5.800379292880308846 ) ) ;
#18298 = CIRCLE ( 'NONE', #12911, 3.000000000000002665 ) ;
#18299 = AXIS2_PLACEMENT_3D ( 'NONE', #20084, #25900, #5651 ) ;
#18300 = CARTESIAN_POINT ( 'NONE',  ( -47.63139720814399425, -27.50000000000022382, -16.00000000000000000 ) ) ;
#18301 = AXIS2_PLACEMENT_3D ( 'NONE', #9842, #23738, #7048 ) ;
#18302 = CIRCLE ( 'NONE', #33270, 2.000000000000001776 ) ;
#18303 = LINE ( 'NONE', #24303, #33278 ) ;
#18304 = EDGE_CURVE ( 'NONE', #17144, #3455, #34303, .T. ) ;
#18305 = DIRECTION ( 'NONE',  ( 0.000000000000000000, 0.000000000000000000, 1.000000000000000000 ) ) ;
#18306 = LINE ( 'NONE', #29733, #9541 ) ;
#18307 = EDGE_LOOP ( 'NONE', ( #15272, #16208, #37025 ) ) ;
#18308 = CARTESIAN_POINT ( 'NONE',  ( 0.000000000000000000, 0.000000000000000000, 27.50000000000000000 ) ) ;
#18309 = DIRECTION ( 'NONE',  ( -0.000000000000000000, -0.000000000000000000, -1.000000000000000000 ) ) ;
#18310 = DIRECTION ( 'NONE',  ( 0.000000000000000000, 0.000000000000000000, 1.000000000000000000 ) ) ;
#18311 = CIRCLE ( 'NONE', #3346, 95.00000000000000000 ) ;
#18312 = EDGE_LOOP ( 'NONE', ( #6679, #7020 ) ) ;
#18313 = ORIENTED_EDGE ( 'NONE', *, *, #29941, .F. ) ;
#18314 = ORIENTED_EDGE ( 'NONE', *, *, #29752, .T. ) ;
#18315 = CARTESIAN_POINT ( 'NONE',  ( -72.00000337463100664, -17.32050807568882078, -9.999999999999998224 ) ) ;
#18316 = CARTESIAN_POINT ( 'NONE',  ( 17.99999662536858125, 86.60254037844397601, -9.999999999999998224 ) ) ;
#18317 = AXIS2_PLACEMENT_3D ( 'NONE', #22604, #19418, #31043 ) ;
#18318 = DIRECTION ( 'NONE',  ( 0.000000000000000000, 0.000000000000000000, 1.000000000000000000 ) ) ;
#18319 = EDGE_CURVE ( 'NONE', #20996, #35319, #18726, .T. ) ;
#18320 = CIRCLE ( 'NONE', #10533, 27.00000000000001421 ) ;
#18321 = CARTESIAN_POINT ( 'NONE',  ( 0.000000000000000000, 55.00000000000000000, -10.00000000000000000 ) ) ;
#18322 = CARTESIAN_POINT ( 'NONE',  ( -40.00000337463113453, 69.28203230275516944, 12.50000000000000000 ) ) ;
#18323 = EDGE_CURVE ( 'NONE', #14606, #35117, #133, .T. ) ;
#18324 = AXIS2_PLACEMENT_3D ( 'NONE', #25334, #5289, #27763 ) ;
#18325 = CIRCLE ( 'NONE', #2161, 2.000000000000001776 ) ;
#18326 = CARTESIAN_POINT ( 'NONE',  ( -42.97377950131527058, 96.90768712682508124, -19.99999999999999645 ) ) ;
#18327 = CONICAL_SURFACE ( 'NONE', #6953, 2.541999999999999815, 1.047197551196591858 ) ;
#18328 = ORIENTED_EDGE ( 'NONE', *, *, #12498, .F. ) ;
#18329 = ADVANCED_FACE ( 'NONE', ( #25169 ), #20257, .F. ) ;
#18330 = CIRCLE ( 'NONE', #30903, 2.000000000000001776 ) ;
#18331 = ORIENTED_EDGE ( 'NONE', *, *, #3671, .F. ) ;
#18332 = FACE_OUTER_BOUND ( 'NONE', #5997, .T. ) ;
#18333 = CARTESIAN_POINT ( 'NONE',  ( -2.374207310413330682E-13, -68.00000000000000000, -4.999999999999997335 ) ) ;
#18334 = ORIENTED_EDGE ( 'NONE', *, *, #28412, .T. ) ;
#18335 = EDGE_CURVE ( 'NONE', #792, #35451, #11440, .T. ) ;
#18336 = DIRECTION ( 'NONE',  ( 0.000000000000000000, 0.000000000000000000, 1.000000000000000000 ) ) ;
#18337 = EDGE_CURVE ( 'NONE', #36783, #19009, #1345, .T. ) ;
#18338 = ORIENTED_EDGE ( 'NONE', *, *, #12176, .T. ) ;
#18339 = FACE_OUTER_BOUND ( 'NONE', #791, .T. ) ;
#18340 = EDGE_CURVE ( 'NONE', #32462, #25777, #21101, .T. ) ;
#18341 = AXIS2_PLACEMENT_3D ( 'NONE', #34726, #2859, #20445 ) ;
#18342 = DIRECTION ( 'NONE',  ( 0.000000000000000000, 0.000000000000000000, 1.000000000000000000 ) ) ;
#18343 = VERTEX_POINT ( 'NONE', #25330 ) ;
#18344 = EDGE_LOOP ( 'NONE', ( #26486, #20439 ) ) ;
#18345 = CARTESIAN_POINT ( 'NONE',  ( -5.000000000000000000, 24.49489742783178414, -15.00000000000000000 ) ) ;
#18346 = ORIENTED_EDGE ( 'NONE', *, *, #419, .T. ) ;
#18347 = EDGE_CURVE ( 'NONE', #26170, #7831, #11067, .T. ) ;
#18348 =( LENGTH_UNIT ( ) NAMED_UNIT ( * ) SI_UNIT ( .MILLI., .METRE. ) );
#18349 = AXIS2_PLACEMENT_3D ( 'NONE', #22198, #36633, #33635 ) ;
#18350 = EDGE_CURVE ( 'NONE', #2100, #25853, #35491, .T. ) ;
#18351 = CARTESIAN_POINT ( 'NONE',  ( -2.931639317407897849, 4.080919942823912017, -0.01465562841807576538 ) ) ;
#18352 = ADVANCED_FACE ( 'NONE', ( #14061 ), #17270, .F. ) ;
#18353 = CIRCLE ( 'NONE', #29713, 3.499999999999996003 ) ;
#18354 = DIRECTION ( 'NONE',  ( 0.000000000000000000, 0.000000000000000000, 1.000000000000000000 ) ) ;
#18355 = CARTESIAN_POINT ( 'NONE',  ( -25.00000337463120914, 77.94228634059957983, 17.49999999999999645 ) ) ;
#18356 = ORIENTED_EDGE ( 'NONE', *, *, #34788, .T. ) ;
#18357 = ORIENTED_EDGE ( 'NONE', *, *, #33232, .T. ) ;
#18358 = AXIS2_PLACEMENT_3D ( 'NONE', #18300, #15302, #6507 ) ;
#18359 = VECTOR ( 'NONE', #23701, 1000.000000000000000 ) ;
#18360 = VERTEX_POINT ( 'NONE', #28695 ) ;
#18361 = VECTOR ( 'NONE', #33117, 1000.000000000000000 ) ;
#18362 = AXIS2_PLACEMENT_3D ( 'NONE', #9223, #20656, #20311 ) ;
#18363 = ORIENTED_EDGE ( 'NONE', *, *, #20778, .T. ) ;
#18364 = ORIENTED_EDGE ( 'NONE', *, *, #8629, .T. ) ;
#18365 = CARTESIAN_POINT ( 'NONE',  ( -58.00000337463104216, 51.96152422706639129, -9.999999999999998224 ) ) ;
#18366 = DIRECTION ( 'NONE',  ( -0.000000000000000000, -0.000000000000000000, 1.000000000000000000 ) ) ;
#18367 = EDGE_LOOP ( 'NONE', ( #560, #1240 ) ) ;
#18368 = CARTESIAN_POINT ( 'NONE',  ( -22.00000337463124112, -69.28203230275522628, -5.000000000000000000 ) ) ;
#18369 = LINE ( 'NONE', #15365, #3144 ) ;
#18370 = CYLINDRICAL_SURFACE ( 'NONE', #26756, 2.000000000000001776 ) ;
#18371 = ORIENTED_EDGE ( 'NONE', *, *, #8860, .T. ) ;
#18372 = CARTESIAN_POINT ( 'NONE',  ( -33.99999999999945288, 58.88972745734214698, -4.999999999999997335 ) ) ;
#18373 = AXIS2_PLACEMENT_3D ( 'NONE', #17505, #31751, #12046 ) ;
#18374 = DIRECTION ( 'NONE',  ( 1.000000000000000000, 0.000000000000000000, 0.000000000000000000 ) ) ;
#18375 = EDGE_CURVE ( 'NONE', #19982, #755, #31289, .T. ) ;
#18376 = CARTESIAN_POINT ( 'NONE',  ( 4.897544501024384282E-15, 69.94802294027087441, 27.49999999999999645 ) ) ;
#18377 = ORIENTED_EDGE ( 'NONE', *, *, #24172, .T. ) ;
#18378 = DIRECTION ( 'NONE',  ( 0.000000000000000000, 0.000000000000000000, -1.000000000000000000 ) ) ;
#18379 = EDGE_CURVE ( 'NONE', #3118, #25301, #29423, .T. ) ;
#18380 = DIRECTION ( 'NONE',  ( 1.000000000000000000, 0.000000000000000000, 0.000000000000000000 ) ) ;
#18381 = ORIENTED_EDGE ( 'NONE', *, *, #34354, .F. ) ;
#18382 = CIRCLE ( 'NONE', #32746, 33.00000000000001421 ) ;
#18383 = VERTEX_POINT ( 'NONE', #18168 ) ;
#18384 = LINE ( 'NONE', #18183, #13445 ) ;
#18385 = AXIS2_PLACEMENT_3D ( 'NONE', #1301, #10477, #21171 ) ;
#18386 = CLOSED_SHELL ( 'NONE', ( #25004, #17108, #26279, #20220, #12484, #35257, #10769, #20408, #32840, #12571, #19049, #34487, #18011, #1890, #31167, #2607, #566, #21342, #20529, #8958, #30914, #5474, #34146, #31853 ) ) ;
#18387 = CARTESIAN_POINT ( 'NONE',  ( -61.53067111003215217, 72.28378166042038799, -49.22241343995295892 ) ) ;
#18388 = DIRECTION ( 'NONE',  ( 1.000000000000000000, 0.000000000000000000, 0.000000000000000000 ) ) ;
#18389 = DIRECTION ( 'NONE',  ( -1.000000000000000000, 0.000000000000000000, 0.000000000000000000 ) ) ;
#18390 = EDGE_CURVE ( 'NONE', #35025, #1395, #31859, .T. ) ;
#18391 = ORIENTED_EDGE ( 'NONE', *, *, #10566, .F. ) ;
#18392 = ORIENTED_EDGE ( 'NONE', *, *, #31869, .F. ) ;
#18394 = AXIS2_PLACEMENT_3D ( 'NONE', #21, #11449, #22894 ) ;
#18393 = DIRECTION ( 'NONE',  ( 1.000000000000000000, 0.000000000000000000, 0.000000000000000000 ) ) ;
#18395 = DIRECTION ( 'NONE',  ( 0.000000000000000000, 0.000000000000000000, 1.000000000000000000 ) ) ;
#18396 = AXIS2_PLACEMENT_3D ( 'NONE', #5451, #33948, #28297 ) ;
#18397 = CIRCLE ( 'NONE', #2226, 2.000000000000000000 ) ;
#18398 = ORIENTED_EDGE ( 'NONE', *, *, #5215, .T. ) ;
#18399 = CARTESIAN_POINT ( 'NONE',  ( -67.00000337463104927, -43.30127018922202353, -5.000000000000000000 ) ) ;
#18400 = ORIENTED_EDGE ( 'NONE', *, *, #31062, .T. ) ;
#18401 = EDGE_CURVE ( 'NONE', #6597, #22278, #15129, .T. ) ;
#18402 = CARTESIAN_POINT ( 'NONE',  ( 41.99999662536853151, -69.28203230275519786, -9.999999999999998224 ) ) ;
#18403 = AXIS2_PLACEMENT_3D ( 'NONE', #8843, #8652, #202 ) ;
#18404 = EDGE_CURVE ( 'NONE', #16311, #20316, #19321, .T. ) ;
#18405 = LINE ( 'NONE', #29833, #9225 ) ;
#18406 = EDGE_CURVE ( 'NONE', #460, #30149, #28398, .T. ) ;
#18407 = DIRECTION ( 'NONE',  ( 0.000000000000000000, 0.000000000000000000, -1.000000000000000000 ) ) ;
#18408 = EDGE_CURVE ( 'NONE', #7069, #6161, #18369, .T. ) ;
#18409 = VERTEX_POINT ( 'NONE', #26809 ) ;
#18410 = ORIENTED_EDGE ( 'NONE', *, *, #3690, .F. ) ;
#18411 = AXIS2_PLACEMENT_3D ( 'NONE', #18259, #29691, #15265 ) ;
#18412 = AXIS2_PLACEMENT_3D ( 'NONE', #27894, #19463, #17214 ) ;
#18413 = VECTOR ( 'NONE', #12642, 1000.000000000000000 ) ;
#18414 = ORIENTED_EDGE ( 'NONE', *, *, #246, .F. ) ;
#18415 = CARTESIAN_POINT ( 'NONE',  ( 76.99999662536836809, 43.30127018922198801, -9.999999999999998224 ) ) ;
#18416 = FACE_OUTER_BOUND ( 'NONE', #2487, .T. ) ;
#18417 = DIRECTION ( 'NONE',  ( 1.000000000000000000, 0.000000000000000000, 0.000000000000000000 ) ) ;
#18418 = FACE_OUTER_BOUND ( 'NONE', #28509, .T. ) ;
#18419 = CARTESIAN_POINT ( 'NONE',  ( -31.74999999999995737, 6.123233995736766282E-16, -5.000000000000000000 ) ) ;
#18420 = EDGE_LOOP ( 'NONE', ( #4546, #27620 ) ) ;
#18421 = CYLINDRICAL_SURFACE ( 'NONE', #12301, 2.000000000000001776 ) ;
#18422 = CIRCLE ( 'NONE', #29191, 2.000000000000001776 ) ;
#18423 = CIRCLE ( 'NONE', #24420, 2.000000000000001776 ) ;
#18424 = DIRECTION ( 'NONE',  ( -0.8191520442889913545, 0.000000000000000000, -0.5735764363510468256 ) ) ;
#18425 = SURFACE_STYLE_USAGE ( .BOTH. , #4179 ) ;
#18426 = EDGE_LOOP ( 'NONE', ( #8552, #14295, #12106, #3348, #342 ) ) ;
#18427 = CARTESIAN_POINT ( 'NONE',  ( 35.19434990244975126, -52.39915983220758022, -4.999999999999997335 ) ) ;
#18428 = FACE_BOUND ( 'NONE', #10670, .T. ) ;
#18429 = LINE ( 'NONE', #32472, #7825 ) ;
#18430 = VECTOR ( 'NONE', #6472, 1000.000000000000000 ) ;
#18431 = ADVANCED_FACE ( 'NONE', ( #9365 ), #14613, .F. ) ;
#18432 = ORIENTED_EDGE ( 'NONE', *, *, #26539, .F. ) ;
#18433 = EDGE_LOOP ( 'NONE', ( #8147, #3349 ) ) ;
#18434 = AXIS2_PLACEMENT_3D ( 'NONE', #7918, #15992, #36056 ) ;
#18435 = DIRECTION ( 'NONE',  ( 1.000000000000000000, 0.000000000000000000, 0.000000000000000000 ) ) ;
#18436 = CARTESIAN_POINT ( 'NONE',  ( -50.00000337463109190, 69.28203230275518365, -9.999999999999998224 ) ) ;
#18437 = DIRECTION ( 'NONE',  ( 0.000000000000000000, 0.000000000000000000, 1.000000000000000000 ) ) ;
#18438 = ORIENTED_EDGE ( 'NONE', *, *, #6465, .F. ) ;
#18439 = EDGE_LOOP ( 'NONE', ( #27234, #18802 ) ) ;
#18440 = CIRCLE ( 'NONE', #2267, 2.000000000000001776 ) ;
#18441 = AXIS2_PLACEMENT_3D ( 'NONE', #33406, #10519, #30589 ) ;
#18442 = EDGE_LOOP ( 'NONE', ( #25114, #20061 ) ) ;
#18443 = CIRCLE ( 'NONE', #1682, 2.000000000000000000 ) ;
#18444 = CARTESIAN_POINT ( 'NONE',  ( -75.00000337463097821, 25.98076211353318854, -9.999999999999998224 ) ) ;
#18445 = CIRCLE ( 'NONE', #26815, 3.000000000000002665 ) ;
#18446 = VERTEX_POINT ( 'NONE', #361 ) ;
#18447 = ORIENTED_EDGE ( 'NONE', *, *, #329, .F. ) ;
#18448 = DIRECTION ( 'NONE',  ( 0.000000000000000000, 0.000000000000000000, 1.000000000000000000 ) ) ;
#18449 = ORIENTED_EDGE ( 'NONE', *, *, #14017, .F. ) ;
#18450 = ORIENTED_EDGE ( 'NONE', *, *, #18379, .F. ) ;
#18451 = CIRCLE ( 'NONE', #2905, 45.00000000000000711 ) ;
#18452 = DIRECTION ( 'NONE',  ( 1.000000000000000000, 0.000000000000000000, -0.000000000000000000 ) ) ;
#18453 = DIRECTION ( 'NONE',  ( 1.000000000000000000, 0.000000000000000000, 0.000000000000000000 ) ) ;
#18454 = ADVANCED_FACE ( 'NONE', ( #11796 ), #23255, .T. ) ;
#18455 = ORIENTED_EDGE ( 'NONE', *, *, #7657, .T. ) ;
#18456 = ORIENTED_EDGE ( 'NONE', *, *, #17465, .T. ) ;
#18457 = CARTESIAN_POINT ( 'NONE',  ( -78.00000337463094979, 34.64101615137757051, -5.000000000000000000 ) ) ;
#18458 = AXIS2_PLACEMENT_3D ( 'NONE', #25115, #31260, #34276 ) ;
#18459 = CARTESIAN_POINT ( 'NONE',  ( 56.99999662536846046, -43.30127018922200222, -9.999999999999998224 ) ) ;
#18460 = CARTESIAN_POINT ( 'NONE',  ( 0.000000000000000000, 0.000000000000000000, 15.00000000000000000 ) ) ;
#18461 = CARTESIAN_POINT ( 'NONE',  ( 34.99999662536855283, -77.94228634059960825, -5.000000000000000000 ) ) ;
#18462 = VERTEX_POINT ( 'NONE', #20430 ) ;
#18463 = FACE_OUTER_BOUND ( 'NONE', #28933, .T. ) ;
#18464 = CIRCLE ( 'NONE', #1080, 30.00000000000000000 ) ;
#18465 = VERTEX_POINT ( 'NONE', #1474 ) ;
#18466 = CYLINDRICAL_SURFACE ( 'NONE', #22151, 2.000000000000000000 ) ;
#18467 = CIRCLE ( 'NONE', #30423, 2.000000000000001776 ) ;
#18468 = VECTOR ( 'NONE', #24779, 1000.000000000000000 ) ;
#18469 = CARTESIAN_POINT ( 'NONE',  ( 6.000000000000000000, -149.8799519615616305, 27.50000000000000000 ) ) ;
#18470 = CARTESIAN_POINT ( 'NONE',  ( 0.000000000000000000, 55.00000000000000000, -15.00000000000000000 ) ) ;
#18472 = CIRCLE ( 'NONE', #22059, 2.000000000000001776 ) ;
#18471 = DIRECTION ( 'NONE',  ( 1.000000000000000000, 0.000000000000000000, 0.000000000000000000 ) ) ;
#18473 = DIRECTION ( 'NONE',  ( -1.051347561198064495E-14, -1.000000000000000000, 0.000000000000000000 ) ) ;
#18474 = VECTOR ( 'NONE', #36603, 1000.000000000000000 ) ;
#18475 = DIRECTION ( 'NONE',  ( -0.000000000000000000, -0.000000000000000000, 1.000000000000000000 ) ) ;
#18476 = ORIENTED_EDGE ( 'NONE', *, *, #11798, .F. ) ;
#18477 = CARTESIAN_POINT ( 'NONE',  ( 34.99999662536853862, 77.94228634059959404, -9.999999999999998224 ) ) ;
#18478 = CARTESIAN_POINT ( 'NONE',  ( -80.00000337463094979, -2.428612866367529932E-14, 17.49999999999999645 ) ) ;
#18479 = CARTESIAN_POINT ( 'NONE',  ( -45.00000337463111322, 60.62177826491077326, -9.999999999999998224 ) ) ;
#18480 = EDGE_CURVE ( 'NONE', #7831, #13768, #18099, .T. ) ;
#18481 = EDGE_LOOP ( 'NONE', ( #13876, #1509, #32130, #30081 ) ) ;
#18482 = CIRCLE ( 'NONE', #32241, 33.00000000000001421 ) ;
#18483 = VERTEX_POINT ( 'NONE', #18923 ) ;
#18484 = ORIENTED_EDGE ( 'NONE', *, *, #27040, .F. ) ;
#18485 = DIRECTION ( 'NONE',  ( -1.000000000000000000, 0.000000000000000000, 0.000000000000000000 ) ) ;
#18486 = DIRECTION ( 'NONE',  ( -1.000000000000000000, 0.000000000000000000, -0.000000000000000000 ) ) ;
#18487 = DIRECTION ( 'NONE',  ( -1.000000000000000000, 0.000000000000000000, 0.000000000000000000 ) ) ;
#18488 = EDGE_CURVE ( 'NONE', #5388, #12428, #15724, .T. ) ;
#18489 = VERTEX_POINT ( 'NONE', #21728 ) ;
#18490 = CIRCLE ( 'NONE', #13064, 2.000000000000001776 ) ;
#18491 = PRODUCT_DEFINITION_SHAPE ( 'NONE', 'NONE',  #37114 ) ;
#18492 = CARTESIAN_POINT ( 'NONE',  ( -10.00000337463128730, 69.28203230275516944, -9.999999999999998224 ) ) ;
#18493 = EDGE_CURVE ( 'NONE', #2053, #29771, #9722, .T. ) ;
#18494 = DIRECTION ( 'NONE',  ( -0.000000000000000000, 0.000000000000000000, 1.000000000000000000 ) ) ;
#18495 = ORIENTED_EDGE ( 'NONE', *, *, #29786, .T. ) ;
#18496 = CARTESIAN_POINT ( 'NONE',  ( 44.13139720814420031, 27.49999999999988987, -10.00000000000000000 ) ) ;
#18497 = ORIENTED_EDGE ( 'NONE', *, *, #3650, .F. ) ;
#18498 = CIRCLE ( 'NONE', #6521, 2.000000000000001776 ) ;
#18499 = CARTESIAN_POINT ( 'NONE',  ( 76.99999662536836809, 43.30127018922198801, 17.49999999999999645 ) ) ;
#18500 = CARTESIAN_POINT ( 'NONE',  ( -33.00000337463116296, -60.62177826491080168, -9.999999999999998224 ) ) ;
#18501 = AXIS2_PLACEMENT_3D ( 'NONE', #12299, #9134, #14577 ) ;
#18502 = CARTESIAN_POINT ( 'NONE',  ( -47.63139720814438505, -27.49999999999955591, 5.000000000000000888 ) ) ;
#18503 = AXIS2_PLACEMENT_3D ( 'NONE', #30045, #15440, #35881 ) ;
#18504 = DIRECTION ( 'NONE',  ( 0.000000000000000000, 0.000000000000000000, 1.000000000000000000 ) ) ;
#18505 = EDGE_CURVE ( 'NONE', #3218, #34714, #22312, .T. ) ;
#18506 = ORIENTED_EDGE ( 'NONE', *, *, #36596, .T. ) ;
#18507 = LINE ( 'NONE', #24861, #29653 ) ;
#18508 = AXIS2_PLACEMENT_3D ( 'NONE', #14587, #34297, #20233 ) ;
#18509 = DIRECTION ( 'NONE',  ( 0.000000000000000000, 0.000000000000000000, -1.000000000000000000 ) ) ;
#18510 = VECTOR ( 'NONE', #29279, 1000.000000000000000 ) ;
#18511 = CARTESIAN_POINT ( 'NONE',  ( 0.000000000000000000, 0.000000000000000000, 12.49999999999999822 ) ) ;
#18512 = CYLINDRICAL_SURFACE ( 'NONE', #31113, 2.000000000000001776 ) ;
#18513 = ORIENTED_EDGE ( 'NONE', *, *, #11690, .T. ) ;
#18514 = CARTESIAN_POINT ( 'NONE',  ( 84.99999662536832545, 8.660254037844394404, -9.999999999999998224 ) ) ;
#18515 = DIRECTION ( 'NONE',  ( 1.000000000000000000, 0.000000000000000000, 0.000000000000000000 ) ) ;
#18516 = LINE ( 'NONE', #4440, #4617 ) ;
#18517 = ADVANCED_FACE ( 'NONE', ( #27716 ), #24739, .T. ) ;
#18518 = VERTEX_POINT ( 'NONE', #16127 ) ;
#18519 = CIRCLE ( 'NONE', #14926, 2.000000000000000000 ) ;
#18520 = ADVANCED_FACE ( 'NONE', ( #2034 ), #34892, .F. ) ;
#18521 = ORIENTED_EDGE ( 'NONE', *, *, #32773, .F. ) ;
#18522 = AXIS2_PLACEMENT_3D ( 'NONE', #12531, #28537, #2874 ) ;
#18523 = CARTESIAN_POINT ( 'NONE',  ( -5.000000000000000888, 2.886751345948107783, -5.700000000000000178 ) ) ;
#18524 = CARTESIAN_POINT ( 'NONE',  ( -77.00000337463097821, 43.30127018922197379, -5.000000000000000000 ) ) ;
#18525 = FACE_OUTER_BOUND ( 'NONE', #4923, .T. ) ;
#18526 = EDGE_LOOP ( 'NONE', ( #6537, #36552 ) ) ;
#18527 = AXIS2_PLACEMENT_3D ( 'NONE', #4606, #12262, #18098 ) ;
#18528 = DIRECTION ( 'NONE',  ( -0.000000000000000000, -0.000000000000000000, 1.000000000000000000 ) ) ;
#18529 = DIRECTION ( 'NONE',  ( 0.000000000000000000, 0.4999999999999959477, -0.8660254037844409281 ) ) ;
#18530 = APPLICATION_CONTEXT ( 'automotive_design' ) ;
#18531 = EDGE_CURVE ( 'NONE', #10265, #6948, #30091, .T. ) ;
#18533 = CARTESIAN_POINT ( 'NONE',  ( 0.000000000000000000, 55.00000000000000000, -5.000000000000000000 ) ) ;
#18532 = AXIS2_PLACEMENT_3D ( 'NONE', #29567, #15534, #29213 ) ;
#18534 = ORIENTED_EDGE ( 'NONE', *, *, #1848, .F. ) ;
#18535 = VERTEX_POINT ( 'NONE', #36173 ) ;
#18536 = CYLINDRICAL_SURFACE ( 'NONE', #21299, 1.999999999999998224 ) ;
#18537 = AXIS2_PLACEMENT_3D ( 'NONE', #2206, #19452, #7458 ) ;
#18538 = ADVANCED_FACE ( 'NONE', ( #15737 ), #15561, .T. ) ;
#18539 = DIRECTION ( 'NONE',  ( 0.000000000000000000, 0.000000000000000000, 1.000000000000000000 ) ) ;
#18540 = ORIENTED_EDGE ( 'NONE', *, *, #20513, .F. ) ;
#18541 = VECTOR ( 'NONE', #11021, 1000.000000000000000 ) ;
#18542 = DIRECTION ( 'NONE',  ( 1.000000000000000000, 0.000000000000000000, 0.000000000000000000 ) ) ;
#18543 = EDGE_LOOP ( 'NONE', ( #3404, #8595, #31456, #16186, #21857 ) ) ;
#18544 = DIRECTION ( 'NONE',  ( 0.000000000000000000, 0.000000000000000000, 1.000000000000000000 ) ) ;
#18545 = CIRCLE ( 'NONE', #29907, 2.000000000000001776 ) ;
#18546 = FACE_BOUND ( 'NONE', #32480, .T. ) ;
#18547 = CIRCLE ( 'NONE', #32279, 30.00000000000000000 ) ;
#18548 = ORIENTED_EDGE ( 'NONE', *, *, #18683, .F. ) ;
#18549 = VERTEX_POINT ( 'NONE', #15922 ) ;
#18550 = AXIS2_PLACEMENT_3D ( 'NONE', #25659, #11008, #22652 ) ;
#18551 = DIRECTION ( 'NONE',  ( 1.000000000000000000, 0.000000000000000000, 0.000000000000000000 ) ) ;
#18552 = VERTEX_POINT ( 'NONE', #7124 ) ;
#18553 = SHAPE_REPRESENTATION_RELATIONSHIP ( 'NONE' , 'NONE' ,  #34443, #23302 ) ;
#18554 = DIRECTION ( 'NONE',  ( 0.000000000000000000, 0.8660254037844379305, -0.5000000000000014433 ) ) ;
#18555 = EDGE_CURVE ( 'NONE', #23730, #816, #17268, .T. ) ;
#18556 = CARTESIAN_POINT ( 'NONE',  ( -101.7384897088158766, -110.2237710830526112, 32.50000000000000000 ) ) ;
#18557 = CARTESIAN_POINT ( 'NONE',  ( -75.00000337463097821, 25.98076211353318854, 17.49999999999999645 ) ) ;
#18558 = ORIENTED_EDGE ( 'NONE', *, *, #21476, .F. ) ;
#18559 = CARTESIAN_POINT ( 'NONE',  ( -18.00000337463123756, -86.60254037844400443, -9.999999999999998224 ) ) ;
#18560 = ORIENTED_EDGE ( 'NONE', *, *, #29374, .T. ) ;
#18561 = EDGE_CURVE ( 'NONE', #15127, #24605, #153, .T. ) ;
#18562 = ORIENTED_EDGE ( 'NONE', *, *, #28888, .F. ) ;
#18563 = CIRCLE ( 'NONE', #2398, 1.750000000000015765 ) ;
#18564 = ORIENTED_EDGE ( 'NONE', *, *, #10268, .F. ) ;
#18565 = DIRECTION ( 'NONE',  ( 0.000000000000000000, 0.000000000000000000, 1.000000000000000000 ) ) ;
#18566 = EDGE_CURVE ( 'NONE', #16909, #36669, #15751, .T. ) ;
#18567 = PRESENTATION_LAYER_ASSIGNMENT (  '', '', ( #33559 ) ) ;
#18568 = DIRECTION ( 'NONE',  ( 1.000000000000000000, 0.000000000000000000, 0.000000000000000000 ) ) ;
#18569 = ORIENTED_EDGE ( 'NONE', *, *, #3957, .T. ) ;
#18570 = CARTESIAN_POINT ( 'NONE',  ( -5.000000000000000000, -0.1416384297035285789, -0.5080592402122394713 ) ) ;
#18571 = VECTOR ( 'NONE', #24777, 1000.000000000000000 ) ;
#18572 = CARTESIAN_POINT ( 'NONE',  ( 74.99999662536836809, 25.98076211353319565, -9.999999999999998224 ) ) ;
#18573 = EDGE_LOOP ( 'NONE', ( #30671, #11726, #30684, #35161 ) ) ;
#18574 = CARTESIAN_POINT ( 'NONE',  ( 86.99999662536832545, 8.660254037844394404, -9.999999999999998224 ) ) ;
#18575 = DIRECTION ( 'NONE',  ( -1.000000000000000000, 0.000000000000000000, 0.000000000000000000 ) ) ;
#18576 = AXIS2_PLACEMENT_3D ( 'NONE', #5925, #17701, #17356 ) ;
#18577 = DIRECTION ( 'NONE',  ( 1.000000000000000000, 0.000000000000000000, 0.000000000000000000 ) ) ;
#18578 = CARTESIAN_POINT ( 'NONE',  ( 73.90204319670436917, -6.988578749851891203, -5.000000000000000000 ) ) ;
#18579 = AXIS2_PLACEMENT_3D ( 'NONE', #20738, #17948, #29375 ) ;
#18580 = CARTESIAN_POINT ( 'NONE',  ( 57.99999662536842493, -51.96152422706639840, -9.999999999999998224 ) ) ;
#18581 = CARTESIAN_POINT ( 'NONE',  ( -2.500000000000003997, -4.330127018922192761, -6.000000000000000000 ) ) ;
#18582 = VERTEX_POINT ( 'NONE', #32990 ) ;
#18583 = ORIENTED_EDGE ( 'NONE', *, *, #3572, .T. ) ;
#18584 = DIRECTION ( 'NONE',  ( 0.000000000000000000, 0.000000000000000000, 1.000000000000000000 ) ) ;
#18585 = EDGE_CURVE ( 'NONE', #20117, #32307, #29988, .T. ) ;
#18586 = DIRECTION ( 'NONE',  ( 0.000000000000000000, 0.000000000000000000, 1.000000000000000000 ) ) ;
#18587 = CARTESIAN_POINT ( 'NONE',  ( 32.50000000000065370, 56.29165124598813463, 12.49999999999999822 ) ) ;
#18588 = CARTESIAN_POINT ( 'NONE',  ( -63.00000337463102085, 60.62177826491077326, -9.999999999999998224 ) ) ;
#18589 = EDGE_LOOP ( 'NONE', ( #8919, #5974, #12957, #7362, #26811, #22632 ) ) ;
#18590 = UNCERTAINTY_MEASURE_WITH_UNIT (LENGTH_MEASURE( 1.000000000000000082E-05 ), #18939, 'distance_accuracy_value', 'NONE');
#18591 = DIRECTION ( 'NONE',  ( 0.000000000000000000, 0.000000000000000000, 1.000000000000000000 ) ) ;
#18592 = FACE_OUTER_BOUND ( 'NONE', #21580, .T. ) ;
#18593 = ORIENTED_EDGE ( 'NONE', *, *, #37103, .T. ) ;
#18594 = DIRECTION ( 'NONE',  ( 0.000000000000000000, 0.000000000000000000, 1.000000000000000000 ) ) ;
#18595 = ORIENTED_EDGE ( 'NONE', *, *, #34645, .T. ) ;
#18596 = LINE ( 'NONE', #24599, #4166 ) ;
#18597 = DIRECTION ( 'NONE',  ( 0.000000000000000000, 0.000000000000000000, 1.000000000000000000 ) ) ;
#18598 = EDGE_CURVE ( 'NONE', #8789, #29589, #17538, .T. ) ;
#18599 = CARTESIAN_POINT ( 'NONE',  ( 4.279208249584789847, 3.302900657080011459, -1.325189086772932123 ) ) ;
#18600 = EDGE_LOOP ( 'NONE', ( #9688, #31285 ) ) ;
#18601 = EDGE_CURVE ( 'NONE', #14753, #9603, #10296, .T. ) ;
#18602 = ORIENTED_EDGE ( 'NONE', *, *, #26497, .F. ) ;
#18603 = EDGE_CURVE ( 'NONE', #24524, #31695, #20523, .T. ) ;
#18604 = ORIENTED_EDGE ( 'NONE', *, *, #19176, .F. ) ;
#18605 = CYLINDRICAL_SURFACE ( 'NONE', #27370, 5.999999999999999112 ) ;
#18606 = DIRECTION ( 'NONE',  ( 1.000000000000000000, 0.000000000000000000, 0.000000000000000000 ) ) ;
#18607 = ADVANCED_FACE ( 'NONE', ( #11903 ), #8031, .T. ) ;
#18608 = CARTESIAN_POINT ( 'NONE',  ( 72.99999662536835388, -25.98076211353319565, -9.999999999999998224 ) ) ;
#18609 = CARTESIAN_POINT ( 'NONE',  ( 42.99999662536848888, 60.62177826491077326, -9.999999999999998224 ) ) ;
#18610 = LINE ( 'NONE', #13160, #9945 ) ;
#18611 = EDGE_CURVE ( 'NONE', #36868, #148, #660, .T. ) ;
#18612 = ORIENTED_EDGE ( 'NONE', *, *, #35205, .T. ) ;
#18613 = CARTESIAN_POINT ( 'NONE',  ( 76.71706219562632612, -9.685771384082254798, 12.50000000000000000 ) ) ;
#18614 = LINE ( 'NONE', #32649, #7185 ) ;
#18615 = CIRCLE ( 'NONE', #32978, 2.000000000000001776 ) ;
#18616 = CARTESIAN_POINT ( 'NONE',  ( 0.000000000000000000, 89.94802294027088863, 27.49999999999999645 ) ) ;
#18617 = ORIENTED_EDGE ( 'NONE', *, *, #2085, .T. ) ;
#18618 = DIRECTION ( 'NONE',  ( 1.000000000000000000, 0.000000000000000000, 0.000000000000000000 ) ) ;
#18619 = DIRECTION ( 'NONE',  ( 1.000000000000000000, 0.000000000000000000, 0.000000000000000000 ) ) ;
#18620 = EDGE_CURVE ( 'NONE', #4001, #29187, #18149, .T. ) ;
#18621 = EDGE_LOOP ( 'NONE', ( #27379, #36542 ) ) ;
#18622 = EDGE_CURVE ( 'NONE', #550, #35128, #28101, .T. ) ;
#18623 = ORIENTED_EDGE ( 'NONE', *, *, #16133, .F. ) ;
#18624 = EDGE_CURVE ( 'NONE', #7482, #32676, #17715, .T. ) ;
#18625 = ADVANCED_FACE ( 'NONE', ( #5586 ), #25124, .F. ) ;
#18626 = CARTESIAN_POINT ( 'NONE',  ( -35.00000337463116296, 77.94228634059957983, -9.999999999999998224 ) ) ;
#18627 = DIRECTION ( 'NONE',  ( 1.000000000000000000, 0.000000000000000000, 0.000000000000000000 ) ) ;
#18628 = FACE_OUTER_BOUND ( 'NONE', #2141, .T. ) ;
#18629 = ORIENTED_EDGE ( 'NONE', *, *, #1561, .F. ) ;
#18630 = ORIENTED_EDGE ( 'NONE', *, *, #18505, .T. ) ;
#18631 = EDGE_LOOP ( 'NONE', ( #14213, #5742 ) ) ;
#18632 = DIRECTION ( 'NONE',  ( 0.000000000000000000, 0.000000000000000000, 1.000000000000000000 ) ) ;
#18633 = EDGE_LOOP ( 'NONE', ( #16926, #31071, #12234 ) ) ;
#18634 = ORIENTED_EDGE ( 'NONE', *, *, #28682, .F. ) ;
#18635 = FACE_BOUND ( 'NONE', #27531, .T. ) ;
#18636 = ORIENTED_EDGE ( 'NONE', *, *, #36830, .F. ) ;
#18637 = VERTEX_POINT ( 'NONE', #11214 ) ;
#18638 = FACE_OUTER_BOUND ( 'NONE', #24090, .T. ) ;
#18640 = AXIS2_PLACEMENT_3D ( 'NONE', #26951, #12865, #12298 ) ;
#18639 = FACE_OUTER_BOUND ( 'NONE', #1925, .T. ) ;
#18641 = ORIENTED_EDGE ( 'NONE', *, *, #578, .F. ) ;
#18642 = ORIENTED_EDGE ( 'NONE', *, *, #21702, .T. ) ;
#18643 = DIRECTION ( 'NONE',  ( 0.000000000000000000, 0.000000000000000000, 1.000000000000000000 ) ) ;
#18644 = DIRECTION ( 'NONE',  ( 1.000000000000000000, 0.000000000000000000, 0.000000000000000000 ) ) ;
#18645 = DIRECTION ( 'NONE',  ( 0.000000000000000000, 0.000000000000000000, 1.000000000000000000 ) ) ;
#18646 = CARTESIAN_POINT ( 'NONE',  ( -67.00000337463102085, 60.62177826491077326, -9.999999999999998224 ) ) ;
#18647 = ORIENTED_EDGE ( 'NONE', *, *, #26331, .F. ) ;
#18648 = DIRECTION ( 'NONE',  ( -1.000000000000000000, 0.000000000000000000, 0.000000000000000000 ) ) ;
#18649 = ORIENTED_EDGE ( 'NONE', *, *, #16804, .F. ) ;
#18650 = CARTESIAN_POINT ( 'NONE',  ( -50.00000337463112032, -51.96152422706641971, -9.999999999999998224 ) ) ;
#18651 = CARTESIAN_POINT ( 'NONE',  ( -107.2724133595211526, 47.50000000000096634, 32.50002500000000083 ) ) ;
#18652 = DIRECTION ( 'NONE',  ( -0.000000000000000000, -0.000000000000000000, 1.000000000000000000 ) ) ;
#18653 = DIRECTION ( 'NONE',  ( 0.000000000000000000, 0.000000000000000000, 1.000000000000000000 ) ) ;
#18654 = CYLINDRICAL_SURFACE ( 'NONE', #18895, 1.999999999999998224 ) ;
#18655 = CARTESIAN_POINT ( 'NONE',  ( 27.78182860042856461, 56.67878100130339902, 12.49999999999999822 ) ) ;
#18656 = DIRECTION ( 'NONE',  ( 0.000000000000000000, 0.000000000000000000, 1.000000000000000000 ) ) ;
#18657 = ORIENTED_EDGE ( 'NONE', *, *, #14885, .T. ) ;
#18658 = CARTESIAN_POINT ( 'NONE',  ( 26.99999662536859546, -77.94228634059960825, -9.999999999999998224 ) ) ;
#18659 = AXIS2_PLACEMENT_3D ( 'NONE', #14418, #8599, #5440 ) ;
#18660 = CARTESIAN_POINT ( 'NONE',  ( -82.00000337463094979, 17.32050807568878525, -5.000000000000000000 ) ) ;
#18661 = CARTESIAN_POINT ( 'NONE',  ( 69.99999662536838230, -51.96152422706639840, -9.999999999999998224 ) ) ;
#18662 = ORIENTED_EDGE ( 'NONE', *, *, #34858, .F. ) ;
#18663 = EDGE_LOOP ( 'NONE', ( #19428, #11917, #13076, #19248 ) ) ;
#18664 = ORIENTED_EDGE ( 'NONE', *, *, #18820, .F. ) ;
#18665 = EDGE_CURVE ( 'NONE', #21723, #29824, #7962, .T. ) ;
#18666 = LINE ( 'NONE', #16398, #6452 ) ;
#18667 = CARTESIAN_POINT ( 'NONE',  ( 54.99999662536844625, 43.30127018922198801, -5.000000000000000000 ) ) ;
#18668 = DIRECTION ( 'NONE',  ( 1.000000000000000000, 0.000000000000000000, 0.000000000000000000 ) ) ;
#18669 = ORIENTED_EDGE ( 'NONE', *, *, #20113, .F. ) ;
#18670 = DIRECTION ( 'NONE',  ( 0.000000000000000000, 0.000000000000000000, 1.000000000000000000 ) ) ;
#18671 = CARTESIAN_POINT ( 'NONE',  ( 0.000000000000000000, 0.000000000000000000, 12.49999999999999822 ) ) ;
#18672 = ORIENTED_EDGE ( 'NONE', *, *, #30354, .T. ) ;
#18673 = DIRECTION ( 'NONE',  ( 0.000000000000000000, 0.000000000000000000, 1.000000000000000000 ) ) ;
#18674 = EDGE_LOOP ( 'NONE', ( #23993, #15514, #26394, #9833 ) ) ;
#18675 = FACE_BOUND ( 'NONE', #26541, .T. ) ;
#18676 = CARTESIAN_POINT ( 'NONE',  ( -3.000000000000000000, 3.673940397442059868E-16, 0.000000000000000000 ) ) ;
#18677 = CARTESIAN_POINT ( 'NONE',  ( 2.179555516819077443, -4.788648424347467625, -4.057628883416056098 ) ) ;
#18678 = VECTOR ( 'NONE', #3817, 1000.000000000000000 ) ;
#18679 = CARTESIAN_POINT ( 'NONE',  ( 71.20511420343271425, 36.23716514913449060, -5.000000000000000000 ) ) ;
#18680 = VERTEX_POINT ( 'NONE', #34973 ) ;
#18681 = CARTESIAN_POINT ( 'NONE',  ( -15.97563234535668109, 90.60231327712331506, -49.86561046011506448 ) ) ;
#18682 = AXIS2_PLACEMENT_3D ( 'NONE', #3198, #11454, #36780 ) ;
#18683 = EDGE_CURVE ( 'NONE', #13179, #8353, #28898, .T. ) ;
#18684 = CONTEXT_DEPENDENT_SHAPE_REPRESENTATION ( #22628, #7725 ) ;
#18685 = EDGE_CURVE ( 'NONE', #13703, #16037, #10855, .T. ) ;
#18686 = FACE_BOUND ( 'NONE', #31863, .T. ) ;
#18687 = CARTESIAN_POINT ( 'NONE',  ( -46.00000000000000000, 103.4105893997321886, -19.99999999999999645 ) ) ;
#18688 = DIRECTION ( 'NONE',  ( 1.000000000000000000, 0.000000000000000000, 0.000000000000000000 ) ) ;
#18689 = DIRECTION ( 'NONE',  ( 0.000000000000000000, -0.000000000000000000, -1.000000000000000000 ) ) ;
#18690 = ORIENTED_EDGE ( 'NONE', *, *, #17216, .T. ) ;
#18691 = FACE_OUTER_BOUND ( 'NONE', #32580, .T. ) ;
#18692 = DIRECTION ( 'NONE',  ( 1.000000000000000000, 0.000000000000000000, 0.000000000000000000 ) ) ;
#18693 = CARTESIAN_POINT ( 'NONE',  ( -35.00000337463116296, 77.94228634059957983, -9.999999999999998224 ) ) ;
#18694 = ADVANCED_FACE ( 'NONE', ( #36903 ), #31098, .F. ) ;
#18695 = VERTEX_POINT ( 'NONE', #25670 ) ;
#18696 = ORIENTED_EDGE ( 'NONE', *, *, #23416, .F. ) ;
#18697 = DIRECTION ( 'NONE',  ( 0.000000000000000000, 0.000000000000000000, 1.000000000000000000 ) ) ;
#18698 = DIRECTION ( 'NONE',  ( 1.000000000000000000, 0.000000000000000000, 0.000000000000000000 ) ) ;
#18699 = DIRECTION ( 'NONE',  ( 3.469446951953612611E-15, 1.000000000000000000, 0.000000000000000000 ) ) ;
#18700 = ORIENTED_EDGE ( 'NONE', *, *, #20381, .F. ) ;
#18701 = AXIS2_PLACEMENT_3D ( 'NONE', #32460, #15414, #20848 ) ;
#18702 = EDGE_CURVE ( 'NONE', #27052, #27413, #3163, .T. ) ;
#18703 = CARTESIAN_POINT ( 'NONE',  ( -3.499999999999987566, 55.00000000000000000, -10.00000000000000178 ) ) ;
#18704 = CYLINDRICAL_SURFACE ( 'NONE', #19643, 2.500000000000000444 ) ;
#18705 = DIRECTION ( 'NONE',  ( 0.000000000000000000, 0.000000000000000000, 1.000000000000000000 ) ) ;
#18706 = DIRECTION ( 'NONE',  ( -1.000000000000000000, 0.000000000000000000, 0.000000000000000000 ) ) ;
#18707 = ORIENTED_EDGE ( 'NONE', *, *, #25672, .T. ) ;
#18708 = ORIENTED_EDGE ( 'NONE', *, *, #13415, .T. ) ;
#18709 = CARTESIAN_POINT ( 'NONE',  ( 4.999999999999999112, 1.231908430319627934, -0.1119772403577117409 ) ) ;
#18710 = CARTESIAN_POINT ( 'NONE',  ( 4.467624384280048488, 0.000000000000000000, 0.000000000000000000 ) ) ;
#18711 = EDGE_LOOP ( 'NONE', ( #30616, #3898 ) ) ;
#18712 = CARTESIAN_POINT ( 'NONE',  ( -1.598077599632966805, -4.850852159561880761, -3.971474537231491908 ) ) ;
#18713 = EDGE_LOOP ( 'NONE', ( #36920, #33623, #17992, #26360, #6400 ) ) ;
#18714 = CARTESIAN_POINT ( 'NONE',  ( -50.00000337463110611, -69.28203230275519786, 17.49999999999999645 ) ) ;
#18715 = AXIS2_PLACEMENT_3D ( 'NONE', #17636, #6594, #12175 ) ;
#18716 = AXIS2_PLACEMENT_3D ( 'NONE', #17673, #28922, #21047 ) ;
#18717 = FACE_BOUND ( 'NONE', #34869, .T. ) ;
#18718 = ORIENTED_EDGE ( 'NONE', *, *, #33713, .F. ) ;
#18719 = ORIENTED_EDGE ( 'NONE', *, *, #35780, .F. ) ;
#18720 = ADVANCED_FACE ( 'NONE', ( #28449 ), #2425, .F. ) ;
#18721 = CARTESIAN_POINT ( 'NONE',  ( -38.00000337463113453, -69.28203230275519786, -5.000000000000000000 ) ) ;
#18722 = ORIENTED_EDGE ( 'NONE', *, *, #11430, .F. ) ;
#18723 = EDGE_CURVE ( 'NONE', #725, #21874, #27701, .T. ) ;
#18724 =( NAMED_UNIT ( * ) SI_UNIT ( $, .STERADIAN. ) SOLID_ANGLE_UNIT ( ) );
#18725 = DIRECTION ( 'NONE',  ( 1.000000000000000000, 0.000000000000000000, 0.000000000000000000 ) ) ;
#18726 = CIRCLE ( 'NONE', #6722, 2.000000000000001776 ) ;
#18727 = DIRECTION ( 'NONE',  ( 0.000000000000000000, 0.000000000000000000, 1.000000000000000000 ) ) ;
#18728 = CARTESIAN_POINT ( 'NONE',  ( 89.99999662536828282, 0.000000000000000000, -9.999999999999998224 ) ) ;
#18729 = VERTEX_POINT ( 'NONE', #14214 ) ;
#18730 = CYLINDRICAL_SURFACE ( 'NONE', #25082, 2.000000000000001776 ) ;
#18731 = EDGE_CURVE ( 'NONE', #26888, #14326, #4376, .T. ) ;
#18732 = DIRECTION ( 'NONE',  ( -0.000000000000000000, -0.000000000000000000, 1.000000000000000000 ) ) ;
#18733 = ORIENTED_EDGE ( 'NONE', *, *, #7822, .F. ) ;
#18734 = ORIENTED_EDGE ( 'NONE', *, *, #29385, .T. ) ;
#18735 = EDGE_CURVE ( 'NONE', #5564, #25160, #12127, .T. ) ;
#18736 = VERTEX_POINT ( 'NONE', #472 ) ;
#18737 = CARTESIAN_POINT ( 'NONE',  ( 81.99999662536833966, 34.64101615137759183, -9.999999999999998224 ) ) ;
#18738 = FACE_OUTER_BOUND ( 'NONE', #27902, .T. ) ;
#18739 = ORIENTED_EDGE ( 'NONE', *, *, #30271, .F. ) ;
#18740 = CARTESIAN_POINT ( 'NONE',  ( 0.000000000000000000, 0.000000000000000000, -5.000000000000000000 ) ) ;
#18741 = DIRECTION ( 'NONE',  ( 1.000000000000000000, 0.000000000000000000, 0.000000000000000000 ) ) ;
#18742 = VERTEX_POINT ( 'NONE', #8232 ) ;
#18743 = DIRECTION ( 'NONE',  ( -0.000000000000000000, -0.000000000000000000, 1.000000000000000000 ) ) ;
#18744 = CYLINDRICAL_SURFACE ( 'NONE', #9040, 30.00000000000000000 ) ;
#18745 = DIRECTION ( 'NONE',  ( 1.000000000000000000, 0.000000000000000000, 0.000000000000000000 ) ) ;
#18746 = CARTESIAN_POINT ( 'NONE',  ( 102.2321609167755980, -32.43314223652354400, 32.50000000000000000 ) ) ;
#18747 = LINE ( 'NONE', #30168, #5228 ) ;
#18748 = CARTESIAN_POINT ( 'NONE',  ( -43.00000337463112743, -60.62177826491080168, 17.49999999999999645 ) ) ;
#18749 = VERTEX_POINT ( 'NONE', #29698 ) ;
#18750 = ORIENTED_EDGE ( 'NONE', *, *, #3690, .T. ) ;
#18751 = EDGE_CURVE ( 'NONE', #4621, #8789, #772, .T. ) ;
#18752 = DIRECTION ( 'NONE',  ( 0.000000000000000000, 0.000000000000000000, 1.000000000000000000 ) ) ;
#18753 = AXIS2_PLACEMENT_3D ( 'NONE', #18740, #32804, #24368 ) ;
#18754 = CARTESIAN_POINT ( 'NONE',  ( -53.00000337463110611, -43.30127018922202353, -9.999999999999998224 ) ) ;
#18755 = PLANE ( 'NONE',  #11464 ) ;
#18756 = LINE ( 'NONE', #10143, #19132 ) ;
#18757 = ORIENTED_EDGE ( 'NONE', *, *, #17585, .T. ) ;
#18758 = EDGE_CURVE ( 'NONE', #30786, #17343, #9749, .T. ) ;
#18759 = DIRECTION ( 'NONE',  ( 0.000000000000000000, 0.000000000000000000, 1.000000000000000000 ) ) ;
#18760 = CARTESIAN_POINT ( 'NONE',  ( -2.500000000000003997, -4.330127018922192761, -6.000000000000000000 ) ) ;
#18761 = PLANE ( 'NONE',  #32952 ) ;
#18762 = ORIENTED_EDGE ( 'NONE', *, *, #25860, .F. ) ;
#18763 = ADVANCED_FACE ( 'NONE', ( #21466 ), #32903, .F. ) ;
#18764 = CYLINDRICAL_SURFACE ( 'NONE', #427, 2.000000000000000000 ) ;
#18765 = VECTOR ( 'NONE', #4194, 1000.000000000000000 ) ;
#18766 = ORIENTED_EDGE ( 'NONE', *, *, #8439, .T. ) ;
#18767 =( NAMED_UNIT ( * ) PLANE_ANGLE_UNIT ( ) SI_UNIT ( $, .RADIAN. ) );
#18768 = DIRECTION ( 'NONE',  ( 1.000000000000000000, 0.000000000000000000, 0.000000000000000000 ) ) ;
#18769 = AXIS2_PLACEMENT_3D ( 'NONE', #28116, #13480, #2438 ) ;
#18770 = CARTESIAN_POINT ( 'NONE',  ( -68.00000337463099243, 17.32050807568877460, -9.999999999999998224 ) ) ;
#18771 = CARTESIAN_POINT ( 'NONE',  ( -8.000003374631287301, 69.28203230275516944, -5.000000000000000000 ) ) ;
#18772 = EDGE_LOOP ( 'NONE', ( #7211, #443, #24150, #21548 ) ) ;
#18773 = ORIENTED_EDGE ( 'NONE', *, *, #27711, .F. ) ;
#18774 = EDGE_CURVE ( 'NONE', #29875, #23027, #21741, .T. ) ;
#18775 = VERTEX_POINT ( 'NONE', #30076 ) ;
#18776 = DIRECTION ( 'NONE',  ( -1.000000000000000000, 0.000000000000000000, 0.000000000000000000 ) ) ;
#18777 = AXIS2_PLACEMENT_3D ( 'NONE', #19221, #36642, #36271 ) ;
#18778 = DIRECTION ( 'NONE',  ( 1.000000000000000000, 0.000000000000000000, 0.000000000000000000 ) ) ;
#18779 = DIRECTION ( 'NONE',  ( 0.000000000000000000, 0.000000000000000000, 1.000000000000000000 ) ) ;
#18780 = CARTESIAN_POINT ( 'NONE',  ( -5.000000000000000888, 2.886751345948107783, -3.984345921091764886 ) ) ;
#18781 = DIRECTION ( 'NONE',  ( 1.000000000000000000, 0.000000000000000000, 0.000000000000000000 ) ) ;
#18782 = VERTEX_POINT ( 'NONE', #13016 ) ;
#18783 = CIRCLE ( 'NONE', #2016, 1.999999999999998224 ) ;
#18784 = CARTESIAN_POINT ( 'NONE',  ( 31.46585318596250502, 86.45172111230321832, -4.999999999999997335 ) ) ;
#18785 = PRODUCT_DEFINITION_SHAPE ( 'NONE', 'NONE',  #37117 ) ;
#18786 = DIRECTION ( 'NONE',  ( 0.000000000000000000, 0.000000000000000000, 1.000000000000000000 ) ) ;
#18787 = CARTESIAN_POINT ( 'NONE',  ( 2.999996625368645198, 77.94228634059957983, -9.999999999999998224 ) ) ;
#18788 = EDGE_LOOP ( 'NONE', ( #8823, #14096, #33224, #20827 ) ) ;
#18789 =( REPRESENTATION_RELATIONSHIP ('NONE','NONE', #15268, #34443 ) REPRESENTATION_RELATIONSHIP_WITH_TRANSFORMATION ( #8532 )SHAPE_REPRESENTATION_RELATIONSHIP( ) );
#18790 = CARTESIAN_POINT ( 'NONE',  ( -80.00000337463094979, -17.32050807568882078, -5.000000000000000000 ) ) ;
#18791 = CYLINDRICAL_SURFACE ( 'NONE', #25539, 2.000000000000001776 ) ;
#18792 = AXIS2_PLACEMENT_3D ( 'NONE', #33786, #10354, #27775 ) ;
#18793 = VERTEX_POINT ( 'NONE', #4399 ) ;
#18794 = CIRCLE ( 'NONE', #36168, 2.000000000000001776 ) ;
#18795 = VERTEX_POINT ( 'NONE', #24474 ) ;
#18796 = EDGE_CURVE ( 'NONE', #9227, #7555, #14542, .T. ) ;
#18797 = DIRECTION ( 'NONE',  ( 1.000000000000000000, 0.000000000000000000, 0.000000000000000000 ) ) ;
#18798 = DIRECTION ( 'NONE',  ( 0.000000000000000000, 0.000000000000000000, 1.000000000000000000 ) ) ;
#18799 = ADVANCED_FACE ( 'NONE', ( #32141 ), #18264, .T. ) ;
#18800 = CARTESIAN_POINT ( 'NONE',  ( -3.447886558751868336, -3.782864459065579776, -0.7348938709837913308 ) ) ;
#18801 = ORIENTED_EDGE ( 'NONE', *, *, #12613, .F. ) ;
#18802 = ORIENTED_EDGE ( 'NONE', *, *, #32137, .T. ) ;
#18803 = VERTEX_POINT ( 'NONE', #29342 ) ;
#18804 = AXIS2_PLACEMENT_3D ( 'NONE', #31336, #11469, #19743 ) ;
#18805 = EDGE_CURVE ( 'NONE', #24065, #2400, #35513, .T. ) ;
#18806 = DIRECTION ( 'NONE',  ( 0.000000000000000000, 0.000000000000000000, 1.000000000000000000 ) ) ;
#18807 = ORIENTED_EDGE ( 'NONE', *, *, #16239, .F. ) ;
#18809 = EDGE_CURVE ( 'NONE', #29585, #16050, #3773, .T. ) ;
#18808 = VERTEX_POINT ( 'NONE', #12813 ) ;
#18810 = CARTESIAN_POINT ( 'NONE',  ( 0.000000000000000000, -55.00000000000000000, -5.000000000000000000 ) ) ;
#18811 = ORIENTED_EDGE ( 'NONE', *, *, #14570, .F. ) ;
#18812 = EDGE_CURVE ( 'NONE', #8370, #21726, #5576, .T. ) ;
#18813 = ORIENTED_EDGE ( 'NONE', *, *, #679, .F. ) ;
#18814 = CARTESIAN_POINT ( 'NONE',  ( -63.00000337463102085, 60.62177826491077326, -9.999999999999998224 ) ) ;
#18815 = CARTESIAN_POINT ( 'NONE',  ( 57.99999662536842493, -51.96152422706639840, -9.999999999999998224 ) ) ;
#18816 = ORIENTED_EDGE ( 'NONE', *, *, #21897, .F. ) ;
#18817 = EDGE_LOOP ( 'NONE', ( #11824, #27660 ) ) ;
#18818 = LINE ( 'NONE', #6810, #26273 ) ;
#18819 = DIRECTION ( 'NONE',  ( -1.000000000000000000, 0.000000000000000000, 0.000000000000000000 ) ) ;
#18820 = EDGE_CURVE ( 'NONE', #24840, #24399, #834, .T. ) ;
#18821 = CARTESIAN_POINT ( 'NONE',  ( 71.99999662536839651, -3.469446951953614189E-15, -5.000000000000000000 ) ) ;
#18822 = EDGE_CURVE ( 'NONE', #36472, #12700, #9148, .T. ) ;
#18823 = CARTESIAN_POINT ( 'NONE',  ( 5.999999999999998224, 6.123233995736766282E-16, -5.000000000000000000 ) ) ;
#18824 = CIRCLE ( 'NONE', #2644, 3.000000000000006217 ) ;
#18825 = ADVANCED_FACE ( 'NONE', ( #20914 ), #7028, .F. ) ;
#18826 = ORIENTED_EDGE ( 'NONE', *, *, #26122, .F. ) ;
#18827 = DIRECTION ( 'NONE',  ( 1.000000000000000000, 0.000000000000000000, 0.000000000000000000 ) ) ;
#18828 = VERTEX_POINT ( 'NONE', #6658 ) ;
#18829 = CYLINDRICAL_SURFACE ( 'NONE', #4680, 2.000000000000001776 ) ;
#18830 = EDGE_CURVE ( 'NONE', #13152, #12255, #16335, .T. ) ;
#18831 = CARTESIAN_POINT ( 'NONE',  ( 96.53048327204888324, -102.5304832720499633, 32.50000000000000000 ) ) ;
#18832 = DIRECTION ( 'NONE',  ( 0.000000000000000000, 0.000000000000000000, 1.000000000000000000 ) ) ;
#18833 = CARTESIAN_POINT ( 'NONE',  ( 69.99999662536839651, -3.469446951953614189E-15, 17.49999999999999645 ) ) ;
#18834 = CARTESIAN_POINT ( 'NONE',  ( 0.000000000000000000, -2.935248768560059229, 3.469446951953614189E-15 ) ) ;
#18835 = AXIS2_PLACEMENT_3D ( 'NONE', #28298, #30930, #10707 ) ;
#18836 = DIRECTION ( 'NONE',  ( 0.000000000000000000, 0.000000000000000000, 1.000000000000000000 ) ) ;
#18837 = AXIS2_PLACEMENT_3D ( 'NONE', #26436, #6372, #24008 ) ;
#18838 = DIRECTION ( 'NONE',  ( 0.000000000000000000, 0.000000000000000000, 1.000000000000000000 ) ) ;
#18839 = ORIENTED_EDGE ( 'NONE', *, *, #9501, .T. ) ;
#18840 = CARTESIAN_POINT ( 'NONE',  ( -5.000000000000000000, 30.00000000000000355, -15.00000000000000000 ) ) ;
#18841 = DIRECTION ( 'NONE',  ( 0.000000000000000000, 0.000000000000000000, 1.000000000000000000 ) ) ;
#18842 = DIRECTION ( 'NONE',  ( 1.000000000000000000, 0.000000000000000000, 0.000000000000000000 ) ) ;
#18843 = ORIENTED_EDGE ( 'NONE', *, *, #19294, .T. ) ;
#18844 = ORIENTED_EDGE ( 'NONE', *, *, #26397, .T. ) ;
#18845 = ORIENTED_EDGE ( 'NONE', *, *, #34655, .T. ) ;
#18846 = DIRECTION ( 'NONE',  ( 1.000000000000000000, 0.000000000000000000, 0.000000000000000000 ) ) ;
#18847 = DIRECTION ( 'NONE',  ( 0.000000000000000000, 0.000000000000000000, 1.000000000000000000 ) ) ;
#18848 = AXIS2_PLACEMENT_3D ( 'NONE', #35264, #9914, #9558 ) ;
#18849 = EDGE_LOOP ( 'NONE', ( #13917, #11700, #20238, #20891 ) ) ;
#18850 = VECTOR ( 'NONE', #15381, 1000.000000000000000 ) ;
#18851 = CARTESIAN_POINT ( 'NONE',  ( -68.00000337463100664, -17.32050807568882078, -9.999999999999998224 ) ) ;
#18852 = FACE_OUTER_BOUND ( 'NONE', #34886, .T. ) ;
#18853 = ORIENTED_EDGE ( 'NONE', *, *, #30286, .F. ) ;
#18854 = DIRECTION ( 'NONE',  ( 1.000000000000000000, 0.000000000000000000, -0.000000000000000000 ) ) ;
#18855 = ORIENTED_EDGE ( 'NONE', *, *, #4326, .F. ) ;
#18856 = FACE_BOUND ( 'NONE', #20227, .T. ) ;
#18857 = AXIS2_PLACEMENT_3D ( 'NONE', #21902, #27339, #35433 ) ;
#18858 = AXIS2_PLACEMENT_3D ( 'NONE', #718, #20413, #6160 ) ;
#18859 = CARTESIAN_POINT ( 'NONE',  ( -87.00000337463093558, 8.660254037844389075, -9.999999999999998224 ) ) ;
#18860 = DIRECTION ( 'NONE',  ( 0.000000000000000000, 0.000000000000000000, 1.000000000000000000 ) ) ;
#18861 = VECTOR ( 'NONE', #13850, 1000.000000000000000 ) ;
#18862 = VERTEX_POINT ( 'NONE', #15472 ) ;
#18863 = CARTESIAN_POINT ( 'NONE',  ( 4.999999999999999112, 0.4881033300985041512, -6.000000000000000000 ) ) ;
#18864 = DIRECTION ( 'NONE',  ( -0.000000000000000000, -0.000000000000000000, 1.000000000000000000 ) ) ;
#18865 = EDGE_CURVE ( 'NONE', #12353, #5148, #26906, .T. ) ;
#18866 = DIRECTION ( 'NONE',  ( 1.000000000000000000, 0.000000000000000000, 0.000000000000000000 ) ) ;
#18867 = EDGE_CURVE ( 'NONE', #30363, #6764, #30632, .T. ) ;
#18868 = PLANE ( 'NONE',  #6599 ) ;
#18869 = CARTESIAN_POINT ( 'NONE',  ( 18.03952607653389961, -86.20686977408767859, 12.50000000000000000 ) ) ;
#18870 = ADVANCED_FACE ( 'NONE', ( #13933 ), #19383, .F. ) ;
#18871 = ORIENTED_EDGE ( 'NONE', *, *, #3985, .T. ) ;
#18872 = LINE ( 'NONE', #30499, #15427 ) ;
#18873 = AXIS2_PLACEMENT_3D ( 'NONE', #9088, #26706, #17710 ) ;
#18874 = CARTESIAN_POINT ( 'NONE',  ( 22.99999662536857059, 77.94228634059957983, -9.999999999999998224 ) ) ;
#18875 = CARTESIAN_POINT ( 'NONE',  ( 5.122341571230610846, -2.957385285031219446, -4.281776566113608240 ) ) ;
#18876 = ORIENTED_EDGE ( 'NONE', *, *, #6849, .T. ) ;
#18877 = ORIENTED_EDGE ( 'NONE', *, *, #36750, .T. ) ;
#18878 = FACE_OUTER_BOUND ( 'NONE', #29370, .T. ) ;
#18879 = CARTESIAN_POINT ( 'NONE',  ( -5.029394918168152984, 2.903722509865296342, -4.151004066889650623 ) ) ;
#18880 = AXIS2_PLACEMENT_3D ( 'NONE', #33549, #37089, #14199 ) ;
#18881 = AXIS2_PLACEMENT_3D ( 'NONE', #10657, #30535, #10840 ) ;
#18882 = CARTESIAN_POINT ( 'NONE',  ( 39.99999662536853151, -69.28203230275519786, -9.999999999999998224 ) ) ;
#18883 = ORIENTED_EDGE ( 'NONE', *, *, #879, .F. ) ;
#18884 = CARTESIAN_POINT ( 'NONE',  ( -88.00000337463090716, -1.040834085586084257E-14, 12.50000000000000000 ) ) ;
#18885 = DIRECTION ( 'NONE',  ( 0.000000000000000000, 0.000000000000000000, -1.000000000000000000 ) ) ;
#18886 = CARTESIAN_POINT ( 'NONE',  ( -50.00000337463112032, -51.96152422706641971, 12.50000000000000000 ) ) ;
#18887 = LINE ( 'NONE', #10439, #17388 ) ;
#18888 = EDGE_CURVE ( 'NONE', #23793, #11572, #12155, .T. ) ;
#18889 = EDGE_LOOP ( 'NONE', ( #3752, #8030, #18117, #16176 ) ) ;
#18890 = ORIENTED_EDGE ( 'NONE', *, *, #12405, .F. ) ;
#18891 = CYLINDRICAL_SURFACE ( 'NONE', #36280, 2.000000000000000000 ) ;
#18892 = CIRCLE ( 'NONE', #15891, 2.000000000000001776 ) ;
#18893 = DIRECTION ( 'NONE',  ( 1.000000000000000000, 0.000000000000000000, 0.000000000000000000 ) ) ;
#18894 = VERTEX_POINT ( 'NONE', #4593 ) ;
#18895 = AXIS2_PLACEMENT_3D ( 'NONE', #22015, #13208, #13567 ) ;
#18896 = CARTESIAN_POINT ( 'NONE',  ( 62.33939050065184517, -13.89091430021398565, 12.49999999999999822 ) ) ;
#18897 = ORIENTED_EDGE ( 'NONE', *, *, #5743, .T. ) ;
#18898 = FACE_OUTER_BOUND ( 'NONE', #1163, .T. ) ;
#18899 = AXIS2_PLACEMENT_3D ( 'NONE', #24894, #36338, #18893 ) ;
#18900 = AXIS2_PLACEMENT_3D ( 'NONE', #1032, #23169, #17718 ) ;
#18901 = CIRCLE ( 'NONE', #12281, 2.000000000000001776 ) ;
#18902 = CARTESIAN_POINT ( 'NONE',  ( -17.00000337463125533, -77.94228634059960825, 17.49999999999999645 ) ) ;
#18903 = ORIENTED_EDGE ( 'NONE', *, *, #20734, .F. ) ;
#18904 = DIRECTION ( 'NONE',  ( 1.000000000000000000, 0.000000000000000000, 0.000000000000000000 ) ) ;
#18905 = VERTEX_POINT ( 'NONE', #22207 ) ;
#18906 = VECTOR ( 'NONE', #1249, 1000.000000000000000 ) ;
#18907 = AXIS2_PLACEMENT_3D ( 'NONE', #9703, #7265, #18132 ) ;
#18908 = CARTESIAN_POINT ( 'NONE',  ( 77.99999662536833966, -3.224517592124143893E-15, 12.50000000000000000 ) ) ;
#18909 = DIRECTION ( 'NONE',  ( 0.000000000000000000, 0.000000000000000000, -1.000000000000000000 ) ) ;
#18910 = LINE ( 'NONE', #10283, #28087 ) ;
#18911 = EDGE_CURVE ( 'NONE', #21307, #12339, #16577, .T. ) ;
#18912 = EDGE_LOOP ( 'NONE', ( #9978, #21496 ) ) ;
#18913 = FACE_OUTER_BOUND ( 'NONE', #12580, .T. ) ;
#18914 = CARTESIAN_POINT ( 'NONE',  ( -101.4252494179839488, 31.43181965331819683, 32.50001250000000397 ) ) ;
#18915 = DIRECTION ( 'NONE',  ( -1.000000000000000000, 0.000000000000000000, 0.000000000000000000 ) ) ;
#18916 = EDGE_LOOP ( 'NONE', ( #9452, #18346, #8314, #36962 ) ) ;
#18917 = EDGE_LOOP ( 'NONE', ( #20533, #32079, #17973, #26121 ) ) ;
#18918 = ORIENTED_EDGE ( 'NONE', *, *, #33002, .T. ) ;
#18919 = AXIS2_PLACEMENT_3D ( 'NONE', #3426, #21033, #20468 ) ;
#18920 = CARTESIAN_POINT ( 'NONE',  ( 34.99999662536855283, -60.62177826491080168, 17.49999999999999645 ) ) ;
#18921 = ORIENTED_EDGE ( 'NONE', *, *, #35261, .F. ) ;
#18922 = AXIS2_PLACEMENT_3D ( 'NONE', #3574, #23818, #35064 ) ;
#18923 = CARTESIAN_POINT ( 'NONE',  ( 34.46585318596250858, 86.45172111230321832, 12.49999999999999822 ) ) ;
#18924 = DIRECTION ( 'NONE',  ( 1.000000000000000000, 0.000000000000000000, 0.000000000000000000 ) ) ;
#18925 = AXIS2_PLACEMENT_3D ( 'NONE', #12933, #4711, #10148 ) ;
#18926 = AXIS2_PLACEMENT_3D ( 'NONE', #13377, #26909, #10387 ) ;
#18927 = FACE_OUTER_BOUND ( 'NONE', #6754, .T. ) ;
#18928 = AXIS2_PLACEMENT_3D ( 'NONE', #602, #15036, #23474 ) ;
#18929 = EDGE_CURVE ( 'NONE', #16545, #20202, #30730, .T. ) ;
#18930 = DIRECTION ( 'NONE',  ( 0.000000000000000000, 0.000000000000000000, 1.000000000000000000 ) ) ;
#18931 = CARTESIAN_POINT ( 'NONE',  ( 32.99999662536855283, -77.94228634059960825, -5.000000000000000000 ) ) ;
#18932 = DIRECTION ( 'NONE',  ( 0.000000000000000000, 0.000000000000000000, 1.000000000000000000 ) ) ;
#18933 = CIRCLE ( 'NONE', #2763, 33.00000000000001421 ) ;
#18934 = ADVANCED_FACE ( 'NONE', ( #2336 ), #7776, .F. ) ;
#18935 = DIRECTION ( 'NONE',  ( 1.000000000000000000, 0.000000000000000000, 0.000000000000000000 ) ) ;
#18936 = VERTEX_POINT ( 'NONE', #33646 ) ;
#18937 = AXIS2_PLACEMENT_3D ( 'NONE', #4462, #4284, #10100 ) ;
#18938 = EDGE_LOOP ( 'NONE', ( #8342, #29317 ) ) ;
#18939 =( LENGTH_UNIT ( ) NAMED_UNIT ( * ) SI_UNIT ( .MILLI., .METRE. ) );
#18940 = CARTESIAN_POINT ( 'NONE',  ( 39.99999662536853151, -69.28203230275519786, 17.49999999999999645 ) ) ;
#18941 = CARTESIAN_POINT ( 'NONE',  ( -10.00000337463128197, 86.60254037844397601, 12.50000000000000000 ) ) ;
#18942 = DIRECTION ( 'NONE',  ( -0.000000000000000000, -0.000000000000000000, 1.000000000000000000 ) ) ;
#18943 = EDGE_CURVE ( 'NONE', #31490, #14801, #2127, .T. ) ;
#18944 = ORIENTED_EDGE ( 'NONE', *, *, #8934, .T. ) ;
#18945 = UNCERTAINTY_MEASURE_WITH_UNIT (LENGTH_MEASURE( 1.000000000000000082E-05 ), #11779, 'distance_accuracy_value', 'NONE');
#18946 = AXIS2_PLACEMENT_3D ( 'NONE', #22805, #25611, #19611 ) ;
#18947 = CARTESIAN_POINT ( 'NONE',  ( -70.00000337463100664, -17.32050807568882078, -9.999999999999998224 ) ) ;
#18948 = DIRECTION ( 'NONE',  ( -0.000000000000000000, -0.000000000000000000, 1.000000000000000000 ) ) ;
#18949 = EDGE_CURVE ( 'NONE', #16912, #17074, #34942, .T. ) ;
#18950 = AXIS2_PLACEMENT_3D ( 'NONE', #34160, #2634, #3023 ) ;
#18951 = CARTESIAN_POINT ( 'NONE',  ( 5.000000000000000000, -0.6964580643377611402, -0.6026403643956901313 ) ) ;
#18952 = EDGE_LOOP ( 'NONE', ( #17513, #25401, #1101, #25217 ) ) ;
#18953 = AXIS2_PLACEMENT_3D ( 'NONE', #11931, #6860, #9298 ) ;
#18954 = PLANE ( 'NONE',  #24403 ) ;
#18955 = EDGE_LOOP ( 'NONE', ( #1134, #1954 ) ) ;
#18956 = AXIS2_PLACEMENT_3D ( 'NONE', #14129, #17137, #36652 ) ;
#18957 = VECTOR ( 'NONE', #22193, 1000.000000000000000 ) ;
#18958 = VECTOR ( 'NONE', #1822, 1000.000000000000000 ) ;
#18959 = CARTESIAN_POINT ( 'NONE',  ( 87.83969979969883468, 14.80603122773026037, 12.49999999999999645 ) ) ;
#18960 = AXIS2_PLACEMENT_3D ( 'NONE', #36774, #16530, #5638 ) ;
#18961 = CARTESIAN_POINT ( 'NONE',  ( 69.99999662536839651, 34.64101615137758472, 12.50000000000000000 ) ) ;
#18962 = AXIS2_PLACEMENT_3D ( 'NONE', #9087, #11525, #28783 ) ;
#18963 = CARTESIAN_POINT ( 'NONE',  ( 1.546821644788039851, 4.880444798889544522, -0.7375898304884582757 ) ) ;
#18964 = ADVANCED_FACE ( 'NONE', ( #1777 ), #27635, .F. ) ;
#18965 = ORIENTED_EDGE ( 'NONE', *, *, #9805, .F. ) ;
#18966 = VERTEX_POINT ( 'NONE', #24833 ) ;
#18968 = CIRCLE ( 'NONE', #16556, 2.000000000000001776 ) ;
#18967 = CARTESIAN_POINT ( 'NONE',  ( -52.00000337463112032, -51.96152422706641971, -9.999999999999998224 ) ) ;
#18969 = ORIENTED_EDGE ( 'NONE', *, *, #34824, .F. ) ;
#18970 = DIRECTION ( 'NONE',  ( 1.000000000000000000, 0.000000000000000000, 0.000000000000000000 ) ) ;
#18971 = CARTESIAN_POINT ( 'NONE',  ( 79.99999662536833966, 34.64101615137759183, -9.999999999999998224 ) ) ;
#18972 = CARTESIAN_POINT ( 'NONE',  ( -73.00000337463097821, -8.660254037844422825, 12.50000000000000000 ) ) ;
#18973 = DIRECTION ( 'NONE',  ( -1.000000000000000000, 0.000000000000000000, -0.000000000000000000 ) ) ;
#18974 = CYLINDRICAL_SURFACE ( 'NONE', #34522, 3.499999999999989342 ) ;
#18975 = EDGE_LOOP ( 'NONE', ( #36423, #1859 ) ) ;
#18976 = FACE_OUTER_BOUND ( 'NONE', #17968, .T. ) ;
#18977 = AXIS2_PLACEMENT_3D ( 'NONE', #31348, #4939, #30998 ) ;
#18978 = EDGE_CURVE ( 'NONE', #10304, #24755, #4784, .T. ) ;
#18979 = DIRECTION ( 'NONE',  ( 0.000000000000000000, 0.000000000000000000, 1.000000000000000000 ) ) ;
#18980 = CONICAL_SURFACE ( 'NONE', #5217, 20.00000000000001066, 0.1396263401595466691 ) ;
#18981 = EDGE_CURVE ( 'NONE', #10475, #7880, #24654, .T. ) ;
#18982 = ORIENTED_EDGE ( 'NONE', *, *, #31619, .T. ) ;
#18983 = CARTESIAN_POINT ( 'NONE',  ( -80.00000337463094979, -2.428612866367529932E-14, -9.999999999999998224 ) ) ;
#18984 = DIRECTION ( 'NONE',  ( 0.000000000000000000, 0.000000000000000000, 1.000000000000000000 ) ) ;
#18985 = DIRECTION ( 'NONE',  ( 0.000000000000000000, 0.000000000000000000, 1.000000000000000000 ) ) ;
#18986 = ORIENTED_EDGE ( 'NONE', *, *, #5453, .T. ) ;
#18987 = EDGE_CURVE ( 'NONE', #12004, #17325, #6183, .T. ) ;
#18988 = AXIS2_PLACEMENT_3D ( 'NONE', #9014, #28508, #573 ) ;
#18989 = ORIENTED_EDGE ( 'NONE', *, *, #2094, .F. ) ;
#18990 = PLANE ( 'NONE',  #21706 ) ;
#18991 = CYLINDRICAL_SURFACE ( 'NONE', #35560, 2.000000000000001776 ) ;
#18992 = CARTESIAN_POINT ( 'NONE',  ( -2.255011273957059359, -4.471571325851515510, -0.5083873451168858804 ) ) ;
#18993 = EDGE_CURVE ( 'NONE', #26245, #26119, #33139, .T. ) ;
#18994 = ORIENTED_EDGE ( 'NONE', *, *, #27203, .T. ) ;
#18995 = VERTEX_POINT ( 'NONE', #33466 ) ;
#18996 = ORIENTED_EDGE ( 'NONE', *, *, #24767, .F. ) ;
#18997 = VECTOR ( 'NONE', #30010, 1000.000000000000000 ) ;
#18998 = DIRECTION ( 'NONE',  ( 0.000000000000000000, 0.000000000000000000, 1.000000000000000000 ) ) ;
#18999 = EDGE_CURVE ( 'NONE', #29382, #6775, #22356, .T. ) ;
#19000 = EDGE_LOOP ( 'NONE', ( #3820, #18069 ) ) ;
#19001 = AXIS2_PLACEMENT_3D ( 'NONE', #16975, #28233, #14162 ) ;
#19002 = DIRECTION ( 'NONE',  ( 0.000000000000000000, 0.000000000000000000, -1.000000000000000000 ) ) ;
#19003 = ORIENTED_EDGE ( 'NONE', *, *, #22172, .T. ) ;
#19004 = CIRCLE ( 'NONE', #25585, 4.749999999999999112 ) ;
#19005 = VERTEX_POINT ( 'NONE', #31008 ) ;
#19006 = CARTESIAN_POINT ( 'NONE',  ( -4.279621169095561228, 62.97617850287782915, -49.86561046011506448 ) ) ;
#19007 = VECTOR ( 'NONE', #6483, 1000.000000000000000 ) ;
#19008 = CARTESIAN_POINT ( 'NONE',  ( -43.00000337463111322, 77.94228634059959404, -9.999999999999998224 ) ) ;
#19009 = VERTEX_POINT ( 'NONE', #10384 ) ;
#19010 = ORIENTED_EDGE ( 'NONE', *, *, #26390, .T. ) ;
#19011 = DIRECTION ( 'NONE',  ( -1.000000000000000000, 0.000000000000000000, 0.000000000000000000 ) ) ;
#19012 = DIRECTION ( 'NONE',  ( 0.000000000000000000, 0.000000000000000000, 1.000000000000000000 ) ) ;
#19013 = CARTESIAN_POINT ( 'NONE',  ( -70.00000337463099243, -2.428612866367529932E-14, -9.999999999999998224 ) ) ;
#19014 = AXIS2_PLACEMENT_3D ( 'NONE', #19793, #5532, #16960 ) ;
#19015 = CIRCLE ( 'NONE', #30375, 27.00000000000001421 ) ;
#19016 = LINE ( 'NONE', #1761, #8477 ) ;
#19017 = DIRECTION ( 'NONE',  ( 0.000000000000000000, 0.000000000000000000, 1.000000000000000000 ) ) ;
#19018 = EDGE_CURVE ( 'NONE', #19694, #29078, #24151, .T. ) ;
#19019 = EDGE_LOOP ( 'NONE', ( #32982, #20515 ) ) ;
#19020 = DIRECTION ( 'NONE',  ( 0.000000000000000000, 0.000000000000000000, 1.000000000000000000 ) ) ;
#19021 = FACE_BOUND ( 'NONE', #1453, .T. ) ;
#19022 = DIRECTION ( 'NONE',  ( 0.000000000000000000, 0.000000000000000000, 1.000000000000000000 ) ) ;
#19023 = CYLINDRICAL_SURFACE ( 'NONE', #5231, 2.000000000000001776 ) ;
#19024 = CIRCLE ( 'NONE', #30976, 27.00000000000001421 ) ;
#19025 = CARTESIAN_POINT ( 'NONE',  ( 4.999996625368676284, -77.94228634059960825, -9.999999999999998224 ) ) ;
#19026 = CYLINDRICAL_SURFACE ( 'NONE', #27845, 2.000000000000001776 ) ;
#19027 = EDGE_CURVE ( 'NONE', #31926, #26476, #2512, .T. ) ;
#19028 = DIRECTION ( 'NONE',  ( -1.000000000000000000, 0.000000000000000000, 0.000000000000000000 ) ) ;
#19029 = AXIS2_PLACEMENT_3D ( 'NONE', #30124, #30319, #1642 ) ;
#19030 = EDGE_CURVE ( 'NONE', #7462, #9506, #29540, .T. ) ;
#19031 = DIRECTION ( 'NONE',  ( 0.000000000000000000, 0.000000000000000000, 1.000000000000000000 ) ) ;
#19032 = ORIENTED_EDGE ( 'NONE', *, *, #32885, .T. ) ;
#19033 = DIRECTION ( 'NONE',  ( -0.000000000000000000, -0.000000000000000000, 1.000000000000000000 ) ) ;
#19034 = EDGE_CURVE ( 'NONE', #357, #36483, #13383, .T. ) ;
#19035 = CIRCLE ( 'NONE', #10060, 2.000000000000001776 ) ;
#19036 = AXIS2_PLACEMENT_3D ( 'NONE', #2121, #28186, #16931 ) ;
#19037 = FACE_OUTER_BOUND ( 'NONE', #18589, .T. ) ;
#19038 = DIRECTION ( 'NONE',  ( 0.000000000000000000, 0.000000000000000000, 1.000000000000000000 ) ) ;
#19039 = B_SPLINE_CURVE_WITH_KNOTS ( 'NONE', 3,
 ( #3443, #26483, #793, #14877, #626, #23674, #18051, #29471 ),
 .UNSPECIFIED., .F., .F.,
 ( 4, 2, 2, 4 ),
 ( 2.451332856729116966E-07, 0.001475502392055643005, 0.002213131021440628045, 0.002950759650825612868 ),
 .UNSPECIFIED. ) ;
#19040 = CIRCLE ( 'NONE', #1654, 0.2999999999999999334 ) ;
#19041 = ORIENTED_EDGE ( 'NONE', *, *, #22493, .F. ) ;
#19042 = ORIENTED_EDGE ( 'NONE', *, *, #34294, .T. ) ;
#19043 = ORIENTED_EDGE ( 'NONE', *, *, #35816, .T. ) ;
#19044 = AXIS2_PLACEMENT_3D ( 'NONE', #15424, #35320, #11854 ) ;
#19045 = CARTESIAN_POINT ( 'NONE',  ( -67.00000337463106348, -60.62177826491083010, -9.999999999999998224 ) ) ;
#19046 = FACE_OUTER_BOUND ( 'NONE', #35461, .T. ) ;
#19047 = VERTEX_POINT ( 'NONE', #31358 ) ;
#19048 = DIRECTION ( 'NONE',  ( -1.000000000000000000, 0.000000000000000000, 0.000000000000000000 ) ) ;
#19049 = ADVANCED_FACE ( 'NONE', ( #420 ), #29094, .T. ) ;
#19050 = CARTESIAN_POINT ( 'NONE',  ( 80.69570903995992239, -15.44541228182033699, -5.000000000000000000 ) ) ;
#19051 = VERTEX_POINT ( 'NONE', #3072 ) ;
#19052 = CARTESIAN_POINT ( 'NONE',  ( -124.4080600076932370, -12.15049814296501829, 32.50002500000000083 ) ) ;
#19053 = EDGE_LOOP ( 'NONE', ( #12523, #13142, #5399, #14935 ) ) ;
#19054 = FACE_BOUND ( 'NONE', #19589, .T. ) ;
#19055 = AXIS2_PLACEMENT_3D ( 'NONE', #8911, #6652, #8717 ) ;
#19056 = CARTESIAN_POINT ( 'NONE',  ( -73.00000337463097821, -8.660254037844422825, 17.49999999999999645 ) ) ;
#19057 = CARTESIAN_POINT ( 'NONE',  ( -43.00000337463111322, 60.62177826491077326, -9.999999999999998224 ) ) ;
#19058 = AXIS2_PLACEMENT_3D ( 'NONE', #961, #35301, #20096 ) ;
#19059 = CARTESIAN_POINT ( 'NONE',  ( -4.749999999999999112, 0.000000000000000000, 0.000000000000000000 ) ) ;
#19060 = ORIENTED_EDGE ( 'NONE', *, *, #26399, .T. ) ;
#19061 = CARTESIAN_POINT ( 'NONE',  ( 17.99999662536861678, -69.28203230275519786, -9.999999999999998224 ) ) ;
#19062 = CIRCLE ( 'NONE', #4088, 2.000000000000001776 ) ;
#19063 = VECTOR ( 'NONE', #2586, 1000.000000000000000 ) ;
#19064 = CARTESIAN_POINT ( 'NONE',  ( 6.000000000000000000, 5.000000000000000000, 0.000000000000000000 ) ) ;
#19065 = LINE ( 'NONE', #27838, #2602 ) ;
#19066 = ADVANCED_FACE ( 'NONE', ( #61 ), #3431, .F. ) ;
#19067 = AXIS2_PLACEMENT_3D ( 'NONE', #26616, #9013, #26818 ) ;
#19068 = ORIENTED_EDGE ( 'NONE', *, *, #13848, .T. ) ;
#19069 = FACE_BOUND ( 'NONE', #28112, .T. ) ;
#19070 = LINE ( 'NONE', #24688, #2384 ) ;
#19071 = ORIENTED_EDGE ( 'NONE', *, *, #3960, .F. ) ;
#19072 = EDGE_CURVE ( 'NONE', #5817, #5072, #13976, .T. ) ;
#19073 = CYLINDRICAL_SURFACE ( 'NONE', #20790, 2.000000000000001776 ) ;
#19074 = DIRECTION ( 'NONE',  ( 1.000000000000000000, 0.000000000000000000, 0.000000000000000000 ) ) ;
#19075 = LINE ( 'NONE', #1985, #23153 ) ;
#19076 = EDGE_CURVE ( 'NONE', #9332, #34006, #7406, .T. ) ;
#19077 = AXIS2_PLACEMENT_3D ( 'NONE', #28656, #2796, #28828 ) ;
#19078 = ORIENTED_EDGE ( 'NONE', *, *, #14576, .T. ) ;
#19079 = VERTEX_POINT ( 'NONE', #26109 ) ;
#19080 = EDGE_CURVE ( 'NONE', #27157, #31151, #18174, .T. ) ;
#19081 = DIRECTION ( 'NONE',  ( 1.000000000000000000, 0.000000000000000000, 0.000000000000000000 ) ) ;
#19082 = CIRCLE ( 'NONE', #34045, 2.000000000000001776 ) ;
#19083 = CARTESIAN_POINT ( 'NONE',  ( -62.97617850287781494, -4.279621169095772615, -4.999999999999997335 ) ) ;
#19084 = EDGE_CURVE ( 'NONE', #8433, #25339, #28746, .T. ) ;
#19085 = DIRECTION ( 'NONE',  ( 0.000000000000000000, 0.000000000000000000, 1.000000000000000000 ) ) ;
#19086 = ORIENTED_EDGE ( 'NONE', *, *, #13306, .F. ) ;
#19087 = VERTEX_POINT ( 'NONE', #19771 ) ;
#19088 = AXIS2_PLACEMENT_3D ( 'NONE', #9348, #26042, #14600 ) ;
#19089 = CARTESIAN_POINT ( 'NONE',  ( 0.000000000000000000, 0.000000000000000000, -5.000000000000000000 ) ) ;
#19090 = CARTESIAN_POINT ( 'NONE',  ( -67.00000337463104927, -25.98076211353322051, 12.50000000000000000 ) ) ;
#19091 = AXIS2_PLACEMENT_3D ( 'NONE', #19882, #14612, #11983 ) ;
#19092 = CARTESIAN_POINT ( 'NONE',  ( 67.99999662536838230, 17.32050807568879236, 17.49999999999999645 ) ) ;
#19093 = CARTESIAN_POINT ( 'NONE',  ( -107.0734680828344096, 50.67989423971658169, 32.50000000000000000 ) ) ;
#19094 = EDGE_CURVE ( 'NONE', #33342, #22833, #16981, .T. ) ;
#19095 = ORIENTED_EDGE ( 'NONE', *, *, #28255, .T. ) ;
#19096 = VECTOR ( 'NONE', #22413, 1000.000000000000000 ) ;
#19098 = ORIENTED_EDGE ( 'NONE', *, *, #26869, .T. ) ;
#19097 = EDGE_CURVE ( 'NONE', #19686, #21619, #3800, .T. ) ;
#19099 = CARTESIAN_POINT ( 'NONE',  ( 4.999999999999999112, 0.4965892259340526915, -0.01450341304856531295 ) ) ;
#19100 = CIRCLE ( 'NONE', #28650, 2.000000000000001776 ) ;
#19101 = EDGE_CURVE ( 'NONE', #21726, #8370, #7990, .T. ) ;
#19102 = DIRECTION ( 'NONE',  ( -1.000000000000000000, 0.000000000000000000, 0.000000000000000000 ) ) ;
#19104 = EDGE_CURVE ( 'NONE', #13211, #1000, #34249, .T. ) ;
#19103 = ORIENTED_EDGE ( 'NONE', *, *, #18238, .F. ) ;
#19105 = CARTESIAN_POINT ( 'NONE',  ( 5.000000000000000000, 30.00000000000000355, -15.00000000000000000 ) ) ;
#19106 = ORIENTED_EDGE ( 'NONE', *, *, #18112, .F. ) ;
#19107 = LINE ( 'NONE', #19277, #12317 ) ;
#19108 = CIRCLE ( 'NONE', #19766, 6.000000000000005329 ) ;
#19109 = CIRCLE ( 'NONE', #21473, 150.0000000000000284 ) ;
#19110 = DIRECTION ( 'NONE',  ( -1.000000000000000000, 0.000000000000000000, 0.000000000000000000 ) ) ;
#19111 = DIRECTION ( 'NONE',  ( 0.000000000000000000, 0.000000000000000000, 1.000000000000000000 ) ) ;
#19112 = ORIENTED_EDGE ( 'NONE', *, *, #12739, .F. ) ;
#19113 = PRODUCT_DEFINITION_SHAPE ( 'NONE', 'NONE',  #37112 ) ;
#19114 = DIRECTION ( 'NONE',  ( 0.000000000000000000, 0.5000000000000013323, 0.8660254037844378194 ) ) ;
#19115 = CIRCLE ( 'NONE', #16726, 3.000000000000004885 ) ;
#19116 = DIRECTION ( 'NONE',  ( 1.000000000000000000, 0.000000000000000000, 0.000000000000000000 ) ) ;
#19117 = DIRECTION ( 'NONE',  ( 0.000000000000000000, 0.000000000000000000, 1.000000000000000000 ) ) ;
#19118 = ORIENTED_EDGE ( 'NONE', *, *, #21138, .F. ) ;
#19119 = CARTESIAN_POINT ( 'NONE',  ( 0.000000000000000000, 0.000000000000000000, -5.000000000000000000 ) ) ;
#19120 = AXIS2_PLACEMENT_3D ( 'NONE', #31431, #34996, #17551 ) ;
#19121 = DIRECTION ( 'NONE',  ( 1.000000000000000000, 0.000000000000000000, 0.000000000000000000 ) ) ;
#19122 = CARTESIAN_POINT ( 'NONE',  ( 35.99999999999999289, 0.000000000000000000, 2.445500000000000007 ) ) ;
#19123 = ORIENTED_EDGE ( 'NONE', *, *, #9576, .F. ) ;
#19124 = EDGE_CURVE ( 'NONE', #13703, #23401, #14561, .T. ) ;
#19125 = EDGE_LOOP ( 'NONE', ( #4861, #13024, #25977, #3738, #1378, #8699, #11498, #6913, #5297, #10714, #10305, #19071, #13845, #14984 ) ) ;
#19126 = ORIENTED_EDGE ( 'NONE', *, *, #27061, .F. ) ;
#19127 = VECTOR ( 'NONE', #30817, 1000.000000000000000 ) ;
#19128 = DIRECTION ( 'NONE',  ( 1.000000000000000000, 0.000000000000000000, 0.000000000000000000 ) ) ;
#19129 = ORIENTED_EDGE ( 'NONE', *, *, #20881, .F. ) ;
#19130 = DIRECTION ( 'NONE',  ( -0.000000000000000000, -0.000000000000000000, -1.000000000000000000 ) ) ;
#19131 = CARTESIAN_POINT ( 'NONE',  ( 47.99999662536846756, -69.28203230275519786, -9.999999999999998224 ) ) ;
#19132 = VECTOR ( 'NONE', #33005, 1000.000000000000000 ) ;
#19133 = CYLINDRICAL_SURFACE ( 'NONE', #35989, 1.999999999999998224 ) ;
#19134 = VECTOR ( 'NONE', #2761, 1000.000000000000000 ) ;
#19135 = DIRECTION ( 'NONE',  ( -0.000000000000000000, -0.000000000000000000, 1.000000000000000000 ) ) ;
#19136 = VECTOR ( 'NONE', #32138, 1000.000000000000000 ) ;
#19137 = DIRECTION ( 'NONE',  ( 0.000000000000000000, 0.000000000000000000, -1.000000000000000000 ) ) ;
#19138 = FACE_OUTER_BOUND ( 'NONE', #26749, .T. ) ;
#19139 = CARTESIAN_POINT ( 'NONE',  ( -6.069707180676227632E-15, 5.773502691896269745, -4.069520038198747081 ) ) ;
#19140 = LINE ( 'NONE', #30564, #26229 ) ;
#19141 = ORIENTED_EDGE ( 'NONE', *, *, #3341, .F. ) ;
#19142 = ORIENTED_EDGE ( 'NONE', *, *, #28274, .F. ) ;
#19143 = CIRCLE ( 'NONE', #7756, 2.000000000000001776 ) ;
#19144 = CARTESIAN_POINT ( 'NONE',  ( 52.39915983220795681, 35.19434990244919703, 12.49999999999999822 ) ) ;
#19145 = EDGE_CURVE ( 'NONE', #20765, #12599, #803, .T. ) ;
#19146 = DIRECTION ( 'NONE',  ( -1.000000000000000000, 0.000000000000000000, 0.000000000000000000 ) ) ;
#19147 = FACE_OUTER_BOUND ( 'NONE', #9305, .T. ) ;
#19148 = ORIENTED_EDGE ( 'NONE', *, *, #17858, .T. ) ;
#19149 = AXIS2_PLACEMENT_3D ( 'NONE', #28178, #5324, #5119 ) ;
#19150 = DIRECTION ( 'NONE',  ( 0.000000000000000000, 0.000000000000000000, 1.000000000000000000 ) ) ;
#19151 = CARTESIAN_POINT ( 'NONE',  ( -65.00000000000000000, 0.000000000000000000, -5.000000000000000000 ) ) ;
#19152 = ORIENTED_EDGE ( 'NONE', *, *, #6710, .T. ) ;
#19153 = CARTESIAN_POINT ( 'NONE',  ( -85.00000337463092137, -25.98076211353322051, -9.999999999999998224 ) ) ;
#19154 = EDGE_LOOP ( 'NONE', ( #25897, #14683 ) ) ;
#19155 = AXIS2_PLACEMENT_3D ( 'NONE', #17731, #35192, #23940 ) ;
#19156 = DIRECTION ( 'NONE',  ( 1.000000000000000000, 0.000000000000000000, 0.000000000000000000 ) ) ;
#19157 = DIRECTION ( 'NONE',  ( 1.000000000000000000, 0.000000000000000000, 0.000000000000000000 ) ) ;
#19158 = CARTESIAN_POINT ( 'NONE',  ( 44.99999662536851019, 77.94228634059959404, -9.999999999999998224 ) ) ;
#19159 = VERTEX_POINT ( 'NONE', #31893 ) ;
#19160 = EDGE_LOOP ( 'NONE', ( #29758, #8605, #28269, #22702 ) ) ;
#19161 = CIRCLE ( 'NONE', #10777, 2.000000000000001776 ) ;
#19162 = EDGE_CURVE ( 'NONE', #33879, #36954, #17319, .T. ) ;
#19163 = ADVANCED_FACE ( 'NONE', ( #6227 ), #25769, .F. ) ;
#19164 = ORIENTED_EDGE ( 'NONE', *, *, #9881, .F. ) ;
#19165 = DIRECTION ( 'NONE',  ( 1.000000000000000000, 0.000000000000000000, 0.000000000000000000 ) ) ;
#19166 = AXIS2_PLACEMENT_3D ( 'NONE', #21859, #4984, #36308 ) ;
#19167 = CARTESIAN_POINT ( 'NONE',  ( 9.999996625368655856, -69.28203230275519786, -9.999999999999998224 ) ) ;
#19168 = EDGE_CURVE ( 'NONE', #22389, #13276, #31194, .T. ) ;
#19169 = AXIS2_PLACEMENT_3D ( 'NONE', #21904, #4858, #36709 ) ;
#19170 = CYLINDRICAL_SURFACE ( 'NONE', #13049, 2.000000000000000000 ) ;
#19171 = DIRECTION ( 'NONE',  ( -1.000000000000000000, 0.000000000000000000, 0.000000000000000000 ) ) ;
#19172 = CARTESIAN_POINT ( 'NONE',  ( 19.99999662536861678, -86.60254037844400443, 12.50000000000000000 ) ) ;
#19173 = EDGE_LOOP ( 'NONE', ( #14602, #19875, #35034, #30811 ) ) ;
#19174 = CARTESIAN_POINT ( 'NONE',  ( -43.00000337463111322, 77.94228634059959404, -9.999999999999998224 ) ) ;
#19175 = DIRECTION ( 'NONE',  ( 1.000000000000000000, 0.000000000000000000, 0.000000000000000000 ) ) ;
#19176 = EDGE_CURVE ( 'NONE', #17536, #18182, #36738, .T. ) ;
#19177 = DIRECTION ( 'NONE',  ( -0.000000000000000000, -0.000000000000000000, 1.000000000000000000 ) ) ;
#19178 = ORIENTED_EDGE ( 'NONE', *, *, #34671, .T. ) ;
#19179 = DIRECTION ( 'NONE',  ( 1.000000000000000000, 0.000000000000000000, 0.000000000000000000 ) ) ;
#19180 = DIRECTION ( 'NONE',  ( -0.000000000000000000, -0.000000000000000000, 1.000000000000000000 ) ) ;
#19181 = AXIS2_PLACEMENT_3D ( 'NONE', #13393, #24110, #24851 ) ;
#19182 = EDGE_LOOP ( 'NONE', ( #9872, #23941, #23226, #30892, #18377, #13215, #23783, #7887, #13319, #9793 ) ) ;
#19183 = ORIENTED_EDGE ( 'NONE', *, *, #30935, .F. ) ;
#19184 = CARTESIAN_POINT ( 'NONE',  ( -1.598077599634237123, 4.850852159561235055, -3.971474537231017621 ) ) ;
#19185 = AXIS2_PLACEMENT_3D ( 'NONE', #14863, #20114, #3071 ) ;
#19186 = EDGE_CURVE ( 'NONE', #29302, #3947, #17861, .T. ) ;
#19187 = CARTESIAN_POINT ( 'NONE',  ( 108.3061974404898820, 19.22934205794938478, 27.50000000000000000 ) ) ;
#19188 = CARTESIAN_POINT ( 'NONE',  ( -75.00000337463097821, 8.660254037844374864, 12.50000000000000000 ) ) ;
#19189 = ORIENTED_EDGE ( 'NONE', *, *, #29549, .F. ) ;
#19190 = ORIENTED_EDGE ( 'NONE', *, *, #36558, .T. ) ;
#19191 =( GEOMETRIC_REPRESENTATION_CONTEXT ( 3 ) GLOBAL_UNCERTAINTY_ASSIGNED_CONTEXT ( ( #36575 ) ) GLOBAL_UNIT_ASSIGNED_CONTEXT ( ( #26051, #31307, #31681 ) ) REPRESENTATION_CONTEXT ( 'NONE', 'WORKASPACE' ) );
#19192 = CARTESIAN_POINT ( 'NONE',  ( 71.99999662536838230, -51.96152422706639840, -9.999999999999998224 ) ) ;
#19193 = AXIS2_PLACEMENT_3D ( 'NONE', #23579, #32199, #26219 ) ;
#19194 = ORIENTED_EDGE ( 'NONE', *, *, #6849, .F. ) ;
#19195 = VECTOR ( 'NONE', #23952, 1000.000000000000000 ) ;
#19196 = CARTESIAN_POINT ( 'NONE',  ( -22.00000337463124112, 69.28203230275516944, 12.50000000000000000 ) ) ;
#19197 = ORIENTED_EDGE ( 'NONE', *, *, #25601, .F. ) ;
#19198 = ORIENTED_EDGE ( 'NONE', *, *, #25254, .F. ) ;
#19199 = CARTESIAN_POINT ( 'NONE',  ( -75.00000337463097821, 8.660254037844374864, -5.000000000000000000 ) ) ;
#19200 = EDGE_CURVE ( 'NONE', #16532, #19694, #17555, .T. ) ;
#19201 = DIRECTION ( 'NONE',  ( 0.000000000000000000, 0.000000000000000000, 1.000000000000000000 ) ) ;
#19202 = EDGE_LOOP ( 'NONE', ( #13661, #26207, #6318, #34933 ) ) ;
#19203 = CIRCLE ( 'NONE', #23984, 5.000000000000000888 ) ;
#19204 = ORIENTED_EDGE ( 'NONE', *, *, #3904, .F. ) ;
#19205 = CARTESIAN_POINT ( 'NONE',  ( -62.33939050065184517, 13.89091430021398565, 12.49999999999999822 ) ) ;
#19206 = DIRECTION ( 'NONE',  ( 0.000000000000000000, 0.000000000000000000, 1.000000000000000000 ) ) ;
#19207 = LINE ( 'NONE', #28180, #16879 ) ;
#19208 = CYLINDRICAL_SURFACE ( 'NONE', #12489, 2.000000000000000000 ) ;
#19209 = ORIENTED_EDGE ( 'NONE', *, *, #14247, .T. ) ;
#19210 = CYLINDRICAL_SURFACE ( 'NONE', #27926, 2.000000000000001776 ) ;
#19211 = CIRCLE ( 'NONE', #11402, 5.000000000000000000 ) ;
#19212 = FACE_BOUND ( 'NONE', #14167, .T. ) ;
#19213 = EDGE_CURVE ( 'NONE', #18148, #33445, #36152, .T. ) ;
#19214 = CARTESIAN_POINT ( 'NONE',  ( 66.99999662536841072, -25.98076211353320275, -9.999999999999998224 ) ) ;
#19215 = CIRCLE ( 'NONE', #3544, 2.000000000000001776 ) ;
#19216 = CARTESIAN_POINT ( 'NONE',  ( -10.21421600225141724, -84.61404523131187716, 12.50000000000000000 ) ) ;
#19217 = DIRECTION ( 'NONE',  ( 0.000000000000000000, 0.000000000000000000, 1.000000000000000000 ) ) ;
#19218 = DIRECTION ( 'NONE',  ( 0.000000000000000000, 0.000000000000000000, 1.000000000000000000 ) ) ;
#19219 = CARTESIAN_POINT ( 'NONE',  ( 21.38228493551344300, 108.2013385194334489, 27.49998799999999832 ) ) ;
#19220 = ADVANCED_FACE ( 'NONE', ( #15422 ), #32290, .F. ) ;
#19221 = CARTESIAN_POINT ( 'NONE',  ( 19.99999662536857770, 86.60254037844397601, 17.49999999999999645 ) ) ;
#19222 = EDGE_LOOP ( 'NONE', ( #20838, #2523, #22520, #1211 ) ) ;
#19223 = LINE ( 'NONE', #16031, #22584 ) ;
#19224 = DIRECTION ( 'NONE',  ( -1.000000000000000000, -0.000000000000000000, -0.000000000000000000 ) ) ;
#19225 = CARTESIAN_POINT ( 'NONE',  ( -37.00000337463117717, -77.94228634059963667, -9.999999999999998224 ) ) ;
#19226 = ORIENTED_EDGE ( 'NONE', *, *, #14504, .T. ) ;
#19227 = VERTEX_POINT ( 'NONE', #26860 ) ;
#19228 = ORIENTED_EDGE ( 'NONE', *, *, #23638, .T. ) ;
#19229 = CARTESIAN_POINT ( 'NONE',  ( -70.80619744048887299, 84.18124734178336155, 32.50000000000000000 ) ) ;
#19230 = FACE_OUTER_BOUND ( 'NONE', #8871, .T. ) ;
#19231 = ORIENTED_EDGE ( 'NONE', *, *, #4124, .T. ) ;
#19232 = DIRECTION ( 'NONE',  ( 0.000000000000000000, 1.000000000000000000, -1.625241993126352989E-15 ) ) ;
#19233 = EDGE_CURVE ( 'NONE', #29485, #12226, #34924, .T. ) ;
#19234 = DIRECTION ( 'NONE',  ( 1.000000000000000000, 0.000000000000000000, 0.000000000000000000 ) ) ;
#19235 = ORIENTED_EDGE ( 'NONE', *, *, #28610, .T. ) ;
#19236 = CARTESIAN_POINT ( 'NONE',  ( -23.00000337463121980, -77.94228634059963667, -9.999999999999998224 ) ) ;
#19237 = ORIENTED_EDGE ( 'NONE', *, *, #6102, .F. ) ;
#19238 = DIRECTION ( 'NONE',  ( 0.000000000000000000, 0.000000000000000000, 1.000000000000000000 ) ) ;
#19239 = EDGE_CURVE ( 'NONE', #19877, #17193, #15775, .T. ) ;
#19240 = CARTESIAN_POINT ( 'NONE',  ( 145.0000000000000853, 5.999999999999493738, 27.50000000000000000 ) ) ;
#19241 = CARTESIAN_POINT ( 'NONE',  ( 14.99999662536859901, 77.94228634059957983, -9.999999999999998224 ) ) ;
#19242 = EDGE_CURVE ( 'NONE', #3733, #24428, #1176, .T. ) ;
#19243 = EDGE_LOOP ( 'NONE', ( #21965, #8197 ) ) ;
#19244 = CARTESIAN_POINT ( 'NONE',  ( 3.000000000000000000, 0.000000000000000000, 0.000000000000000000 ) ) ;
#19245 = ITEM_DEFINED_TRANSFORMATION ( 'NONE', 'NONE', #15983,  #21385 ) ;
#19246 = DIRECTION ( 'NONE',  ( 0.000000000000000000, 0.000000000000000000, 1.000000000000000000 ) ) ;
#19247 = CARTESIAN_POINT ( 'NONE',  ( 95.00000000000000000, 1.163414459189985643E-14, 17.49999999999999645 ) ) ;
#19248 = ORIENTED_EDGE ( 'NONE', *, *, #18347, .F. ) ;
#19249 = FACE_BOUND ( 'NONE', #32350, .T. ) ;
#19250 = CARTESIAN_POINT ( 'NONE',  ( -14.80603122773057478, 87.83969979969877784, -4.999999999999997335 ) ) ;
#19251 = ORIENTED_EDGE ( 'NONE', *, *, #14597, .T. ) ;
#19252 = FACE_OUTER_BOUND ( 'NONE', #10193, .T. ) ;
#19253 = CIRCLE ( 'NONE', #22242, 2.000000000000001776 ) ;
#19254 = CARTESIAN_POINT ( 'NONE',  ( -31.83425564451526668, -89.42901512340343118, 12.49999999999999822 ) ) ;
#19255 = CYLINDRICAL_SURFACE ( 'NONE', #21357, 2.000000000000001776 ) ;
#19256 = ORIENTED_EDGE ( 'NONE', *, *, #25844, .F. ) ;
#19257 = ADVANCED_FACE ( 'NONE', ( #32858 ), #12196, .F. ) ;
#19258 = ORIENTED_EDGE ( 'NONE', *, *, #22238, .T. ) ;
#19259 = CARTESIAN_POINT ( 'NONE',  ( -56.67878100130369035, 27.78182860042797131, -4.999999999999997335 ) ) ;
#19260 = DIRECTION ( 'NONE',  ( 0.000000000000000000, 0.000000000000000000, 1.000000000000000000 ) ) ;
#19261 = CARTESIAN_POINT ( 'NONE',  ( 51.13139720814417899, 27.49999999999988987, -10.00000000000000000 ) ) ;
#19262 = ORIENTED_EDGE ( 'NONE', *, *, #15609, .F. ) ;
#19263 = EDGE_LOOP ( 'NONE', ( #16295, #27704 ) ) ;
#19264 = DIRECTION ( 'NONE',  ( 0.000000000000000000, 0.000000000000000000, 1.000000000000000000 ) ) ;
#19265 = DIRECTION ( 'NONE',  ( 1.000000000000000000, 0.000000000000000000, 0.000000000000000000 ) ) ;
#19266 = DIRECTION ( 'NONE',  ( -1.000000000000000000, -0.000000000000000000, -0.000000000000000000 ) ) ;
#19267 = CARTESIAN_POINT ( 'NONE',  ( -105.5600153471429081, 56.84082786873509008, 32.50000000000000711 ) ) ;
#19268 = VERTEX_POINT ( 'NONE', #21215 ) ;
#19269 = ORIENTED_EDGE ( 'NONE', *, *, #15628, .T. ) ;
#19270 = EDGE_CURVE ( 'NONE', #14483, #34280, #9798, .T. ) ;
#19271 = FACE_OUTER_BOUND ( 'NONE', #25316, .T. ) ;
#19272 = ORIENTED_EDGE ( 'NONE', *, *, #4492, .F. ) ;
#19273 = ADVANCED_FACE ( 'NONE', ( #617 ), #1424, .T. ) ;
#19274 = FACE_BOUND ( 'NONE', #29998, .T. ) ;
#19275 = ORIENTED_EDGE ( 'NONE', *, *, #19742, .T. ) ;
#19276 = AXIS2_PLACEMENT_3D ( 'NONE', #19900, #5846, #14284 ) ;
#19277 = CARTESIAN_POINT ( 'NONE',  ( 52.99999662536844625, 43.30127018922198801, -9.999999999999998224 ) ) ;
#19278 = MANIFOLD_SOLID_BREP ( 'Hex', #32750 ) ;
#19279 = ADVANCED_FACE ( 'NONE', ( #1346 ), #18041, .T. ) ;
#19280 = DIRECTION ( 'NONE',  ( -1.000000000000000000, 0.000000000000000000, 0.000000000000000000 ) ) ;
#19281 = ADVANCED_FACE ( 'NONE', ( #32467 ), #33768, .F. ) ;
#19282 = CARTESIAN_POINT ( 'NONE',  ( 0.000000000000000000, 0.000000000000000000, 15.00000000000000000 ) ) ;
#19283 = ORIENTED_EDGE ( 'NONE', *, *, #32427, .F. ) ;
#19284 = ADVANCED_FACE ( 'NONE', ( #18214 ), #30408, .F. ) ;
#19285 = SURFACE_STYLE_USAGE ( .BOTH. , #1459 ) ;
#19286 = DIRECTION ( 'NONE',  ( 1.000000000000000000, 0.000000000000000000, 0.000000000000000000 ) ) ;
#19287 = DIRECTION ( 'NONE',  ( 0.000000000000000000, 0.000000000000000000, -1.000000000000000000 ) ) ;
#19288 = DIRECTION ( 'NONE',  ( -1.000000000000000000, 0.000000000000000000, -0.000000000000000000 ) ) ;
#19289 = ORIENTED_EDGE ( 'NONE', *, *, #28453, .F. ) ;
#19290 = CARTESIAN_POINT ( 'NONE',  ( -58.00000337463107059, -34.64101615137762025, 17.49999999999999645 ) ) ;
#19291 = CARTESIAN_POINT ( 'NONE',  ( 32.16008401677996886, 61.25926521283067672, -49.22241343995293761 ) ) ;
#19292 = CARTESIAN_POINT ( 'NONE',  ( -52.00000337463110611, -69.28203230275519786, -9.999999999999998224 ) ) ;
#19293 = EDGE_CURVE ( 'NONE', #25751, #12329, #21791, .T. ) ;
#19294 = EDGE_CURVE ( 'NONE', #21710, #16670, #27164, .T. ) ;
#19295 = ORIENTED_EDGE ( 'NONE', *, *, #17177, .F. ) ;
#19296 = ORIENTED_EDGE ( 'NONE', *, *, #6106, .T. ) ;
#19297 = EDGE_CURVE ( 'NONE', #27785, #15953, #11002, .T. ) ;
#19298 = CIRCLE ( 'NONE', #10902, 2.000000000000001776 ) ;
#19299 = EDGE_CURVE ( 'NONE', #8413, #28397, #31938, .T. ) ;
#19300 = CARTESIAN_POINT ( 'NONE',  ( 5.750000000000000000, 89.94802294027094547, 32.49999999999999289 ) ) ;
#19302 = EDGE_CURVE ( 'NONE', #23649, #5222, #27207, .T. ) ;
#19301 = ORIENTED_EDGE ( 'NONE', *, *, #36062, .T. ) ;
#19303 = CARTESIAN_POINT ( 'NONE',  ( -86.45172111230354517, 31.46585318596159553, -4.999999999999997335 ) ) ;
#19304 = DIRECTION ( 'NONE',  ( 1.000000000000000000, 0.000000000000000000, 0.000000000000000000 ) ) ;
#19305 = DIRECTION ( 'NONE',  ( 0.000000000000000000, -0.000000000000000000, -1.000000000000000000 ) ) ;
#19306 = LINE ( 'NONE', #5040, #15860 ) ;
#19307 = DIRECTION ( 'NONE',  ( 1.000000000000000000, 0.000000000000000000, 0.000000000000000000 ) ) ;
#19308 = DIRECTION ( 'NONE',  ( 0.000000000000000000, 0.000000000000000000, 1.000000000000000000 ) ) ;
#19309 = DIRECTION ( 'NONE',  ( 1.000000000000000000, 0.000000000000000000, 0.000000000000000000 ) ) ;
#19310 = DIRECTION ( 'NONE',  ( 0.000000000000000000, 0.000000000000000000, -1.000000000000000000 ) ) ;
#19311 = ORIENTED_EDGE ( 'NONE', *, *, #10307, .T. ) ;
#19312 = VERTEX_POINT ( 'NONE', #8088 ) ;
#19313 = AXIS2_PLACEMENT_3D ( 'NONE', #18626, #10184, #18435 ) ;
#19314 = DIRECTION ( 'NONE',  ( -1.000000000000000000, 0.000000000000000000, 0.000000000000000000 ) ) ;
#19315 = CARTESIAN_POINT ( 'NONE',  ( 89.42901512340354486, -31.83425564451495404, 12.49999999999999822 ) ) ;
#19316 = CARTESIAN_POINT ( 'NONE',  ( -80.00000337463094979, 34.64101615137757051, -9.999999999999998224 ) ) ;
#19317 = CARTESIAN_POINT ( 'NONE',  ( 79.99999662536833966, -3.469446951953614189E-15, 17.49999999999999645 ) ) ;
#19318 = ORIENTED_EDGE ( 'NONE', *, *, #36424, .F. ) ;
#19319 = FACE_OUTER_BOUND ( 'NONE', #23071, .T. ) ;
#19320 = ORIENTED_EDGE ( 'NONE', *, *, #28610, .F. ) ;
#19321 = CIRCLE ( 'NONE', #17510, 25.00000000000000000 ) ;
#19322 = CARTESIAN_POINT ( 'NONE',  ( -3.374631334790434423E-06, 69.28203230275516944, -9.999999999999998224 ) ) ;
#19323 = EDGE_LOOP ( 'NONE', ( #32394, #10896, #20768, #27010 ) ) ;
#19324 = PRESENTATION_STYLE_ASSIGNMENT (( #23896 ) ) ;
#19325 = CARTESIAN_POINT ( 'NONE',  ( -31.00000000000027356, -58.88972745734168512, -49.22241343995298024 ) ) ;
#19326 = CARTESIAN_POINT ( 'NONE',  ( 2.143131898507887033E-16, 84.74289592134881843, -25.98445554337711627 ) ) ;
#19327 = DIRECTION ( 'NONE',  ( -0.5000000000000112133, -0.8660254037844322683, 0.000000000000000000 ) ) ;
#19328 = ORIENTED_EDGE ( 'NONE', *, *, #30434, .T. ) ;
#19329 = ORIENTED_EDGE ( 'NONE', *, *, #734, .T. ) ;
#19330 = EDGE_CURVE ( 'NONE', #14180, #6533, #12963, .T. ) ;
#19331 = AXIS2_PLACEMENT_3D ( 'NONE', #1876, #30001, #4503 ) ;
#19332 = ORIENTED_EDGE ( 'NONE', *, *, #15768, .T. ) ;
#19333 = LINE ( 'NONE', #25512, #32147 ) ;
#19334 = EDGE_CURVE ( 'NONE', #34734, #4235, #30596, .T. ) ;
#19335 = CARTESIAN_POINT ( 'NONE',  ( 79.99999662536832545, -17.32050807568879591, -5.000000000000000000 ) ) ;
#19336 = DIRECTION ( 'NONE',  ( 0.000000000000000000, 0.000000000000000000, -1.000000000000000000 ) ) ;
#19337 = DIRECTION ( 'NONE',  ( 1.000000000000000000, 0.000000000000000000, 0.000000000000000000 ) ) ;
#19338 = CARTESIAN_POINT ( 'NONE',  ( -67.00000337463102085, 25.98076211353317433, -5.000000000000000000 ) ) ;
#19339 = ORIENTED_EDGE ( 'NONE', *, *, #1588, .T. ) ;
#19340 = DIRECTION ( 'NONE',  ( 1.000000000000000000, 0.000000000000000000, 0.000000000000000000 ) ) ;
#19341 = DIRECTION ( 'NONE',  ( 0.000000000000000000, 0.000000000000000000, -1.000000000000000000 ) ) ;
#19342 = AXIS2_PLACEMENT_3D ( 'NONE', #33161, #12910, #4128 ) ;
#19343 = PRESENTATION_STYLE_ASSIGNMENT (( #1730 ) ) ;
#19344 = EDGE_LOOP ( 'NONE', ( #20173, #2903, #24204, #24815 ) ) ;
#19345 = DIRECTION ( 'NONE',  ( -0.000000000000000000, -0.000000000000000000, 1.000000000000000000 ) ) ;
#19346 = CARTESIAN_POINT ( 'NONE',  ( -58.00000337463108480, -51.96152422706641971, -9.999999999999998224 ) ) ;
#19347 = ORIENTED_EDGE ( 'NONE', *, *, #5259, .T. ) ;
#19348 = VERTEX_POINT ( 'NONE', #4740 ) ;
#19349 = CARTESIAN_POINT ( 'NONE',  ( 44.99999662536851019, 77.94228634059959404, -5.000000000000000000 ) ) ;
#19350 = CARTESIAN_POINT ( 'NONE',  ( -93.36492675454779544, -17.14523346298311779, -49.86561046011506448 ) ) ;
#19351 = CARTESIAN_POINT ( 'NONE',  ( 4.296971609540542580, -3.292644976428869885, -4.096693167834889238 ) ) ;
#19352 = CARTESIAN_POINT ( 'NONE',  ( -4.279208249584786294, -3.302900657080020341, -1.325189086772939895 ) ) ;
#19353 = ORIENTED_EDGE ( 'NONE', *, *, #10181, .T. ) ;
#19354 = ORIENTED_EDGE ( 'NONE', *, *, #18665, .T. ) ;
#19355 = AXIS2_PLACEMENT_3D ( 'NONE', #11867, #11501, #2696 ) ;
#19356 = ADVANCED_FACE ( 'NONE', ( #27765 ), #13332, .F. ) ;
#19357 = FACE_BOUND ( 'NONE', #26894, .T. ) ;
#19358 = VECTOR ( 'NONE', #27374, 1000.000000000000000 ) ;
#19359 = EDGE_LOOP ( 'NONE', ( #6708, #35256 ) ) ;
#19360 = LINE ( 'NONE', #11091, #8808 ) ;
#19361 = ORIENTED_EDGE ( 'NONE', *, *, #32563, .T. ) ;
#19362 = VERTEX_POINT ( 'NONE', #15785 ) ;
#19363 = DIRECTION ( 'NONE',  ( -1.000000000000000000, 0.000000000000000000, 0.000000000000000000 ) ) ;
#19364 = VECTOR ( 'NONE', #16939, 1000.000000000000000 ) ;
#19365 = CARTESIAN_POINT ( 'NONE',  ( 49.99999662536846756, 69.28203230275516944, 17.49999999999999645 ) ) ;
#19366 = EDGE_LOOP ( 'NONE', ( #12560, #34820, #33731, #28153 ) ) ;
#19367 = ORIENTED_EDGE ( 'NONE', *, *, #33285, .T. ) ;
#19368 = CARTESIAN_POINT ( 'NONE',  ( 6.000000000000000000, 0.000000000000000000, 32.50000000000000000 ) ) ;
#19369 = CARTESIAN_POINT ( 'NONE',  ( 44.99999662536851019, -60.62177826491080168, -9.999999999999998224 ) ) ;
#19370 = CARTESIAN_POINT ( 'NONE',  ( 3.000000000000000000, 0.000000000000000000, 0.000000000000000000 ) ) ;
#19371 = DIRECTION ( 'NONE',  ( 0.000000000000000000, 0.000000000000000000, 1.000000000000000000 ) ) ;
#19372 = EDGE_LOOP ( 'NONE', ( #25683, #18890, #30513, #4602 ) ) ;
#19373 = CYLINDRICAL_SURFACE ( 'NONE', #1592, 2.000000000000001776 ) ;
#19374 = ADVANCED_FACE ( 'NONE', ( #13164 ), #5087, .F. ) ;
#19375 = FACE_BOUND ( 'NONE', #36076, .T. ) ;
#19376 = DIRECTION ( 'NONE',  ( -1.000000000000000000, 0.000000000000000000, 0.000000000000000000 ) ) ;
#19377 = AXIS2_PLACEMENT_3D ( 'NONE', #7358, #18798, #7917 ) ;
#19378 = DIRECTION ( 'NONE',  ( 0.000000000000000000, 0.000000000000000000, 1.000000000000000000 ) ) ;
#19379 = DIRECTION ( 'NONE',  ( 0.000000000000000000, 0.000000000000000000, 1.000000000000000000 ) ) ;
#19380 = DIRECTION ( 'NONE',  ( 1.000000000000000000, 0.000000000000000000, 0.000000000000000000 ) ) ;
#19381 = AXIS2_PLACEMENT_3D ( 'NONE', #19144, #4886, #31114 ) ;
#19382 = DIRECTION ( 'NONE',  ( 0.000000000000000000, 0.000000000000000000, -1.000000000000000000 ) ) ;
#19383 = CYLINDRICAL_SURFACE ( 'NONE', #31909, 2.000000000000001776 ) ;
#19384 = ORIENTED_EDGE ( 'NONE', *, *, #12536, .F. ) ;
#19385 = CARTESIAN_POINT ( 'NONE',  ( -4.999999999999999112, -2.417244626924490269, -5.688952927922134251 ) ) ;
#19386 = CARTESIAN_POINT ( 'NONE',  ( 26.99999662536856704, 77.94228634059957983, -5.000000000000000000 ) ) ;
#19387 = DIRECTION ( 'NONE',  ( 1.000000000000000000, 0.000000000000000000, 0.000000000000000000 ) ) ;
#19388 = MANIFOLD_SOLID_BREP ( 'M6 Clearance Hole1', #9999 ) ;
#19389 = CIRCLE ( 'NONE', #4428, 2.000000000000001776 ) ;
#19390 = ORIENTED_EDGE ( 'NONE', *, *, #21775, .T. ) ;
#19391 = ORIENTED_EDGE ( 'NONE', *, *, #9193, .T. ) ;
#19392 = EDGE_LOOP ( 'NONE', ( #23404, #35046, #21273, #30936 ) ) ;
#19393 = CIRCLE ( 'NONE', #24178, 2.000000000000001776 ) ;
#19394 = EDGE_CURVE ( 'NONE', #19410, #13732, #2283, .T. ) ;
#19395 = CARTESIAN_POINT ( 'NONE',  ( 0.000000000000000000, 89.94802294027094547, -24.99999999999999645 ) ) ;
#19396 = DIRECTION ( 'NONE',  ( 1.000000000000000000, 0.000000000000000000, 0.000000000000000000 ) ) ;
#19397 = ORIENTED_EDGE ( 'NONE', *, *, #14255, .T. ) ;
#19398 = ADVANCED_FACE ( 'NONE', ( #36601 ), #30207, .F. ) ;
#19399 = CARTESIAN_POINT ( 'NONE',  ( 3.000000000000000000, -1.467624384280027172, 2.542000000000001592 ) ) ;
#19400 = DIRECTION ( 'NONE',  ( 0.000000000000000000, 0.000000000000000000, 1.000000000000000000 ) ) ;
#19401 = VERTEX_POINT ( 'NONE', #28152 ) ;
#19402 = CARTESIAN_POINT ( 'NONE',  ( 23.49187040204899546, -103.5527524078059400, 32.50001250000000397 ) ) ;
#19403 = EDGE_CURVE ( 'NONE', #4724, #15428, #33165, .T. ) ;
#19404 = ORIENTED_EDGE ( 'NONE', *, *, #27768, .T. ) ;
#19405 = CARTESIAN_POINT ( 'NONE',  ( -52.00000337463110611, -69.28203230275519786, 17.49999999999999645 ) ) ;
#19406 = AXIS2_PLACEMENT_3D ( 'NONE', #21317, #15884, #7084 ) ;
#19407 = EDGE_CURVE ( 'NONE', #15883, #21230, #25884, .T. ) ;
#19408 = DIRECTION ( 'NONE',  ( 1.000000000000000000, 0.000000000000000000, 0.000000000000000000 ) ) ;
#19409 = DIRECTION ( 'NONE',  ( 0.000000000000000000, 0.000000000000000000, 1.000000000000000000 ) ) ;
#19410 = VERTEX_POINT ( 'NONE', #23263 ) ;
#19411 = DIRECTION ( 'NONE',  ( 0.000000000000000000, -0.000000000000000000, 1.000000000000000000 ) ) ;
#19412 = ITEM_DEFINED_TRANSFORMATION ( 'NONE', 'NONE', #34526,  #21385 ) ;
#19413 = CIRCLE ( 'NONE', #20000, 2.000000000000001776 ) ;
#19414 = CARTESIAN_POINT ( 'NONE',  ( 62.99999662536841072, 25.98076211353318854, 12.50000000000000000 ) ) ;
#19415 = DIRECTION ( 'NONE',  ( 0.000000000000000000, 0.000000000000000000, 1.000000000000000000 ) ) ;
#19416 = EDGE_LOOP ( 'NONE', ( #5146, #20265, #665, #30726 ) ) ;
#19417 = CIRCLE ( 'NONE', #18223, 2.000000000000001776 ) ;
#19418 = DIRECTION ( 'NONE',  ( 0.000000000000000000, -0.000000000000000000, -1.000000000000000000 ) ) ;
#19419 = DIRECTION ( 'NONE',  ( 0.000000000000000000, 0.000000000000000000, 1.000000000000000000 ) ) ;
#19420 = EDGE_LOOP ( 'NONE', ( #26547, #23242 ) ) ;
#19421 = EDGE_CURVE ( 'NONE', #28397, #8413, #5625, .T. ) ;
#19422 = DIRECTION ( 'NONE',  ( 0.000000000000000000, 0.000000000000000000, 1.000000000000000000 ) ) ;
#19423 = CARTESIAN_POINT ( 'NONE',  ( -60.00000337463104216, 34.64101615137757051, -9.999999999999998224 ) ) ;
#19424 = CARTESIAN_POINT ( 'NONE',  ( 49.99999662536846756, 51.96152422706637708, -5.000000000000000000 ) ) ;
#19425 = DIRECTION ( 'NONE',  ( 0.000000000000000000, 0.000000000000000000, 1.000000000000000000 ) ) ;
#19426 = EDGE_CURVE ( 'NONE', #30126, #1094, #31367, .T. ) ;
#19427 = ORIENTED_EDGE ( 'NONE', *, *, #6750, .T. ) ;
#19428 = ORIENTED_EDGE ( 'NONE', *, *, #2468, .F. ) ;
#19429 = CIRCLE ( 'NONE', #3256, 150.0000000000000284 ) ;
#19430 = FACE_OUTER_BOUND ( 'NONE', #11349, .T. ) ;
#19431 = FACE_OUTER_BOUND ( 'NONE', #33041, .T. ) ;
#19432 = EDGE_CURVE ( 'NONE', #5777, #5185, #8287, .T. ) ;
#19433 = CARTESIAN_POINT ( 'NONE',  ( 0.000000000000000000, 0.000000000000000000, 12.49999999999999822 ) ) ;
#19434 = ORIENTED_EDGE ( 'NONE', *, *, #18401, .T. ) ;
#19435 = EDGE_LOOP ( 'NONE', ( #33789, #5900, #3550, #6982 ) ) ;
#19436 = ADVANCED_FACE ( 'NONE', ( #11610 ), #25720, .F. ) ;
#19437 = DIRECTION ( 'NONE',  ( -1.000000000000000000, 0.000000000000000000, 0.000000000000000000 ) ) ;
#19438 = CARTESIAN_POINT ( 'NONE',  ( -2.018853055115723105, 4.607917337070899677, -0.5666985376598566715 ) ) ;
#19439 = LINE ( 'NONE', #16636, #24856 ) ;
#19440 = ORIENTED_EDGE ( 'NONE', *, *, #24604, .T. ) ;
#19441 = VECTOR ( 'NONE', #27537, 1000.000000000000000 ) ;
#19442 = CIRCLE ( 'NONE', #32592, 2.000000000000001776 ) ;
#19443 = ORIENTED_EDGE ( 'NONE', *, *, #2019, .F. ) ;
#19444 = DIRECTION ( 'NONE',  ( -0.8660254037844379305, 0.5000000000000012212, 0.000000000000000000 ) ) ;
#19445 = AXIS2_PLACEMENT_3D ( 'NONE', #4432, #13238, #30834 ) ;
#19446 = LINE ( 'NONE', #25097, #2728 ) ;
#19447 = ORIENTED_EDGE ( 'NONE', *, *, #29289, .F. ) ;
#19448 = FACE_OUTER_BOUND ( 'NONE', #29865, .T. ) ;
#19449 = VERTEX_POINT ( 'NONE', #19889 ) ;
#19450 = FACE_BOUND ( 'NONE', #29667, .T. ) ;
#19451 = EDGE_CURVE ( 'NONE', #8273, #21059, #22519, .T. ) ;
#19452 = DIRECTION ( 'NONE',  ( 0.000000000000000000, 0.000000000000000000, 1.000000000000000000 ) ) ;
#19453 = AXIS2_PLACEMENT_3D ( 'NONE', #15368, #15565, #35824 ) ;
#19454 = VECTOR ( 'NONE', #31485, 1000.000000000000000 ) ;
#19455 = CARTESIAN_POINT ( 'NONE',  ( 1.598077599632994561, 4.850852159562153432, -3.971474537231019397 ) ) ;
#19456 = EDGE_LOOP ( 'NONE', ( #9063, #31035, #36026, #10326 ) ) ;
#19457 = DIRECTION ( 'NONE',  ( 0.000000000000000000, 0.000000000000000000, 1.000000000000000000 ) ) ;
#19458 = AXIS2_PLACEMENT_3D ( 'NONE', #21575, #30367, #21377 ) ;
#19459 = DIRECTION ( 'NONE',  ( 1.000000000000000000, 0.000000000000000000, 0.000000000000000000 ) ) ;
#19460 = CARTESIAN_POINT ( 'NONE',  ( 61.99999662536845335, 34.64101615137759893, -9.999999999999998224 ) ) ;
#19461 = DIRECTION ( 'NONE',  ( 0.000000000000000000, 0.000000000000000000, 1.000000000000000000 ) ) ;
#19462 = ORIENTED_EDGE ( 'NONE', *, *, #2218, .F. ) ;
#19463 = DIRECTION ( 'NONE',  ( 0.000000000000000000, 0.000000000000000000, -1.000000000000000000 ) ) ;
#19464 = CARTESIAN_POINT ( 'NONE',  ( 54.99999662536844625, 43.30127018922198801, 12.50000000000000000 ) ) ;
#19465 = CIRCLE ( 'NONE', #36834, 3.000000000000000888 ) ;
#19466 = VERTEX_POINT ( 'NONE', #17444 ) ;
#19467 = EDGE_CURVE ( 'NONE', #15920, #25343, #5017, .T. ) ;
#19468 = ORIENTED_EDGE ( 'NONE', *, *, #29505, .F. ) ;
#19469 = FACE_OUTER_BOUND ( 'NONE', #12238, .T. ) ;
#19470 = EDGE_CURVE ( 'NONE', #11022, #4612, #35570, .T. ) ;
#19471 = ORIENTED_EDGE ( 'NONE', *, *, #32604, .F. ) ;
#19472 = CARTESIAN_POINT ( 'NONE',  ( 39.99999662536853151, -69.28203230275519786, -9.999999999999998224 ) ) ;
#19473 = CARTESIAN_POINT ( 'NONE',  ( 4.999996625368645198, 77.94228634059957983, -9.999999999999998224 ) ) ;
#19474 = EDGE_CURVE ( 'NONE', #31658, #12512, #19393, .T. ) ;
#19475 = CARTESIAN_POINT ( 'NONE',  ( 54.99999662536844625, 60.62177826491077326, 17.49999999999999645 ) ) ;
#19476 = CIRCLE ( 'NONE', #23083, 2.000000000000000000 ) ;
#19477 = CARTESIAN_POINT ( 'NONE',  ( -5.204170427930421283E-15, 5.773502691896269745, -0.5999999999999998668 ) ) ;
#19478 = EDGE_CURVE ( 'NONE', #9855, #16950, #12783, .T. ) ;
#19479 = DIRECTION ( 'NONE',  ( 1.000000000000000000, 0.000000000000000000, 0.000000000000000000 ) ) ;
#19480 = CARTESIAN_POINT ( 'NONE',  ( -31.74999999999995737, 0.000000000000000000, 0.000000000000000000 ) ) ;
#19481 = AXIS2_PLACEMENT_3D ( 'NONE', #17526, #11899, #28951 ) ;
#19482 = EDGE_CURVE ( 'NONE', #6351, #30934, #20594, .T. ) ;
#19483 = LINE ( 'NONE', #16481, #20782 ) ;
#19484 = CIRCLE ( 'NONE', #5731, 2.000000000000001776 ) ;
#19485 = CARTESIAN_POINT ( 'NONE',  ( 0.000000000000000000, 0.000000000000000000, -5.000000000000000000 ) ) ;
#19486 = ORIENTED_EDGE ( 'NONE', *, *, #13769, .T. ) ;
#19487 = VECTOR ( 'NONE', #6150, 1000.000000000000000 ) ;
#19488 = ORIENTED_EDGE ( 'NONE', *, *, #6209, .F. ) ;
#19489 = DIRECTION ( 'NONE',  ( 1.000000000000000000, 0.000000000000000000, 0.000000000000000000 ) ) ;
#19490 = CARTESIAN_POINT ( 'NONE',  ( 68.00000000000000000, 0.000000000000000000, -4.999999999999997335 ) ) ;
#19491 = CARTESIAN_POINT ( 'NONE',  ( 2.500000000000008438, 4.330127018922190096, -2.691222917490924395E-15 ) ) ;
#19492 = CARTESIAN_POINT ( 'NONE',  ( -35.83991598322101879, -56.52018970185248037, 12.49999999999999645 ) ) ;
#19493 = VERTEX_POINT ( 'NONE', #11446 ) ;
#19494 = EDGE_CURVE ( 'NONE', #37029, #4744, #8630, .T. ) ;
#19495 = AXIS2_PLACEMENT_3D ( 'NONE', #35401, #15686, #24684 ) ;
#19496 = CIRCLE ( 'NONE', #7529, 33.00000000000001421 ) ;
#19497 = EDGE_CURVE ( 'NONE', #553, #2942, #19417, .T. ) ;
#19498 = CARTESIAN_POINT ( 'NONE',  ( -45.00000337463111322, 60.62177826491077326, -9.999999999999998224 ) ) ;
#19499 = VERTEX_POINT ( 'NONE', #34512 ) ;
#19500 = VERTEX_POINT ( 'NONE', #31315 ) ;
#19501 = FACE_OUTER_BOUND ( 'NONE', #10694, .T. ) ;
#19502 = ORIENTED_EDGE ( 'NONE', *, *, #6002, .F. ) ;
#19503 =( LENGTH_UNIT ( ) NAMED_UNIT ( * ) SI_UNIT ( .MILLI., .METRE. ) );
#19504 = CARTESIAN_POINT ( 'NONE',  ( -22.00000337463124112, -86.60254037844400443, 12.50000000000000000 ) ) ;
#19505 = CYLINDRICAL_SURFACE ( 'NONE', #18835, 3.000000000000000888 ) ;
#19506 = AXIS2_PLACEMENT_3D ( 'NONE', #11848, #34921, #14860 ) ;
#19507 = CARTESIAN_POINT ( 'NONE',  ( -55.00000337463107059, 60.62177826491078747, -5.000000000000000000 ) ) ;
#19508 = ORIENTED_EDGE ( 'NONE', *, *, #29584, .T. ) ;
#19509 = ORIENTED_EDGE ( 'NONE', *, *, #16806, .T. ) ;
#19510 = CIRCLE ( 'NONE', #28487, 2.000000000000001776 ) ;
#19511 = AXIS2_PLACEMENT_3D ( 'NONE', #13735, #2098, #10546 ) ;
#19512 = EDGE_LOOP ( 'NONE', ( #34799, #22888 ) ) ;
#19513 = AXIS2_PLACEMENT_3D ( 'NONE', #3676, #7236, #21282 ) ;
#19514 = STYLED_ITEM ( 'NONE', ( #26960 ), #32508 ) ;
#19515 = ORIENTED_EDGE ( 'NONE', *, *, #32370, .T. ) ;
#19516 = EDGE_CURVE ( 'NONE', #28397, #23804, #8460, .T. ) ;
#19517 = ORIENTED_EDGE ( 'NONE', *, *, #5772, .T. ) ;
#19518 = CARTESIAN_POINT ( 'NONE',  ( 51.99999662536847467, 69.28203230275516944, 12.50000000000000000 ) ) ;
#19519 = CARTESIAN_POINT ( 'NONE',  ( 62.99999662536839651, -43.30127018922199511, -9.999999999999998224 ) ) ;
#19520 = EDGE_CURVE ( 'NONE', #36720, #9972, #17603, .T. ) ;
#19521 = DIRECTION ( 'NONE',  ( -1.000000000000000000, 0.000000000000000000, 0.000000000000000000 ) ) ;
#19522 = DIRECTION ( 'NONE',  ( 0.000000000000000000, 0.000000000000000000, 1.000000000000000000 ) ) ;
#19523 = CARTESIAN_POINT ( 'NONE',  ( 66.99999662536842493, 43.30127018922200222, -9.999999999999998224 ) ) ;
#19524 = ORIENTED_EDGE ( 'NONE', *, *, #9519, .F. ) ;
#19525 = DIRECTION ( 'NONE',  ( 1.000000000000000000, 0.000000000000000000, 0.000000000000000000 ) ) ;
#19526 = AXIS2_PLACEMENT_3D ( 'NONE', #7280, #30329, #13438 ) ;
#19527 = DIRECTION ( 'NONE',  ( 1.000000000000000000, 0.000000000000000000, 0.000000000000000000 ) ) ;
#19528 = CARTESIAN_POINT ( 'NONE',  ( -15.97563234535668109, 90.60231327712331506, -4.999999999999997335 ) ) ;
#19529 = ORIENTED_EDGE ( 'NONE', *, *, #21027, .T. ) ;
#19530 = DIRECTION ( 'NONE',  ( 0.000000000000000000, 0.000000000000000000, 1.000000000000000000 ) ) ;
#19531 = ADVANCED_FACE ( 'NONE', ( #20264 ), #14618, .F. ) ;
#19532 = DIRECTION ( 'NONE',  ( 0.000000000000000000, 0.4999999999999991118, -0.8660254037844391517 ) ) ;
#19533 = ORIENTED_EDGE ( 'NONE', *, *, #13268, .F. ) ;
#19534 = AXIS2_PLACEMENT_3D ( 'NONE', #33453, #1937, #10569 ) ;
#19535 = ORIENTED_EDGE ( 'NONE', *, *, #4827, .F. ) ;
#19536 = DIRECTION ( 'NONE',  ( -1.000000000000000000, 0.000000000000000000, 0.000000000000000000 ) ) ;
#19537 = CARTESIAN_POINT ( 'NONE',  ( -5.170224855064532221, 2.788471980053834010, -4.289066185948678722 ) ) ;
#19538 = CARTESIAN_POINT ( 'NONE',  ( -45.00000337463112743, -60.62177826491080168, -9.999999999999998224 ) ) ;
#19539 = DIRECTION ( 'NONE',  ( 1.000000000000000000, 0.000000000000000000, 0.000000000000000000 ) ) ;
#19540 = ORIENTED_EDGE ( 'NONE', *, *, #3390, .T. ) ;
#19541 = ORIENTED_EDGE ( 'NONE', *, *, #25324, .T. ) ;
#19542 = CIRCLE ( 'NONE', #8162, 95.00000000000000000 ) ;
#19543 = CIRCLE ( 'NONE', #14123, 33.00000000000001421 ) ;
#19544 = EDGE_CURVE ( 'NONE', #16100, #25705, #32596, .T. ) ;
#19545 = CIRCLE ( 'NONE', #9356, 2.000000000000001776 ) ;
#19546 = ADVANCED_FACE ( 'NONE', ( #26816 ), #744, .F. ) ;
#19547 = DIRECTION ( 'NONE',  ( 0.000000000000000000, 0.000000000000000000, -1.000000000000000000 ) ) ;
#19548 = CIRCLE ( 'NONE', #15960, 2.000000000000001776 ) ;
#19549 = EDGE_CURVE ( 'NONE', #36258, #7482, #27188, .T. ) ;
#19550 = EDGE_LOOP ( 'NONE', ( #19524, #7766 ) ) ;
#19551 = EDGE_CURVE ( 'NONE', #15061, #13344, #25996, .T. ) ;
#19552 = CARTESIAN_POINT ( 'NONE',  ( 64.99999662536839651, -43.30127018922199511, -9.999999999999998224 ) ) ;
#19553 = ORIENTED_EDGE ( 'NONE', *, *, #3685, .F. ) ;
#19554 = EDGE_LOOP ( 'NONE', ( #21654, #2820, #8267, #12688 ) ) ;
#19555 = AXIS2_PLACEMENT_3D ( 'NONE', #8355, #19790, #31377 ) ;
#19556 = CARTESIAN_POINT ( 'NONE',  ( 0.000000000000000000, 0.000000000000000000, -10.00000000000000000 ) ) ;
#19557 = CYLINDRICAL_SURFACE ( 'NONE', #35225, 2.000000000000001776 ) ;
#19558 = ORIENTED_EDGE ( 'NONE', *, *, #12053, .T. ) ;
#19559 = ORIENTED_EDGE ( 'NONE', *, *, #14680, .T. ) ;
#19560 = DIRECTION ( 'NONE',  ( -0.8660254037844449249, -0.4999999999999888978, 0.000000000000000000 ) ) ;
#19561 = FACE_OUTER_BOUND ( 'NONE', #18092, .T. ) ;
#19562 = CIRCLE ( 'NONE', #32111, 2.000000000000001776 ) ;
#19563 = DIRECTION ( 'NONE',  ( 0.000000000000000000, 0.000000000000000000, 1.000000000000000000 ) ) ;
#19564 = FACE_OUTER_BOUND ( 'NONE', #6140, .T. ) ;
#19565 = ORIENTED_EDGE ( 'NONE', *, *, #20634, .T. ) ;
#19566 = CYLINDRICAL_SURFACE ( 'NONE', #18977, 2.000000000000001776 ) ;
#19567 = FACE_BOUND ( 'NONE', #36117, .T. ) ;
#19568 = AXIS2_PLACEMENT_3D ( 'NONE', #23557, #32374, #3859 ) ;
#19569 = CARTESIAN_POINT ( 'NONE',  ( 66.99999662536839651, 60.62177826491078747, -9.999999999999998224 ) ) ;
#19570 = CARTESIAN_POINT ( 'NONE',  ( -27.00000337463120914, 77.94228634059957983, -9.999999999999998224 ) ) ;
#19571 = CIRCLE ( 'NONE', #24959, 2.000000000000001776 ) ;
#19572 = DIRECTION ( 'NONE',  ( 0.000000000000000000, 0.000000000000000000, 1.000000000000000000 ) ) ;
#19573 = AXIS2_PLACEMENT_3D ( 'NONE', #13249, #10256, #21511 ) ;
#19574 = EDGE_CURVE ( 'NONE', #36626, #19903, #6184, .T. ) ;
#19575 = CARTESIAN_POINT ( 'NONE',  ( 0.000000000000000000, 0.000000000000000000, -5.000000000000000000 ) ) ;
#19576 = AXIS2_PLACEMENT_3D ( 'NONE', #30210, #33037, #35321 ) ;
#19577 = DIRECTION ( 'NONE',  ( 1.000000000000000000, 0.000000000000000000, 0.000000000000000000 ) ) ;
#19578 = DIRECTION ( 'NONE',  ( 3.469446951953612217E-15, 1.000000000000000000, 0.000000000000000000 ) ) ;
#19579 = ORIENTED_EDGE ( 'NONE', *, *, #3584, .F. ) ;
#19580 = CARTESIAN_POINT ( 'NONE',  ( 81.99999662536832545, -34.64101615137759183, -9.999999999999998224 ) ) ;
#19581 = CARTESIAN_POINT ( 'NONE',  ( 90.60231327712337190, 15.97563234535636134, -4.999999999999997335 ) ) ;
#19582 = CARTESIAN_POINT ( 'NONE',  ( 56.67878100130369035, -27.78182860042797131, 12.49999999999999822 ) ) ;
#19583 = ORIENTED_EDGE ( 'NONE', *, *, #2508, .F. ) ;
#19584 = AXIS2_PLACEMENT_3D ( 'NONE', #32264, #39, #11465 ) ;
#19585 = ORIENTED_EDGE ( 'NONE', *, *, #12463, .F. ) ;
#19586 = VERTEX_POINT ( 'NONE', #29044 ) ;
#19587 = CARTESIAN_POINT ( 'NONE',  ( 19.99999662536858835, 69.28203230275516944, -5.000000000000000000 ) ) ;
#19588 = DIRECTION ( 'NONE',  ( 1.000000000000000000, 0.000000000000000000, 0.000000000000000000 ) ) ;
#19589 = EDGE_LOOP ( 'NONE', ( #27424, #9287 ) ) ;
#19590 = CIRCLE ( 'NONE', #4035, 2.000000000000001776 ) ;
#19591 = CARTESIAN_POINT ( 'NONE',  ( -42.97377950131527058, 96.90768712682508124, -19.99999999999999645 ) ) ;
#19592 = AXIS2_PLACEMENT_3D ( 'NONE', #29700, #32704, #3833 ) ;
#19593 = VERTEX_POINT ( 'NONE', #9929 ) ;
#19594 = CLOSED_SHELL ( 'NONE', ( #31357, #22271, #8066, #33387, #8344, #1929, #4851, #20406, #21678, #33411, #15468, #21016, #19281, #19273, #9107, #25396, #3486, #28868, #30190, #21142, #31346, #18964, #31867, #20742, #32349, #14670, #36381 ) ) ;
#19595 = EDGE_CURVE ( 'NONE', #11195, #2687, #23608, .T. ) ;
#19596 = DIRECTION ( 'NONE',  ( 1.000000000000000000, 0.000000000000000000, 0.000000000000000000 ) ) ;
#19597 = EDGE_LOOP ( 'NONE', ( #15664, #6991, #29034, #33955, #8072, #21411 ) ) ;
#19598 = LINE ( 'NONE', #17147, #34541 ) ;
#19599 = ORIENTED_EDGE ( 'NONE', *, *, #16106, .T. ) ;
#19600 = AXIS2_PLACEMENT_3D ( 'NONE', #3750, #21180, #12355 ) ;
#19601 = AXIS2_PLACEMENT_3D ( 'NONE', #29892, #829, #26902 ) ;
#19602 = DIRECTION ( 'NONE',  ( 1.000000000000000000, 0.000000000000000000, 0.000000000000000000 ) ) ;
#19603 = DIRECTION ( 'NONE',  ( 0.000000000000000000, -0.8660254037844421493, -0.4999999999999942268 ) ) ;
#19604 = ORIENTED_EDGE ( 'NONE', *, *, #3213, .F. ) ;
#19605 = DIRECTION ( 'NONE',  ( -0.000000000000000000, -0.000000000000000000, 1.000000000000000000 ) ) ;
#19606 = VECTOR ( 'NONE', #11938, 1000.000000000000000 ) ;
#19607 = VECTOR ( 'NONE', #24760, 1000.000000000000000 ) ;
#19608 = DIRECTION ( 'NONE',  ( 1.000000000000000000, 0.000000000000000000, 0.000000000000000000 ) ) ;
#19609 = DIRECTION ( 'NONE',  ( 0.000000000000000000, 0.000000000000000000, -1.000000000000000000 ) ) ;
#19610 = VERTEX_POINT ( 'NONE', #31850 ) ;
#19611 = DIRECTION ( 'NONE',  ( 1.000000000000000000, 0.000000000000000000, 0.000000000000000000 ) ) ;
#19612 = DIRECTION ( 'NONE',  ( 1.000000000000000000, 0.000000000000000000, 0.000000000000000000 ) ) ;
#19613 = ORIENTED_EDGE ( 'NONE', *, *, #627, .F. ) ;
#19614 = DIRECTION ( 'NONE',  ( 0.000000000000000000, 0.000000000000000000, 1.000000000000000000 ) ) ;
#19615 = VECTOR ( 'NONE', #31888, 1000.000000000000114 ) ;
#19616 = CARTESIAN_POINT ( 'NONE',  ( 81.99999662536833966, 17.32050807568879236, -9.999999999999998224 ) ) ;
#19617 = CARTESIAN_POINT ( 'NONE',  ( 5.000000000000004441, -2.886751345948140646, -4.069522543421418170 ) ) ;
#19618 = EDGE_CURVE ( 'NONE', #5071, #28766, #14610, .T. ) ;
#19620 = CIRCLE ( 'NONE', #14228, 2.000000000000001776 ) ;
#19619 = CARTESIAN_POINT ( 'NONE',  ( -80.00000337463094979, 17.32050807568878525, -9.999999999999998224 ) ) ;
#19621 = ORIENTED_EDGE ( 'NONE', *, *, #7972, .T. ) ;
#19622 = AXIS2_PLACEMENT_3D ( 'NONE', #9781, #12030, #29295 ) ;
#19623 = ORIENTED_EDGE ( 'NONE', *, *, #24459, .T. ) ;
#19624 = EDGE_CURVE ( 'NONE', #7230, #20815, #4457, .T. ) ;
#19625 = FACE_OUTER_BOUND ( 'NONE', #36364, .T. ) ;
#19626 = CARTESIAN_POINT ( 'NONE',  ( -5.122335214190873565, 2.957381614792576663, -4.281769937709094975 ) ) ;
#19627 = AXIS2_PLACEMENT_3D ( 'NONE', #24276, #7787, #29910 ) ;
#19628 = AXIS2_PLACEMENT_3D ( 'NONE', #19199, #15807, #4762 ) ;
#19630 = VERTEX_POINT ( 'NONE', #21000 ) ;
#19629 = EDGE_CURVE ( 'NONE', #21528, #34463, #32608, .T. ) ;
#19631 = ORIENTED_EDGE ( 'NONE', *, *, #7456, .F. ) ;
#19632 = DIRECTION ( 'NONE',  ( 1.000000000000000000, 0.000000000000000000, 0.000000000000000000 ) ) ;
#19633 = LINE ( 'NONE', #28243, #30391 ) ;
#19634 = DIRECTION ( 'NONE',  ( 1.000000000000000000, 0.000000000000000000, 0.000000000000000000 ) ) ;
#19635 = AXIS2_PLACEMENT_3D ( 'NONE', #20698, #29335, #35165 ) ;
#19636 = ORIENTED_EDGE ( 'NONE', *, *, #16327, .T. ) ;
#19637 = ORIENTED_EDGE ( 'NONE', *, *, #12798, .F. ) ;
#19638 = DIRECTION ( 'NONE',  ( 0.000000000000000000, 0.000000000000000000, 1.000000000000000000 ) ) ;
#19639 = ORIENTED_EDGE ( 'NONE', *, *, #1913, .T. ) ;
#19640 = EDGE_CURVE ( 'NONE', #30820, #7069, #34410, .T. ) ;
#19641 = CYLINDRICAL_SURFACE ( 'NONE', #26311, 95.00000000000001421 ) ;
#19642 = VERTEX_POINT ( 'NONE', #929 ) ;
#19643 = AXIS2_PLACEMENT_3D ( 'NONE', #3881, #10084, #32763 ) ;
#19644 = VECTOR ( 'NONE', #18035, 1000.000000000000000 ) ;
#19645 = FACE_BOUND ( 'NONE', #3239, .T. ) ;
#19646 = AXIS2_PLACEMENT_3D ( 'NONE', #3318, #31633, #28815 ) ;
#19647 = AXIS2_PLACEMENT_3D ( 'NONE', #21002, #26260, #15374 ) ;
#19648 = CYLINDRICAL_SURFACE ( 'NONE', #13122, 6.000000000000005329 ) ;
#19649 = ORIENTED_EDGE ( 'NONE', *, *, #35281, .F. ) ;
#19650 = DIRECTION ( 'NONE',  ( 0.9788780789851974085, 0.2044448739446652619, 0.000000000000000000 ) ) ;
#19651 = LINE ( 'NONE', #31083, #8092 ) ;
#19652 = AXIS2_PLACEMENT_3D ( 'NONE', #8485, #2660, #13743 ) ;
#19653 = DIRECTION ( 'NONE',  ( 1.000000000000000000, 0.000000000000000000, 0.000000000000000000 ) ) ;
#19654 = CARTESIAN_POINT ( 'NONE',  ( -149.8799519615615736, 6.000000000001555200, 32.50000000000000000 ) ) ;
#19655 = EDGE_CURVE ( 'NONE', #17775, #10369, #31960, .T. ) ;
#19656 = ORIENTED_EDGE ( 'NONE', *, *, #30205, .F. ) ;
#19657 = DIRECTION ( 'NONE',  ( 1.000000000000000000, 0.000000000000000000, 0.000000000000000000 ) ) ;
#19658 = DIRECTION ( 'NONE',  ( 0.000000000000000000, 0.000000000000000000, 1.000000000000000000 ) ) ;
#19659 = AXIS2_PLACEMENT_3D ( 'NONE', #9207, #32067, #31716 ) ;
#19660 = CARTESIAN_POINT ( 'NONE',  ( 145.0000000000000853, 5.999999999999493738, 32.50000000000000000 ) ) ;
#19661 = ORIENTED_EDGE ( 'NONE', *, *, #347, .T. ) ;
#19662 = ORIENTED_EDGE ( 'NONE', *, *, #25251, .T. ) ;
#19663 = AXIS2_PLACEMENT_3D ( 'NONE', #16755, #22917, #34004 ) ;
#19664 = EDGE_LOOP ( 'NONE', ( #33848, #18042 ) ) ;
#19665 = ADVANCED_FACE ( 'NONE', ( #18176 ), #15182, .F. ) ;
#19666 = CIRCLE ( 'NONE', #1706, 3.500000000000003109 ) ;
#19667 = CARTESIAN_POINT ( 'NONE',  ( -78.00000337463094979, 34.64101615137757051, -9.999999999999998224 ) ) ;
#19668 = FACE_OUTER_BOUND ( 'NONE', #10204, .T. ) ;
#19669 = AXIS2_PLACEMENT_3D ( 'NONE', #36676, #22809, #8544 ) ;
#19670 = CARTESIAN_POINT ( 'NONE',  ( 3.000000000000000000, 2.935248768560057453, -3.903127820947815962E-15 ) ) ;
#19671 = ADVANCED_FACE ( 'NONE', ( #15569 ), #17812, .F. ) ;
#19672 = VECTOR ( 'NONE', #31496, 1000.000000000000000 ) ;
#19673 = FACE_OUTER_BOUND ( 'NONE', #31340, .T. ) ;
#19674 = CARTESIAN_POINT ( 'NONE',  ( 84.91100539867409225, -72.42200467504753192, 32.49999999999999289 ) ) ;
#19675 = DIRECTION ( 'NONE',  ( 0.000000000000000000, 0.000000000000000000, -1.000000000000000000 ) ) ;
#19676 = CARTESIAN_POINT ( 'NONE',  ( -72.00000337463100664, 34.64101615137758472, -9.999999999999998224 ) ) ;
#19678 = AXIS2_PLACEMENT_3D ( 'NONE', #26827, #3940, #32043 ) ;
#19677 = CARTESIAN_POINT ( 'NONE',  ( -32.00000337463118427, 69.28203230275516944, 12.50000000000000000 ) ) ;
#19679 = ORIENTED_EDGE ( 'NONE', *, *, #5711, .F. ) ;
#19680 = VERTEX_POINT ( 'NONE', #21177 ) ;
#19681 = CIRCLE ( 'NONE', #23261, 2.000000000000001776 ) ;
#19682 = DIRECTION ( 'NONE',  ( 1.000000000000000000, 0.000000000000000000, 0.000000000000000000 ) ) ;
#19683 = DIRECTION ( 'NONE',  ( 0.000000000000000000, 0.000000000000000000, 1.000000000000000000 ) ) ;
#19684 = DIRECTION ( 'NONE',  ( 0.000000000000000000, 0.000000000000000000, 1.000000000000000000 ) ) ;
#19685 = DIRECTION ( 'NONE',  ( 1.000000000000000000, 0.000000000000000000, 0.000000000000000000 ) ) ;
#19686 = VERTEX_POINT ( 'NONE', #32243 ) ;
#19687 = EDGE_CURVE ( 'NONE', #7296, #3432, #20510, .T. ) ;
#19688 = FACE_BOUND ( 'NONE', #10814, .T. ) ;
#19689 = AXIS2_PLACEMENT_3D ( 'NONE', #8264, #19698, #27942 ) ;
#19690 = EDGE_LOOP ( 'NONE', ( #20322, #849, #4960, #31603 ) ) ;
#19691 = ORIENTED_EDGE ( 'NONE', *, *, #31702, .F. ) ;
#19692 = AXIS2_PLACEMENT_3D ( 'NONE', #13194, #10370, #21066 ) ;
#19693 = CYLINDRICAL_SURFACE ( 'NONE', #9255, 2.000000000000000000 ) ;
#19694 = VERTEX_POINT ( 'NONE', #18376 ) ;
#19695 = DIRECTION ( 'NONE',  ( 0.000000000000000000, 0.000000000000000000, 1.000000000000000000 ) ) ;
#19696 = EDGE_CURVE ( 'NONE', #26711, #25432, #36786, .T. ) ;
#19697 = CARTESIAN_POINT ( 'NONE',  ( 0.000000000000000000, 0.000000000000000000, 0.000000000000000000 ) ) ;
#19698 = DIRECTION ( 'NONE',  ( -0.000000000000000000, -0.000000000000000000, 1.000000000000000000 ) ) ;
#19699 = VECTOR ( 'NONE', #13947, 1000.000000000000000 ) ;
#19700 = EDGE_CURVE ( 'NONE', #2614, #114, #3248, .T. ) ;
#19701 = VERTEX_POINT ( 'NONE', #4493 ) ;
#19702 = ORIENTED_EDGE ( 'NONE', *, *, #14686, .T. ) ;
#19703 = AXIS2_PLACEMENT_3D ( 'NONE', #16867, #2440, #8980 ) ;
#19704 = ORIENTED_EDGE ( 'NONE', *, *, #33576, .F. ) ;
#19705 = ORIENTED_EDGE ( 'NONE', *, *, #25066, .T. ) ;
#19706 = CIRCLE ( 'NONE', #33501, 2.000000000000001776 ) ;
#19707 = ORIENTED_EDGE ( 'NONE', *, *, #29573, .T. ) ;
#19708 = CARTESIAN_POINT ( 'NONE',  ( 0.000000000000000000, 1.467624384280024730, -2.542000000000001592 ) ) ;
#19709 = CARTESIAN_POINT ( 'NONE',  ( -108.3061974404900241, -19.22934205794863516, 27.50000000000000000 ) ) ;
#19710 = LINE ( 'NONE', #16341, #36405 ) ;
#19711 = CARTESIAN_POINT ( 'NONE',  ( -48.49679504533954599, -67.96280346788670101, -5.000000000000000000 ) ) ;
#19712 = CARTESIAN_POINT ( 'NONE',  ( 5.253687135845359180, 3.069400712291963096, -4.366239407765167613 ) ) ;
#19713 = ORIENTED_EDGE ( 'NONE', *, *, #7365, .T. ) ;
#19714 = LINE ( 'NONE', #13889, #36209 ) ;
#19715 = DIRECTION ( 'NONE',  ( -0.4999999999999980571, 0.8660254037844399289, 0.000000000000000000 ) ) ;
#19716 = EDGE_CURVE ( 'NONE', #19466, #21436, #27913, .T. ) ;
#19717 = VECTOR ( 'NONE', #35803, 1000.000000000000000 ) ;
#19718 = DIRECTION ( 'NONE',  ( -1.000000000000000000, 0.000000000000000000, 0.000000000000000000 ) ) ;
#19719 = ORIENTED_EDGE ( 'NONE', *, *, #5056, .F. ) ;
#19720 = DIRECTION ( 'NONE',  ( 0.000000000000000000, 0.000000000000000000, 1.000000000000000000 ) ) ;
#19721 = AXIS2_PLACEMENT_3D ( 'NONE', #547, #32222, #29226 ) ;
#19722 = CYLINDRICAL_SURFACE ( 'NONE', #35126, 2.000000000000001776 ) ;
#19723 = EDGE_LOOP ( 'NONE', ( #3316, #13375 ) ) ;
#19724 = ORIENTED_EDGE ( 'NONE', *, *, #22971, .F. ) ;
#19725 = DIRECTION ( 'NONE',  ( 0.000000000000000000, 0.000000000000000000, -1.000000000000000000 ) ) ;
#19726 = CIRCLE ( 'NONE', #8359, 2.000000000000001776 ) ;
#19727 = DIRECTION ( 'NONE',  ( -0.000000000000000000, -0.000000000000000000, 1.000000000000000000 ) ) ;
#19728 = DIRECTION ( 'NONE',  ( -0.000000000000000000, -0.000000000000000000, 1.000000000000000000 ) ) ;
#19729 = CARTESIAN_POINT ( 'NONE',  ( -5.253368672218638125, -3.033033817057809500, -4.359491423763659945 ) ) ;
#19730 = ORIENTED_EDGE ( 'NONE', *, *, #9624, .T. ) ;
#19731 = VERTEX_POINT ( 'NONE', #32812 ) ;
#19732 = AXIS2_PLACEMENT_3D ( 'NONE', #5751, #6497, #18288 ) ;
#19733 = DIRECTION ( 'NONE',  ( 0.000000000000000000, 0.000000000000000000, -1.000000000000000000 ) ) ;
#19734 = CIRCLE ( 'NONE', #5977, 100.0000000000000142 ) ;
#19735 = EDGE_CURVE ( 'NONE', #16685, #33148, #24933, .T. ) ;
#19736 = EDGE_LOOP ( 'NONE', ( #10830, #9700, #14242, #36306, #31977, #17029 ) ) ;
#19737 = AXIS2_PLACEMENT_3D ( 'NONE', #2125, #4947, #22767 ) ;
#19738 = EDGE_CURVE ( 'NONE', #20714, #2553, #10480, .T. ) ;
#19739 = CARTESIAN_POINT ( 'NONE',  ( 61.99999662536843914, -34.64101615137759893, -9.999999999999998224 ) ) ;
#19740 = ORIENTED_EDGE ( 'NONE', *, *, #28412, .F. ) ;
#19741 = DIRECTION ( 'NONE',  ( -0.000000000000000000, -0.000000000000000000, -1.000000000000000000 ) ) ;
#19742 = EDGE_CURVE ( 'NONE', #16632, #19630, #29593, .T. ) ;
#19743 = DIRECTION ( 'NONE',  ( 1.000000000000000000, 0.000000000000000000, 0.000000000000000000 ) ) ;
#19744 = DIRECTION ( 'NONE',  ( 0.000000000000000000, 0.000000000000000000, 1.000000000000000000 ) ) ;
#19745 = AXIS2_PLACEMENT_3D ( 'NONE', #3693, #32377, #4435 ) ;
#19746 = CARTESIAN_POINT ( 'NONE',  ( -47.00000337463111322, 60.62177826491077326, -9.999999999999998224 ) ) ;
#19747 = ORIENTED_EDGE ( 'NONE', *, *, #31094, .T. ) ;
#19748 = ORIENTED_EDGE ( 'NONE', *, *, #21690, .T. ) ;
#19749 = ADVANCED_FACE ( 'NONE', ( #7132 ), #4878, .T. ) ;
#19750 = DIRECTION ( 'NONE',  ( 0.000000000000000000, 0.000000000000000000, 1.000000000000000000 ) ) ;
#19751 = AXIS2_PLACEMENT_3D ( 'NONE', #25281, #14393, #31629 ) ;
#19752 = CARTESIAN_POINT ( 'NONE',  ( -60.00000337463108480, -51.96152422706641971, -5.000000000000000000 ) ) ;
#19753 = EDGE_CURVE ( 'NONE', #32313, #27517, #235, .T. ) ;
#19754 = CARTESIAN_POINT ( 'NONE',  ( -90.00000337463090716, -1.040834085586084257E-14, -9.999999999999998224 ) ) ;
#19755 = FACE_OUTER_BOUND ( 'NONE', #9034, .T. ) ;
#19756 = ORIENTED_EDGE ( 'NONE', *, *, #15171, .T. ) ;
#19757 = DIRECTION ( 'NONE',  ( 0.000000000000000000, -1.000000000000000000, 0.000000000000000000 ) ) ;
#19758 = FACE_BOUND ( 'NONE', #5972, .T. ) ;
#19759 = CARTESIAN_POINT ( 'NONE',  ( -37.50000000000000000, 103.4105893997321886, 27.49999999999999645 ) ) ;
#19760 = DIRECTION ( 'NONE',  ( 0.000000000000000000, 0.000000000000000000, -1.000000000000000000 ) ) ;
#19761 = DIRECTION ( 'NONE',  ( 1.000000000000000000, 0.000000000000000000, 0.000000000000000000 ) ) ;
#19762 = AXIS2_PLACEMENT_3D ( 'NONE', #19052, #27652, #35738 ) ;
#19763 = EDGE_CURVE ( 'NONE', #21017, #35319, #15227, .T. ) ;
#19764 = DIRECTION ( 'NONE',  ( -1.000000000000000000, 0.000000000000000000, -0.000000000000000000 ) ) ;
#19765 = ADVANCED_FACE ( 'NONE', ( #21924 ), #33368, .F. ) ;
#19766 = AXIS2_PLACEMENT_3D ( 'NONE', #9939, #941, #3756 ) ;
#19767 = CARTESIAN_POINT ( 'NONE',  ( -18.28331348626797492, 112.2394285210100833, 27.49998800000000188 ) ) ;
#19768 = EDGE_CURVE ( 'NONE', #31156, #33801, #12206, .T. ) ;
#19769 = EDGE_CURVE ( 'NONE', #5854, #22725, #33191, .T. ) ;
#19770 = CONICAL_SURFACE ( 'NONE', #22768, 4.999999999999997335, 0.9110539511682894664 ) ;
#19771 = CARTESIAN_POINT ( 'NONE',  ( 81.99999662536833966, 34.64101615137759183, 17.49999999999999645 ) ) ;
#19772 = ORIENTED_EDGE ( 'NONE', *, *, #18822, .F. ) ;
#19773 = DIRECTION ( 'NONE',  ( -0.7650473262243671080, -0.6439740589782688707, 0.000000000000000000 ) ) ;
#19774 = CARTESIAN_POINT ( 'NONE',  ( -78.00000337463094979, -17.32050807568882078, -9.999999999999998224 ) ) ;
#19775 = CIRCLE ( 'NONE', #1806, 2.000000000000001776 ) ;
#19776 = CARTESIAN_POINT ( 'NONE',  ( 1.999996625368665182, 69.28203230275516944, -5.000000000000000000 ) ) ;
#19777 = ORIENTED_EDGE ( 'NONE', *, *, #34282, .F. ) ;
#19778 = ORIENTED_EDGE ( 'NONE', *, *, #26802, .T. ) ;
#19779 = ORIENTED_EDGE ( 'NONE', *, *, #13464, .F. ) ;
#19780 = AXIS2_PLACEMENT_3D ( 'NONE', #17169, #22606, #28595 ) ;
#19781 = FACE_OUTER_BOUND ( 'NONE', #9737, .T. ) ;
#19782 = DIRECTION ( 'NONE',  ( 1.000000000000000000, 0.000000000000000000, 0.000000000000000000 ) ) ;
#19783 = AXIS2_PLACEMENT_3D ( 'NONE', #3519, #14952, #12097 ) ;
#19784 = ORIENTED_EDGE ( 'NONE', *, *, #22906, .F. ) ;
#19785 = DIRECTION ( 'NONE',  ( 1.000000000000000000, 0.000000000000000000, 0.000000000000000000 ) ) ;
#19786 = VERTEX_POINT ( 'NONE', #33567 ) ;
#19787 = AXIS2_PLACEMENT_3D ( 'NONE', #31107, #16681, #5243 ) ;
#19788 = CARTESIAN_POINT ( 'NONE',  ( 12.20884028603261484, -116.8570725989752503, 32.50000000000000000 ) ) ;
#19789 = VERTEX_POINT ( 'NONE', #25129 ) ;
#19790 = DIRECTION ( 'NONE',  ( -0.000000000000000000, -0.000000000000000000, 1.000000000000000000 ) ) ;
#19791 = VECTOR ( 'NONE', #10699, 1000.000000000000000 ) ;
#19792 = ORIENTED_EDGE ( 'NONE', *, *, #26387, .T. ) ;
#19793 = CARTESIAN_POINT ( 'NONE',  ( 4.999996625368645198, 77.94228634059957983, -9.999999999999998224 ) ) ;
#19794 = CARTESIAN_POINT ( 'NONE',  ( 4.829002333675111558, -2.985476894631607259, -1.879366290983715881 ) ) ;
#19795 = CIRCLE ( 'NONE', #29, 2.000000000000001776 ) ;
#19796 = VERTEX_POINT ( 'NONE', #4695 ) ;
#19797 = DIRECTION ( 'NONE',  ( 0.000000000000000000, 0.000000000000000000, 1.000000000000000000 ) ) ;
#19798 = STYLED_ITEM ( 'NONE', ( #34156 ), #6859 ) ;
#19799 = CARTESIAN_POINT ( 'NONE',  ( 93.55673653616000252, 16.49657687835711073, -5.000000000000000000 ) ) ;
#19800 = CARTESIAN_POINT ( 'NONE',  ( -3.374631289687624047E-06, -69.28203230275519786, -5.000000000000000000 ) ) ;
#19801 = ORIENTED_EDGE ( 'NONE', *, *, #23769, .F. ) ;
#19802 = DIRECTION ( 'NONE',  ( 0.000000000000000000, 0.000000000000000000, 1.000000000000000000 ) ) ;
#19803 = CARTESIAN_POINT ( 'NONE',  ( 61.99999662536843914, -34.64101615137759893, 12.50000000000000000 ) ) ;
#19804 = ORIENTED_EDGE ( 'NONE', *, *, #12961, .F. ) ;
#19805 = CARTESIAN_POINT ( 'NONE',  ( -75.00000337463097821, -8.660254037844422825, 17.49999999999999645 ) ) ;
#19806 = DIRECTION ( 'NONE',  ( -0.000000000000000000, -0.000000000000000000, 1.000000000000000000 ) ) ;
#19807 = CYLINDRICAL_SURFACE ( 'NONE', #32759, 2.000000000000001776 ) ;
#19808 = CYLINDRICAL_SURFACE ( 'NONE', #26617, 2.000000000000001776 ) ;
#19809 = ORIENTED_EDGE ( 'NONE', *, *, #10328, .T. ) ;
#19810 = EDGE_CURVE ( 'NONE', #18552, #875, #857, .T. ) ;
#19811 = VERTEX_POINT ( 'NONE', #13469 ) ;
#19812 = DIRECTION ( 'NONE',  ( -0.000000000000000000, -0.000000000000000000, 1.000000000000000000 ) ) ;
#19813 = CARTESIAN_POINT ( 'NONE',  ( 19.13981058454793072, -60.93295298010985306, 12.49999999999999822 ) ) ;
#19814 = ORIENTED_EDGE ( 'NONE', *, *, #34041, .T. ) ;
#19815 = ORIENTED_EDGE ( 'NONE', *, *, #10808, .F. ) ;
#19816 = B_SPLINE_CURVE_WITH_KNOTS ( 'NONE', 3,
 ( #17985, #32792, #9153, #20584, #20785, #1107, #12327, #29409 ),
 .UNSPECIFIED., .F., .F.,
 ( 4, 2, 2, 4 ),
 ( 0.002921158011986721599, 0.003648658599403073119, 0.004376159186819424639, 0.005831160361652126811 ),
 .UNSPECIFIED. ) ;
#19817 = CIRCLE ( 'NONE', #21608, 30.00000000000000000 ) ;
#19818 = DIRECTION ( 'NONE',  ( -1.000000000000000000, -0.000000000000000000, -0.000000000000000000 ) ) ;
#19819 = CARTESIAN_POINT ( 'NONE',  ( -87.83969979969870678, -14.80603122773086966, -4.999999999999997335 ) ) ;
#19820 = CARTESIAN_POINT ( 'NONE',  ( 27.78182860042856461, 56.67878100130339902, -4.999999999999997335 ) ) ;
#19821 = EDGE_LOOP ( 'NONE', ( #10212, #31122 ) ) ;
#19822 = EDGE_LOOP ( 'NONE', ( #30466, #25412, #4405, #2265 ) ) ;
#19823 = DIRECTION ( 'NONE',  ( 1.000000000000000000, 0.000000000000000000, 0.000000000000000000 ) ) ;
#19824 = CARTESIAN_POINT ( 'NONE',  ( -35.19434990244938888, 52.39915983220783602, -4.999999999999997335 ) ) ;
#19825 = EDGE_LOOP ( 'NONE', ( #4918, #25551, #4629, #14494, #6518, #18438, #33583, #32692, #6915, #8582, #18177, #22742, #24883 ) ) ;
#19826 = CARTESIAN_POINT ( 'NONE',  ( 79.99999662536832545, -34.64101615137759183, 12.50000000000000000 ) ) ;
#19827 = ORIENTED_EDGE ( 'NONE', *, *, #22911, .F. ) ;
#19828 = FACE_BOUND ( 'NONE', #32317, .T. ) ;
#19829 = EDGE_CURVE ( 'NONE', #35994, #28731, #24577, .T. ) ;
#19830 = EDGE_CURVE ( 'NONE', #22507, #23780, #31390, .T. ) ;
#19831 = CARTESIAN_POINT ( 'NONE',  ( 19.99999662536857770, 86.60254037844397601, -9.999999999999998224 ) ) ;
#19832 = ORIENTED_EDGE ( 'NONE', *, *, #11710, .F. ) ;
#19833 = CARTESIAN_POINT ( 'NONE',  ( 0.000000000000000000, 0.000000000000000000, 0.000000000000000000 ) ) ;
#19834 = DIRECTION ( 'NONE',  ( 0.000000000000000000, 0.000000000000000000, 1.000000000000000000 ) ) ;
#19835 = EDGE_CURVE ( 'NONE', #17590, #22725, #21370, .T. ) ;
#19836 = CARTESIAN_POINT ( 'NONE',  ( 44.99999662536851019, -60.62177826491080168, -9.999999999999998224 ) ) ;
#19837 = FACE_OUTER_BOUND ( 'NONE', #34170, .T. ) ;
#19838 = ORIENTED_EDGE ( 'NONE', *, *, #28077, .T. ) ;
#19839 = CARTESIAN_POINT ( 'NONE',  ( -85.00000337463092137, -8.660254037844422825, 12.50000000000000000 ) ) ;
#19840 = FACE_OUTER_BOUND ( 'NONE', #3850, .T. ) ;
#19841 = FACE_OUTER_BOUND ( 'NONE', #8114, .T. ) ;
#19842 = ORIENTED_EDGE ( 'NONE', *, *, #33538, .F. ) ;
#19843 = ORIENTED_EDGE ( 'NONE', *, *, #34206, .F. ) ;
#19844 = EDGE_CURVE ( 'NONE', #27194, #24231, #24832, .T. ) ;
#19845 = EDGE_LOOP ( 'NONE', ( #7002, #12511, #15736, #22030 ) ) ;
#19846 = DIRECTION ( 'NONE',  ( -1.000000000000000000, 0.000000000000000000, 0.000000000000000000 ) ) ;
#19847 = CARTESIAN_POINT ( 'NONE',  ( -18.00000337463123046, 86.60254037844397601, -9.999999999999998224 ) ) ;
#19848 = CARTESIAN_POINT ( 'NONE',  ( -31.46585318596190106, -86.45172111230344569, 12.49999999999999822 ) ) ;
#19849 = DIRECTION ( 'NONE',  ( 0.000000000000000000, 0.000000000000000000, 1.000000000000000000 ) ) ;
#19850 = CYLINDRICAL_SURFACE ( 'NONE', #25674, 2.000000000000001776 ) ;
#19851 = CARTESIAN_POINT ( 'NONE',  ( -104.1070924947364205, -59.68425981333875541, 32.50000000000000000 ) ) ;
#19852 = AXIS2_PLACEMENT_3D ( 'NONE', #4146, #17824, #29258 ) ;
#19853 = DIRECTION ( 'NONE',  ( 0.000000000000000000, 0.000000000000000000, 1.000000000000000000 ) ) ;
#19854 = DIRECTION ( 'NONE',  ( 1.000000000000000000, 0.000000000000000000, 0.000000000000000000 ) ) ;
#19855 = ORIENTED_EDGE ( 'NONE', *, *, #20570, .T. ) ;
#19856 = VERTEX_POINT ( 'NONE', #21734 ) ;
#19857 = CYLINDRICAL_SURFACE ( 'NONE', #13477, 2.000000000000001776 ) ;
#19858 = EDGE_CURVE ( 'NONE', #1373, #210, #23019, .T. ) ;
#19859 = DIRECTION ( 'NONE',  ( 1.000000000000000000, 0.000000000000000000, 0.000000000000000000 ) ) ;
#19860 = CARTESIAN_POINT ( 'NONE',  ( 0.000000000000000000, -55.00000000000000000, -10.00000000000000178 ) ) ;
#19861 = FACE_OUTER_BOUND ( 'NONE', #15580, .T. ) ;
#19862 = ORIENTED_EDGE ( 'NONE', *, *, #36253, .F. ) ;
#19863 = EDGE_CURVE ( 'NONE', #33445, #2400, #19306, .T. ) ;
#19864 = DIRECTION ( 'NONE',  ( 1.000000000000000000, 0.000000000000000000, 0.000000000000000000 ) ) ;
#19865 = ORIENTED_EDGE ( 'NONE', *, *, #15585, .T. ) ;
#19866 = ORIENTED_EDGE ( 'NONE', *, *, #36770, .F. ) ;
#19867 = EDGE_CURVE ( 'NONE', #26674, #2722, #24315, .T. ) ;
#19868 = LINE ( 'NONE', #14244, #18221 ) ;
#19869 = ORIENTED_EDGE ( 'NONE', *, *, #29017, .T. ) ;
#19870 = CARTESIAN_POINT ( 'NONE',  ( 34.99999662536855283, 60.62177826491078747, 17.49999999999999645 ) ) ;
#19871 = CARTESIAN_POINT ( 'NONE',  ( 110.2237710830529664, -101.7384897088154929, 27.50000000000000000 ) ) ;
#19872 = ADVANCED_FACE ( 'NONE', ( #11567 ), #25847, .F. ) ;
#19873 = AXIS2_PLACEMENT_3D ( 'NONE', #16205, #10759, #22195 ) ;
#19874 = DIRECTION ( 'NONE',  ( 0.000000000000000000, -1.000000000000000000, 0.000000000000000000 ) ) ;
#19875 = ORIENTED_EDGE ( 'NONE', *, *, #27556, .T. ) ;
#19876 = ORIENTED_EDGE ( 'NONE', *, *, #18122, .F. ) ;
#19877 = VERTEX_POINT ( 'NONE', #33738 ) ;
#19878 = ORIENTED_EDGE ( 'NONE', *, *, #15320, .F. ) ;
#19879 = VERTEX_POINT ( 'NONE', #36730 ) ;
#19880 = CARTESIAN_POINT ( 'NONE',  ( -5.750000000000000000, 89.94802294027094547, -24.99999999999999645 ) ) ;
#19881 = FACE_OUTER_BOUND ( 'NONE', #18, .T. ) ;
#19882 = CARTESIAN_POINT ( 'NONE',  ( -56.67878100130369035, 27.78182860042797131, -4.999999999999997335 ) ) ;
#19883 = CARTESIAN_POINT ( 'NONE',  ( 89.99999662536828282, 0.000000000000000000, -9.999999999999998224 ) ) ;
#19884 = CYLINDRICAL_SURFACE ( 'NONE', #29093, 3.500000000000003109 ) ;
#19885 = EDGE_LOOP ( 'NONE', ( #8952, #7398, #27699, #36620 ) ) ;
#19886 = CARTESIAN_POINT ( 'NONE',  ( 49.99999662536846756, -69.28203230275519786, -9.999999999999998224 ) ) ;
#19887 = EDGE_CURVE ( 'NONE', #8683, #27052, #28651, .T. ) ;
#19888 = DIRECTION ( 'NONE',  ( 0.000000000000000000, 0.000000000000000000, -1.000000000000000000 ) ) ;
#19889 = CARTESIAN_POINT ( 'NONE',  ( 72.99999662536836809, 8.660254037844394404, -5.000000000000000000 ) ) ;
#19890 = EDGE_LOOP ( 'NONE', ( #6899, #13633 ) ) ;
#19891 = DIRECTION ( 'NONE',  ( -0.000000000000000000, -0.000000000000000000, 1.000000000000000000 ) ) ;
#19892 = CARTESIAN_POINT ( 'NONE',  ( -37.50000000000000000, -103.4105893997321743, 32.50000000000000000 ) ) ;
#19893 = VERTEX_POINT ( 'NONE', #2792 ) ;
#19894 = EDGE_CURVE ( 'NONE', #6948, #31042, #8421, .T. ) ;
#19895 = ORIENTED_EDGE ( 'NONE', *, *, #28079, .T. ) ;
#19896 = CARTESIAN_POINT ( 'NONE',  ( 94.55012560584681580, 9.234378588654079678, 32.50000000000000000 ) ) ;
#19897 = VECTOR ( 'NONE', #29285, 1000.000000000000000 ) ;
#19898 = EDGE_CURVE ( 'NONE', #28759, #26995, #2429, .T. ) ;
#19899 = LINE ( 'NONE', #28513, #31848 ) ;
#19900 = CARTESIAN_POINT ( 'NONE',  ( 0.000000000000000000, 0.000000000000000000, -5.000000000000000000 ) ) ;
#19901 = DIRECTION ( 'NONE',  ( 1.000000000000000000, 0.000000000000000000, 0.000000000000000000 ) ) ;
#19902 = EDGE_LOOP ( 'NONE', ( #10531, #21057, #16048, #35543 ) ) ;
#19903 = VERTEX_POINT ( 'NONE', #8037 ) ;
#19904 = CARTESIAN_POINT ( 'NONE',  ( 82.99999662536831124, -8.660254037844397956, -9.999999999999998224 ) ) ;
#19905 = CARTESIAN_POINT ( 'NONE',  ( 81.99999662536832545, -34.64101615137759183, -5.000000000000000000 ) ) ;
#19906 = ORIENTED_EDGE ( 'NONE', *, *, #16716, .T. ) ;
#19907 = CARTESIAN_POINT ( 'NONE',  ( 3.750000000000001776, 0.000000000000000000, 13.31572692736085095 ) ) ;
#19908 = ORIENTED_EDGE ( 'NONE', *, *, #3281, .F. ) ;
#19909 = CARTESIAN_POINT ( 'NONE',  ( -80.00000337463094979, 17.32050807568878525, 12.50000000000000000 ) ) ;
#19910 = CIRCLE ( 'NONE', #2551, 3.500000000000003109 ) ;
#19911 = DIRECTION ( 'NONE',  ( 0.8660254037844378194, -0.5000000000000014433, 0.000000000000000000 ) ) ;
#19912 = CARTESIAN_POINT ( 'NONE',  ( -108.3061974404900241, -19.22934205794863516, 32.50000000000000000 ) ) ;
#19913 = ADVANCED_FACE ( 'NONE', ( #19673 ), #33920, .F. ) ;
#19914 = CARTESIAN_POINT ( 'NONE',  ( 74.99999662536836809, 43.30127018922198801, -9.999999999999998224 ) ) ;
#19915 = EDGE_LOOP ( 'NONE', ( #2279, #26691, #36872, #1352 ) ) ;
#19916 = ORIENTED_EDGE ( 'NONE', *, *, #23921, .T. ) ;
#19917 = DIRECTION ( 'NONE',  ( 1.000000000000000000, -0.000000000000000000, 0.000000000000000000 ) ) ;
#19918 = LINE ( 'NONE', #22920, #4615 ) ;
#19919 = CARTESIAN_POINT ( 'NONE',  ( -80.00000337463096400, -34.64101615137762025, 17.49999999999999645 ) ) ;
#19920 = DIRECTION ( 'NONE',  ( 1.000000000000000000, 0.000000000000000000, 0.000000000000000000 ) ) ;
#19921 = ORIENTED_EDGE ( 'NONE', *, *, #29791, .F. ) ;
#19922 = CARTESIAN_POINT ( 'NONE',  ( 31.27962116909601420, -62.97617850287780072, 12.49999999999999822 ) ) ;
#19923 = AXIS2_PLACEMENT_3D ( 'NONE', #8280, #17438, #36765 ) ;
#19924 = FACE_BOUND ( 'NONE', #10925, .T. ) ;
#19925 = AXIS2_PLACEMENT_3D ( 'NONE', #2894, #22570, #34217 ) ;
#19926 = LINE ( 'NONE', #26103, #10061 ) ;
#19927 = CARTESIAN_POINT ( 'NONE',  ( -3.499999999999991562, 55.00000000000000000, -10.00000000000000000 ) ) ;
#19928 = DIRECTION ( 'NONE',  ( -0.000000000000000000, -0.000000000000000000, 1.000000000000000000 ) ) ;
#19929 = CARTESIAN_POINT ( 'NONE',  ( -65.00000337463102085, 25.98076211353317433, -9.999999999999998224 ) ) ;
#19930 = EDGE_CURVE ( 'NONE', #10704, #24005, #7402, .T. ) ;
#19931 = DIRECTION ( 'NONE',  ( 0.000000000000000000, 0.000000000000000000, 1.000000000000000000 ) ) ;
#19932 = CARTESIAN_POINT ( 'NONE',  ( -60.00000337463108480, -51.96152422706641971, -9.999999999999998224 ) ) ;
#19933 = ORIENTED_EDGE ( 'NONE', *, *, #28206, .F. ) ;
#19934 = EDGE_CURVE ( 'NONE', #8805, #29715, #10428, .T. ) ;
#19935 = LINE ( 'NONE', #2514, #4066 ) ;
#19936 = CARTESIAN_POINT ( 'NONE',  ( 35.19434990244975126, -52.39915983220758022, 12.49999999999999822 ) ) ;
#19937 = FACE_OUTER_BOUND ( 'NONE', #963, .T. ) ;
#19938 = VERTEX_POINT ( 'NONE', #30906 ) ;
#19939 = EDGE_CURVE ( 'NONE', #4318, #10468, #9852, .T. ) ;
#19940 = AXIS2_PLACEMENT_3D ( 'NONE', #9018, #577, #23074 ) ;
#19941 = VERTEX_POINT ( 'NONE', #11221 ) ;
#19942 = EDGE_LOOP ( 'NONE', ( #28136, #23052, #3647, #11447, #667 ) ) ;
#19943 = DIRECTION ( 'NONE',  ( 1.000000000000000000, 0.000000000000000000, 0.000000000000000000 ) ) ;
#19944 = DIRECTION ( 'NONE',  ( 1.000000000000000000, 0.000000000000000000, 0.000000000000000000 ) ) ;
#19945 = EDGE_CURVE ( 'NONE', #13995, #1820, #25295, .T. ) ;
#19946 = CARTESIAN_POINT ( 'NONE',  ( -3.000003374631269981, -77.94228634059960825, -9.999999999999998224 ) ) ;
#19947 = ORIENTED_EDGE ( 'NONE', *, *, #28390, .T. ) ;
#19948 = EDGE_CURVE ( 'NONE', #22555, #21363, #5069, .T. ) ;
#19949 = DIRECTION ( 'NONE',  ( 1.000000000000000000, 0.000000000000000000, 0.000000000000000000 ) ) ;
#19950 = VECTOR ( 'NONE', #10579, 1000.000000000000000 ) ;
#19951 = ORIENTED_EDGE ( 'NONE', *, *, #13061, .F. ) ;
#19952 = CARTESIAN_POINT ( 'NONE',  ( -3.108944973436880588, -78.59336093177338967, -5.000000000000000000 ) ) ;
#19953 = ORIENTED_EDGE ( 'NONE', *, *, #30397, .F. ) ;
#19954 = DIRECTION ( 'NONE',  ( 0.000000000000000000, 0.000000000000000000, 1.000000000000000000 ) ) ;
#19955 = EDGE_LOOP ( 'NONE', ( #30633, #17848 ) ) ;
#19956 = EDGE_CURVE ( 'NONE', #23050, #29314, #14024, .T. ) ;
#19957 = VERTEX_POINT ( 'NONE', #31270 ) ;
#19958 = EDGE_CURVE ( 'NONE', #14414, #34086, #4404, .T. ) ;
#19959 = FACE_OUTER_BOUND ( 'NONE', #36681, .T. ) ;
#19960 = DIRECTION ( 'NONE',  ( 0.000000000000000000, 0.000000000000000000, -1.000000000000000000 ) ) ;
#19961 = ADVANCED_FACE ( 'NONE', ( #1809 ), #36115, .T. ) ;
#19962 = EDGE_CURVE ( 'NONE', #34330, #28343, #20542, .T. ) ;
#19963 = EDGE_LOOP ( 'NONE', ( #36099, #10516, #9557, #30918 ) ) ;
#19964 = CARTESIAN_POINT ( 'NONE',  ( -85.00000337463092137, 8.660254037844389075, -9.999999999999998224 ) ) ;
#19965 = CONICAL_SURFACE ( 'NONE', #13367, 4.999999999999997335, 0.9110539511682894664 ) ;
#19966 = CONTEXT_DEPENDENT_SHAPE_REPRESENTATION ( #1526, #30763 ) ;
#19967 = DIRECTION ( 'NONE',  ( 1.000000000000000000, 0.000000000000000000, 0.000000000000000000 ) ) ;
#19968 = DIRECTION ( 'NONE',  ( 1.000000000000000000, 0.000000000000000000, 0.000000000000000000 ) ) ;
#19969 = VECTOR ( 'NONE', #23585, 1000.000000000000000 ) ;
#19970 = ORIENTED_EDGE ( 'NONE', *, *, #30968, .F. ) ;
#19971 = FACE_OUTER_BOUND ( 'NONE', #24098, .T. ) ;
#19972 = CYLINDRICAL_SURFACE ( 'NONE', #31712, 30.00000000000000000 ) ;
#19973 = ORIENTED_EDGE ( 'NONE', *, *, #3508, .T. ) ;
#19974 = CARTESIAN_POINT ( 'NONE',  ( -8.000003374631249997, -86.60254037844400443, 12.50000000000000000 ) ) ;
#19975 = DIRECTION ( 'NONE',  ( 0.000000000000000000, 0.4999999999999951150, -0.8660254037844414832 ) ) ;
#19976 = CYLINDRICAL_SURFACE ( 'NONE', #26150, 45.00000000000000000 ) ;
#19977 = CARTESIAN_POINT ( 'NONE',  ( -70.00000337463102085, -51.96152422706641971, -9.999999999999998224 ) ) ;
#19978 = AXIS2_PLACEMENT_3D ( 'NONE', #3056, #27659, #31175 ) ;
#19980 = ORIENTED_EDGE ( 'NONE', *, *, #826, .F. ) ;
#19979 = EDGE_CURVE ( 'NONE', #17608, #24795, #7978, .T. ) ;
#19981 = AXIS2_PLACEMENT_3D ( 'NONE', #21039, #26662, #23486 ) ;
#19982 = VERTEX_POINT ( 'NONE', #18687 ) ;
#19983 = CARTESIAN_POINT ( 'NONE',  ( -30.00000337463118427, 69.28203230275516944, 12.50000000000000000 ) ) ;
#19984 = DIRECTION ( 'NONE',  ( 1.000000000000000000, 0.000000000000000000, 0.000000000000000000 ) ) ;
#19985 = AXIS2_PLACEMENT_3D ( 'NONE', #13979, #35962, #4831 ) ;
#19986 = ORIENTED_EDGE ( 'NONE', *, *, #1353, .T. ) ;
#19987 = ORIENTED_EDGE ( 'NONE', *, *, #21330, .F. ) ;
#19988 = LINE ( 'NONE', #25088, #15197 ) ;
#19989 = DIRECTION ( 'NONE',  ( 0.000000000000000000, 0.000000000000000000, 1.000000000000000000 ) ) ;
#19990 = ADVANCED_FACE ( 'NONE', ( #13052 ), #21855, .F. ) ;
#19991 = CARTESIAN_POINT ( 'NONE',  ( 42.99999662536850309, 77.94228634059959404, -9.999999999999998224 ) ) ;
#19992 = EDGE_LOOP ( 'NONE', ( #35361, #25223, #36577, #8395 ) ) ;
#19993 = ORIENTED_EDGE ( 'NONE', *, *, #28855, .F. ) ;
#19994 = CIRCLE ( 'NONE', #33156, 33.00000000000001421 ) ;
#19995 = DIRECTION ( 'NONE',  ( 0.000000000000000000, 0.000000000000000000, 1.000000000000000000 ) ) ;
#19996 = EDGE_LOOP ( 'NONE', ( #19621, #5456 ) ) ;
#19997 = PLANE ( 'NONE',  #32899 ) ;
#19998 = ORIENTED_EDGE ( 'NONE', *, *, #8744, .T. ) ;
#19999 = FACE_BOUND ( 'NONE', #3419, .T. ) ;
#20000 = AXIS2_PLACEMENT_3D ( 'NONE', #14428, #30746, #34143 ) ;
#20001 = ADVANCED_FACE ( 'NONE', ( #24506 ), #7426, .F. ) ;
#20002 = PLANE ( 'NONE',  #12514 ) ;
#20003 = EDGE_CURVE ( 'NONE', #22186, #1820, #19065, .T. ) ;
#20004 = EDGE_CURVE ( 'NONE', #13186, #12570, #25358, .T. ) ;
#20005 = DIRECTION ( 'NONE',  ( 0.000000000000000000, 0.000000000000000000, 1.000000000000000000 ) ) ;
#20006 = EDGE_LOOP ( 'NONE', ( #31597, #11969, #3549, #14758, #21663, #18877, #31685, #33049, #19639, #22416, #6969, #30997, #12985, #7329, #18989, #23742 ) ) ;
#20007 = DIRECTION ( 'NONE',  ( 0.000000000000000000, 0.000000000000000000, 1.000000000000000000 ) ) ;
#20008 = DIRECTION ( 'NONE',  ( 0.000000000000000000, 0.4999999999999953926, -0.8660254037844412611 ) ) ;
#20009 = DIRECTION ( 'NONE',  ( 0.000000000000000000, 0.000000000000000000, 1.000000000000000000 ) ) ;
#20010 = LINE ( 'NONE', #11744, #1165 ) ;
#20011 = EDGE_LOOP ( 'NONE', ( #4970, #7593, #20641, #23811 ) ) ;
#20012 = DIRECTION ( 'NONE',  ( -0.000000000000000000, 0.000000000000000000, -1.000000000000000000 ) ) ;
#20013 = CARTESIAN_POINT ( 'NONE',  ( -3.374631303565411855E-06, -86.60254037844400443, -9.999999999999998224 ) ) ;
#20014 = DIRECTION ( 'NONE',  ( -1.000000000000000000, 0.000000000000000000, 0.000000000000000000 ) ) ;
#20015 = EDGE_LOOP ( 'NONE', ( #11994, #26205, #4717, #9155 ) ) ;
#20016 = AXIS2_PLACEMENT_3D ( 'NONE', #20924, #12256, #28963 ) ;
#20017 = VERTEX_POINT ( 'NONE', #33673 ) ;
#20018 = ORIENTED_EDGE ( 'NONE', *, *, #33017, .F. ) ;
#20019 = ADVANCED_FACE ( 'NONE', ( #33105 ), #4625, .F. ) ;
#20020 = CARTESIAN_POINT ( 'NONE',  ( -75.00000337463100664, -43.30127018922202353, -9.999999999999998224 ) ) ;
#20021 = VECTOR ( 'NONE', #1482, 1000.000000000000000 ) ;
#20022 = DIRECTION ( 'NONE',  ( -1.000000000000000000, -0.000000000000000000, -0.000000000000000000 ) ) ;
#20023 = DIRECTION ( 'NONE',  ( 1.000000000000000000, 0.000000000000000000, 0.000000000000000000 ) ) ;
#20024 = PLANE ( 'NONE',  #23088 ) ;
#20025 = DIRECTION ( 'NONE',  ( -0.000000000000000000, -0.000000000000000000, 1.000000000000000000 ) ) ;
#20026 = CARTESIAN_POINT ( 'NONE',  ( 7.999996625368625658, 86.60254037844397601, -5.000000000000000000 ) ) ;
#20027 = VERTEX_POINT ( 'NONE', #16066 ) ;
#20028 = ORIENTED_EDGE ( 'NONE', *, *, #25645, .T. ) ;
#20029 = CYLINDRICAL_SURFACE ( 'NONE', #15875, 2.000000000000001776 ) ;
#20030 = AXIS2_PLACEMENT_3D ( 'NONE', #4735, #15974, #15418 ) ;
#20031 = CARTESIAN_POINT ( 'NONE',  ( 14.99999662536863632, -77.94228634059960825, -9.999999999999998224 ) ) ;
#20032 = LINE ( 'NONE', #30916, #32400 ) ;
#20033 = AXIS2_PLACEMENT_3D ( 'NONE', #11526, #13973, #28235 ) ;
#20034 = DIRECTION ( 'NONE',  ( 0.000000000000000000, 0.000000000000000000, 1.000000000000000000 ) ) ;
#20035 = ORIENTED_EDGE ( 'NONE', *, *, #9866, .T. ) ;
#20036 = AXIS2_PLACEMENT_3D ( 'NONE', #36186, #1875, #24384 ) ;
#20037 = FACE_BOUND ( 'NONE', #21701, .T. ) ;
#20038 = ORIENTED_EDGE ( 'NONE', *, *, #20069, .T. ) ;
#20039 = EDGE_LOOP ( 'NONE', ( #15770, #7784, #34494, #21523, #27868 ) ) ;
#20040 = EDGE_CURVE ( 'NONE', #7675, #7436, #12840, .T. ) ;
#20041 = CARTESIAN_POINT ( 'NONE',  ( -63.00000337463106348, -60.62177826491083010, 12.50000000000000000 ) ) ;
#20042 = EDGE_LOOP ( 'NONE', ( #7491, #21163 ) ) ;
#20043 = AXIS2_PLACEMENT_3D ( 'NONE', #5616, #17052, #28482 ) ;
#20044 = VECTOR ( 'NONE', #23039, 1000.000000000000000 ) ;
#20045 = AXIS2_PLACEMENT_3D ( 'NONE', #24104, #29165, #1235 ) ;
#20046 = DIRECTION ( 'NONE',  ( 0.000000000000000000, 0.000000000000000000, 1.000000000000000000 ) ) ;
#20047 = DIRECTION ( 'NONE',  ( -1.000000000000000000, 0.000000000000000000, 0.000000000000000000 ) ) ;
#20048 = ORIENTED_EDGE ( 'NONE', *, *, #5687, .T. ) ;
#20049 = EDGE_LOOP ( 'NONE', ( #35688, #16733, #21056 ) ) ;
#20050 = EDGE_LOOP ( 'NONE', ( #935, #4599, #22266, #18562 ) ) ;
#20051 = ORIENTED_EDGE ( 'NONE', *, *, #5221, .F. ) ;
#20052 = ORIENTED_EDGE ( 'NONE', *, *, #34444, .T. ) ;
#20054 = CARTESIAN_POINT ( 'NONE',  ( 76.99999662536836809, 43.30127018922198801, 12.50000000000000000 ) ) ;
#20053 = CIRCLE ( 'NONE', #5694, 25.00000000000000000 ) ;
#20055 = DIRECTION ( 'NONE',  ( 0.000000000000000000, 0.000000000000000000, -1.000000000000000000 ) ) ;
#20056 = CIRCLE ( 'NONE', #2697, 2.000000000000001776 ) ;
#20057 = CARTESIAN_POINT ( 'NONE',  ( 42.99999662536850309, 77.94228634059959404, 17.49999999999999645 ) ) ;
#20058 = CARTESIAN_POINT ( 'NONE',  ( 59.99999662536842493, -51.96152422706639840, 12.50000000000000000 ) ) ;
#20059 = CARTESIAN_POINT ( 'NONE',  ( 4.999999999998231637, -2.092670831923694408, -4.100100627019599209 ) ) ;
#20060 = EDGE_CURVE ( 'NONE', #719, #24333, #14637, .T. ) ;
#20061 = ORIENTED_EDGE ( 'NONE', *, *, #24091, .T. ) ;
#20062 = AXIS2_PLACEMENT_3D ( 'NONE', #16099, #27521, #5009 ) ;
#20063 = CARTESIAN_POINT ( 'NONE',  ( 0.000000000000000000, 89.94802294027097389, 32.49999999999990052 ) ) ;
#20064 = AXIS2_PLACEMENT_3D ( 'NONE', #23583, #35235, #15141 ) ;
#20065 = DIRECTION ( 'NONE',  ( 0.000000000000000000, 0.000000000000000000, -1.000000000000000000 ) ) ;
#20066 = DIRECTION ( 'NONE',  ( 0.000000000000000000, 0.000000000000000000, 1.000000000000000000 ) ) ;
#20067 = ORIENTED_EDGE ( 'NONE', *, *, #16327, .F. ) ;
#20068 = CARTESIAN_POINT ( 'NONE',  ( -53.00000337463110611, -43.30127018922202353, -9.999999999999998224 ) ) ;
#20069 = EDGE_CURVE ( 'NONE', #2324, #15669, #1977, .T. ) ;
#20070 = DIRECTION ( 'NONE',  ( -0.000000000000000000, -0.000000000000000000, 1.000000000000000000 ) ) ;
#20071 = CIRCLE ( 'NONE', #3903, 2.000000000000001776 ) ;
#20072 = ORIENTED_EDGE ( 'NONE', *, *, #19104, .T. ) ;
#20073 = VECTOR ( 'NONE', #6456, 1000.000000000000000 ) ;
#20074 = ORIENTED_EDGE ( 'NONE', *, *, #1869, .F. ) ;
#20075 = ADVANCED_FACE ( 'NONE', ( #5172 ), #13606, .F. ) ;
#20076 = CARTESIAN_POINT ( 'NONE',  ( -45.00000337463111322, -77.94228634059960825, 12.50000000000000000 ) ) ;
#20077 = CYLINDRICAL_SURFACE ( 'NONE', #1978, 2.000000000000001776 ) ;
#20078 = DIRECTION ( 'NONE',  ( 0.000000000000000000, 0.000000000000000000, 1.000000000000000000 ) ) ;
#20079 = CARTESIAN_POINT ( 'NONE',  ( 0.000000000000000000, 0.000000000000000000, 27.50000000000000000 ) ) ;
#20080 = ORIENTED_EDGE ( 'NONE', *, *, #10600, .T. ) ;
#20081 = ORIENTED_EDGE ( 'NONE', *, *, #17714, .T. ) ;
#20082 = LINE ( 'NONE', #23079, #32070 ) ;
#20083 = DIRECTION ( 'NONE',  ( -0.000000000000000000, -0.000000000000000000, -1.000000000000000000 ) ) ;
#20084 = CARTESIAN_POINT ( 'NONE',  ( 74.99999662536835388, -25.98076211353319565, -5.000000000000000000 ) ) ;
#20085 = AXIS2_PLACEMENT_3D ( 'NONE', #14948, #26379, #685 ) ;
#20086 = VERTEX_POINT ( 'NONE', #16610 ) ;
#20087 = EDGE_CURVE ( 'NONE', #12699, #5447, #36304, .T. ) ;
#20088 = VECTOR ( 'NONE', #7174, 1000.000000000000000 ) ;
#20089 = CARTESIAN_POINT ( 'NONE',  ( -70.00000337463099243, 34.64101615137758472, -9.999999999999998224 ) ) ;
#20090 = ORIENTED_EDGE ( 'NONE', *, *, #23154, .T. ) ;
#20091 = CIRCLE ( 'NONE', #19511, 3.000000000000002665 ) ;
#20092 = AXIS2_PLACEMENT_3D ( 'NONE', #24849, #36102, #10401 ) ;
#20093 = ORIENTED_EDGE ( 'NONE', *, *, #1611, .T. ) ;
#20094 = CIRCLE ( 'NONE', #23683, 2.000000000000001776 ) ;
#20095 = DIRECTION ( 'NONE',  ( -0.8660254037844380415, 0.5000000000000008882, 0.000000000000000000 ) ) ;
#20096 = DIRECTION ( 'NONE',  ( 1.000000000000000000, 0.000000000000000000, 0.000000000000000000 ) ) ;
#20097 = ORIENTED_EDGE ( 'NONE', *, *, #6441, .F. ) ;
#20098 = ORIENTED_EDGE ( 'NONE', *, *, #12812, .T. ) ;
#20099 = CARTESIAN_POINT ( 'NONE',  ( -73.00000337463097821, 8.660254037844374864, -9.999999999999998224 ) ) ;
#20100 = EDGE_CURVE ( 'NONE', #27793, #22736, #36813, .T. ) ;
#20101 = CARTESIAN_POINT ( 'NONE',  ( 0.000000000000000000, 0.000000000000000000, -5.000000000000000000 ) ) ;
#20102 = CIRCLE ( 'NONE', #31464, 3.500000000000000888 ) ;
#20103 = CARTESIAN_POINT ( 'NONE',  ( 0.000000000000000000, 89.94802294027088863, -23.00000000000000000 ) ) ;
#20104 = ORIENTED_EDGE ( 'NONE', *, *, #22497, .T. ) ;
#20105 = LINE ( 'NONE', #31533, #33346 ) ;
#20106 = EDGE_CURVE ( 'NONE', #16790, #12255, #7810, .T. ) ;
#20107 = FACE_BOUND ( 'NONE', #18367, .T. ) ;
#20108 = CARTESIAN_POINT ( 'NONE',  ( -52.00000337463109190, 69.28203230275518365, -5.000000000000000000 ) ) ;
#20109 = DIRECTION ( 'NONE',  ( 1.000000000000000000, 0.000000000000000000, 0.000000000000000000 ) ) ;
#20110 = DIRECTION ( 'NONE',  ( 0.000000000000000000, 0.000000000000000000, 1.000000000000000000 ) ) ;
#20111 = DIRECTION ( 'NONE',  ( 1.000000000000000000, 0.000000000000000000, 0.000000000000000000 ) ) ;
#20112 = CIRCLE ( 'NONE', #18317, 3.000000000000006661 ) ;
#20113 = EDGE_CURVE ( 'NONE', #34280, #15339, #33820, .T. ) ;
#20114 = DIRECTION ( 'NONE',  ( 0.000000000000000000, 0.000000000000000000, 1.000000000000000000 ) ) ;
#20115 = AXIS2_PLACEMENT_3D ( 'NONE', #6223, #778, #23307 ) ;
#20116 = DIRECTION ( 'NONE',  ( 1.000000000000000000, 0.000000000000000000, 0.000000000000000000 ) ) ;
#20117 = VERTEX_POINT ( 'NONE', #10966 ) ;
#20118 = CARTESIAN_POINT ( 'NONE',  ( -67.00000337463102085, 25.98076211353317433, -9.999999999999998224 ) ) ;
#20119 = ADVANCED_FACE ( 'NONE', ( #16966 ), #11155, .F. ) ;
#20120 = CARTESIAN_POINT ( 'NONE',  ( -5.253368672218637236, 3.033033817057754877, -4.359491423763649287 ) ) ;
#20121 = DIRECTION ( 'NONE',  ( 0.000000000000000000, 0.000000000000000000, -1.000000000000000000 ) ) ;
#20122 = CIRCLE ( 'NONE', #12913, 2.000000000000001776 ) ;
#20123 = CIRCLE ( 'NONE', #14740, 3.499999999999987566 ) ;
#20124 = ORIENTED_EDGE ( 'NONE', *, *, #33218, .F. ) ;
#20125 = ORIENTED_EDGE ( 'NONE', *, *, #9681, .F. ) ;
#20126 = CIRCLE ( 'NONE', #21923, 30.00000000000000000 ) ;
#20127 = ORIENTED_EDGE ( 'NONE', *, *, #21186, .F. ) ;
#20128 = EDGE_CURVE ( 'NONE', #29187, #12874, #14049, .T. ) ;
#20129 = CARTESIAN_POINT ( 'NONE',  ( -22.00000337463124112, -86.60254037844400443, -9.999999999999998224 ) ) ;
#20130 = CARTESIAN_POINT ( 'NONE',  ( 14.99999662536863632, -77.94228634059960825, 12.50000000000000000 ) ) ;
#20131 = DIRECTION ( 'NONE',  ( 1.000000000000000000, 0.000000000000000000, 0.000000000000000000 ) ) ;
#20132 = ORIENTED_EDGE ( 'NONE', *, *, #6914, .T. ) ;
#20133 = CIRCLE ( 'NONE', #26717, 1.999999999999998224 ) ;
#20134 = FACE_OUTER_BOUND ( 'NONE', #4601, .T. ) ;
#20135 = EDGE_LOOP ( 'NONE', ( #13590, #30475 ) ) ;
#20136 = DIRECTION ( 'NONE',  ( -0.000000000000000000, 0.000000000000000000, 1.000000000000000000 ) ) ;
#20137 = VERTEX_POINT ( 'NONE', #8536 ) ;
#20138 = CARTESIAN_POINT ( 'NONE',  ( 44.99999662536849598, 60.62177826491077326, -5.000000000000000000 ) ) ;
#20139 = ORIENTED_EDGE ( 'NONE', *, *, #6531, .F. ) ;
#20140 = AXIS2_PLACEMENT_3D ( 'NONE', #18255, #29684, #18648 ) ;
#20141 = ORIENTED_EDGE ( 'NONE', *, *, #26252, .F. ) ;
#20142 = EDGE_CURVE ( 'NONE', #34714, #16004, #21762, .T. ) ;
#20143 = DIRECTION ( 'NONE',  ( -1.000000000000000000, -0.000000000000000000, -0.000000000000000000 ) ) ;
#20144 = CIRCLE ( 'NONE', #8158, 2.000000000000001776 ) ;
#20145 = CARTESIAN_POINT ( 'NONE',  ( 145.0000000000000284, -6.000000000000504485, 27.50000000000000000 ) ) ;
#20146 = ORIENTED_EDGE ( 'NONE', *, *, #19018, .T. ) ;
#20147 = PRODUCT_DEFINITION_FORMATION_WITH_SPECIFIED_SOURCE ( 'ANY', '', #37010, .NOT_KNOWN. ) ;
#20148 = LINE ( 'NONE', #20892, #27479 ) ;
#20149 = AXIS2_PLACEMENT_3D ( 'NONE', #16785, #34384, #13779 ) ;
#20150 = AXIS2_PLACEMENT_3D ( 'NONE', #1262, #24076, #1012 ) ;
#20151 = AXIS2_PLACEMENT_3D ( 'NONE', #31598, #19812, #34253 ) ;
#20152 = EDGE_CURVE ( 'NONE', #19630, #31778, #1471, .T. ) ;
#20153 = DIRECTION ( 'NONE',  ( 0.000000000000000000, -0.000000000000000000, -1.000000000000000000 ) ) ;
#20154 = CARTESIAN_POINT ( 'NONE',  ( -87.00000337463093558, -25.98076211353322051, 17.49999999999999645 ) ) ;
#20155 = AXIS2_PLACEMENT_3D ( 'NONE', #21306, #32745, #7072 ) ;
#20156 = EDGE_LOOP ( 'NONE', ( #27058, #14668, #18750, #21679 ) ) ;
#20157 = DIRECTION ( 'NONE',  ( 1.000000000000000000, 0.000000000000000000, 0.000000000000000000 ) ) ;
#20158 = DIRECTION ( 'NONE',  ( 0.000000000000000000, 0.000000000000000000, 1.000000000000000000 ) ) ;
#20160 = VERTEX_POINT ( 'NONE', #33851 ) ;
#20159 = EDGE_CURVE ( 'NONE', #7729, #12225, #6266, .T. ) ;
#20161 = CARTESIAN_POINT ( 'NONE',  ( 0.000000000000000000, 0.000000000000000000, 32.50000000000000000 ) ) ;
#20162 = EDGE_CURVE ( 'NONE', #3839, #36232, #23641, .T. ) ;
#20163 = CARTESIAN_POINT ( 'NONE',  ( 61.99999662536842493, -51.96152422706639840, 17.49999999999999645 ) ) ;
#20164 = CARTESIAN_POINT ( 'NONE',  ( 79.99999662536832545, -17.32050807568879591, -9.999999999999998224 ) ) ;
#20165 = DIRECTION ( 'NONE',  ( 0.000000000000000000, 0.000000000000000000, -1.000000000000000000 ) ) ;
#20166 = DIRECTION ( 'NONE',  ( 0.000000000000000000, 0.000000000000000000, 1.000000000000000000 ) ) ;
#20167 = VERTEX_POINT ( 'NONE', #11695 ) ;
#20168 = CARTESIAN_POINT ( 'NONE',  ( -5.854691731421723944E-14, -5.773502691896269745, -0.5999999999999998668 ) ) ;
#20169 = CARTESIAN_POINT ( 'NONE',  ( 76.99999662536836809, 25.98076211353319565, -9.999999999999998224 ) ) ;
#20170 = CIRCLE ( 'NONE', #373, 2.000000000000001776 ) ;
#20171 = VERTEX_POINT ( 'NONE', #11518 ) ;
#20172 = ORIENTED_EDGE ( 'NONE', *, *, #14503, .F. ) ;
#20173 = ORIENTED_EDGE ( 'NONE', *, *, #36350, .F. ) ;
#20174 = EDGE_CURVE ( 'NONE', #3735, #36464, #4484, .T. ) ;
#20175 = AXIS2_PLACEMENT_3D ( 'NONE', #4309, #1123, #7679 ) ;
#20176 = DIRECTION ( 'NONE',  ( 0.000000000000000000, 0.000000000000000000, 1.000000000000000000 ) ) ;
#20177 = DIRECTION ( 'NONE',  ( 0.000000000000000000, 0.000000000000000000, -1.000000000000000000 ) ) ;
#20178 = ADVANCED_BREP_SHAPE_REPRESENTATION ( '', ( #19388, #21385 ), #23118 ) ;
#20179 = CARTESIAN_POINT ( 'NONE',  ( 0.000000000000000000, 0.000000000000000000, -5.000000000000000000 ) ) ;
#20180 = CARTESIAN_POINT ( 'NONE',  ( -4.279621169095561228, 62.97617850287782915, -4.999999999999997335 ) ) ;
#20181 = VECTOR ( 'NONE', #1243, 1000.000000000000000 ) ;
#20182 = VECTOR ( 'NONE', #34888, 1000.000000000000000 ) ;
#20183 = CIRCLE ( 'NONE', #4016, 3.499999999999989342 ) ;
#20184 = CIRCLE ( 'NONE', #20784, 30.00000000000000000 ) ;
#20185 = CARTESIAN_POINT ( 'NONE',  ( 9.999996625368655856, -69.28203230275519786, -5.000000000000000000 ) ) ;
#20186 = ORIENTED_EDGE ( 'NONE', *, *, #14371, .F. ) ;
#20187 = LINE ( 'NONE', #37079, #29894 ) ;
#20188 = ORIENTED_EDGE ( 'NONE', *, *, #33706, .T. ) ;
#20189 = FACE_BOUND ( 'NONE', #35004, .T. ) ;
#20190 = VECTOR ( 'NONE', #24445, 1000.000000000000000 ) ;
#20191 = EDGE_CURVE ( 'NONE', #14464, #32620, #20340, .T. ) ;
#20192 = DIRECTION ( 'NONE',  ( 0.000000000000000000, 0.000000000000000000, 1.000000000000000000 ) ) ;
#20193 = FACE_OUTER_BOUND ( 'NONE', #21717, .T. ) ;
#20194 = EDGE_CURVE ( 'NONE', #14287, #20625, #28422, .T. ) ;
#20195 = CARTESIAN_POINT ( 'NONE',  ( 0.000000000000000000, 0.000000000000000000, 0.000000000000000000 ) ) ;
#20196 = AXIS2_PLACEMENT_3D ( 'NONE', #9769, #27401, #16164 ) ;
#20197 = EDGE_CURVE ( 'NONE', #28343, #26021, #9258, .T. ) ;
#20198 = FACE_OUTER_BOUND ( 'NONE', #16146, .T. ) ;
#20199 = AXIS2_PLACEMENT_3D ( 'NONE', #13466, #1225, #14918 ) ;
#20200 = FACE_OUTER_BOUND ( 'NONE', #9138, .T. ) ;
#20201 = PLANE ( 'NONE',  #23932 ) ;
#20202 = VERTEX_POINT ( 'NONE', #25609 ) ;
#20203 = DIRECTION ( 'NONE',  ( 0.000000000000000000, 0.000000000000000000, 1.000000000000000000 ) ) ;
#20204 = EDGE_CURVE ( 'NONE', #25880, #9332, #28590, .T. ) ;
#20205 = FACE_OUTER_BOUND ( 'NONE', #12357, .T. ) ;
#20206 = CARTESIAN_POINT ( 'NONE',  ( -30.99999999999944933, 58.88972745734214698, 12.49999999999999822 ) ) ;
#20207 = EDGE_CURVE ( 'NONE', #25010, #16622, #3098, .T. ) ;
#20208 = AXIS2_PLACEMENT_3D ( 'NONE', #447, #34400, #26332 ) ;
#20209 = VECTOR ( 'NONE', #27725, 1000.000000000000000 ) ;
#20210 = EDGE_LOOP ( 'NONE', ( #28755, #20360, #27042, #10229, #24012, #19540, #3526, #16297, #28792, #26998, #28667, #14777, #31300, #14638, #34687, #3602, #35410, #13148, #6834, #14383, #15144, #28036, #20400, #25508, #7076, #19068, #796, #9912, #14124, #2799, #18314, #3578, #19329, #6559, #11466, #18146, #25085, #16639, #28777, #27945, #13942, #36361, #17671, #15646, #2518, #1145, #36439, #34341, #30893, #33572, #32571, #14994, #4300, #16497, #6934, #16336, #5858, #33134, #13413, #9698, #35844, #4955, #28264, #14339, #19235, #11106, #6440, #29484, #8494, #7452, #21649, #32626, #30341, #9108, #15289, #19427, #16171, #2077, #9804, #36140, #3884, #12088, #12778, #9546, #6990, #34043, #15551, #26427, #9257, #12622, #36228, #20547, #13941, #25865, #22957, #20661, #24163, #8743, #29114, #2151, #2230, #35915, #21053, #36847, #23013, #34974, #28302, #35581, #291, #35605, #35920, #35439, #5550, #13953, #31469, #15914, #4176, #37037, #8526, #12779, #16291, #10210, #25230, #1720, #13320, #4761, #36425, #10003, #27984, #28720, #1547, #32002, #6621, #23954, #36589, #13507, #10797, #20478, #4242, #31266, #31743, #9022, #17451, #9170, #35304, #28747, #2015, #28536, #8335, #36606, #9583, #18944, #35565, #7659, #4507, #28028, #15451, #12771, #22191, #30497, #21216, #14160, #11599, #29117, #24346, #30678, #14424, #26154, #20686, #27227, #8690, #27160, #29433, #18982, #25259, #36444, #32108, #185, #30365, #12386, #3145, #23708, #10364, #33967, #33618, #24429, #9059, #14980, #13343, #10190, #9554, #15555, #17354, #25911, #9442, #31402, #22660, #17030, #28138 ) ) ;
#20211 = CIRCLE ( 'NONE', #8828, 3.000000000000002220 ) ;
#20212 = VERTEX_POINT ( 'NONE', #20154 ) ;
#20213 = ORIENTED_EDGE ( 'NONE', *, *, #23168, .F. ) ;
#20214 = AXIS2_PLACEMENT_3D ( 'NONE', #4070, #9864, #21304 ) ;
#20215 = ADVANCED_FACE ( 'NONE', ( #16807 ), #31580, .F. ) ;
#20216 = EDGE_CURVE ( 'NONE', #13186, #10841, #2538, .T. ) ;
#20217 = FACE_BOUND ( 'NONE', #22843, .T. ) ;
#20218 = EDGE_CURVE ( 'NONE', #23471, #10338, #19389, .T. ) ;
#20219 = CIRCLE ( 'NONE', #19029, 33.00000000000001421 ) ;
#20220 = ADVANCED_FACE ( 'NONE', ( #22602 ), #8012, .T. ) ;
#20221 = CARTESIAN_POINT ( 'NONE',  ( 9.999996625368655856, -86.60254037844400443, 17.49999999999999645 ) ) ;
#20222 = CARTESIAN_POINT ( 'NONE',  ( -98.28784258493107018, -106.7731239591678474, 32.55002500000000509 ) ) ;
#20223 = CARTESIAN_POINT ( 'NONE',  ( 0.000000000000000000, 0.000000000000000000, 17.49999999999999645 ) ) ;
#20224 = AXIS2_PLACEMENT_3D ( 'NONE', #8735, #31949, #37069 ) ;
#20225 = AXIS2_PLACEMENT_3D ( 'NONE', #17653, #11481, #56 ) ;
#20226 = CARTESIAN_POINT ( 'NONE',  ( 67.99999662536839651, 51.96152422706640550, -9.999999999999998224 ) ) ;
#20227 = EDGE_LOOP ( 'NONE', ( #32615, #5311 ) ) ;
#20228 = AXIS2_PLACEMENT_3D ( 'NONE', #4679, #4863, #7471 ) ;
#20229 = ORIENTED_EDGE ( 'NONE', *, *, #6220, .T. ) ;
#20230 = PLANE ( 'NONE',  #20640 ) ;
#20231 = CIRCLE ( 'NONE', #21435, 3.000000000000004885 ) ;
#20232 = DIRECTION ( 'NONE',  ( 1.000000000000000000, 0.000000000000000000, 0.000000000000000000 ) ) ;
#20233 = DIRECTION ( 'NONE',  ( 1.000000000000000000, 0.000000000000000000, 0.000000000000000000 ) ) ;
#20234 = ORIENTED_EDGE ( 'NONE', *, *, #35330, .F. ) ;
#20235 = AXIS2_PLACEMENT_3D ( 'NONE', #31109, #13855, #31454 ) ;
#20236 = FACE_BOUND ( 'NONE', #18955, .T. ) ;
#20237 = VERTEX_POINT ( 'NONE', #14353 ) ;
#20238 = ORIENTED_EDGE ( 'NONE', *, *, #30891, .T. ) ;
#20239 = DIRECTION ( 'NONE',  ( 0.000000000000000000, 0.000000000000000000, 1.000000000000000000 ) ) ;
#20240 = ORIENTED_EDGE ( 'NONE', *, *, #23623, .F. ) ;
#20241 = AXIS2_PLACEMENT_3D ( 'NONE', #19805, #31228, #16974 ) ;
#20242 = PRODUCT ( 'mounting backplate', 'mounting backplate', '', ( #1422 ) ) ;
#20243 = LINE ( 'NONE', #721, #29586 ) ;
#20244 = AXIS2_PLACEMENT_3D ( 'NONE', #596, #23648, #5865 ) ;
#20245 = CARTESIAN_POINT ( 'NONE',  ( 0.000000000000000000, 0.000000000000000000, 12.49999999999999822 ) ) ;
#20246 = VERTEX_POINT ( 'NONE', #25799 ) ;
#20247 = VERTEX_POINT ( 'NONE', #17352 ) ;
#20248 = CIRCLE ( 'NONE', #16091, 95.00000000000000000 ) ;
#20249 = ORIENTED_EDGE ( 'NONE', *, *, #3237, .F. ) ;
#20250 = AXIS2_PLACEMENT_3D ( 'NONE', #17014, #5773, #8411 ) ;
#20251 = ORIENTED_EDGE ( 'NONE', *, *, #22154, .F. ) ;
#20252 = CIRCLE ( 'NONE', #2899, 2.000000000000001776 ) ;
#20253 = ORIENTED_EDGE ( 'NONE', *, *, #5046, .T. ) ;
#20254 = CARTESIAN_POINT ( 'NONE',  ( -30.00000337463119848, -69.28203230275522628, -9.999999999999998224 ) ) ;
#20255 = DIRECTION ( 'NONE',  ( -0.000000000000000000, -0.000000000000000000, 1.000000000000000000 ) ) ;
#20256 = LINE ( 'NONE', #360, #22057 ) ;
#20257 = CYLINDRICAL_SURFACE ( 'NONE', #16324, 2.000000000000001776 ) ;
#20258 = DIRECTION ( 'NONE',  ( 0.000000000000000000, 0.000000000000000000, -1.000000000000000000 ) ) ;
#20259 = VERTEX_POINT ( 'NONE', #28776 ) ;
#20260 = CARTESIAN_POINT ( 'NONE',  ( -52.00000337463109190, 69.28203230275518365, -9.999999999999998224 ) ) ;
#20261 = VECTOR ( 'NONE', #14900, 1000.000000000000000 ) ;
#20262 = DIRECTION ( 'NONE',  ( 0.7071067811865536790, 0.7071067811865414665, 0.000000000000000000 ) ) ;
#20263 = ADVANCED_FACE ( 'NONE', ( #14525 ), #15681, .F. ) ;
#20264 = FACE_OUTER_BOUND ( 'NONE', #8243, .T. ) ;
#20265 = ORIENTED_EDGE ( 'NONE', *, *, #5784, .T. ) ;
#20266 = CARTESIAN_POINT ( 'NONE',  ( 34.00000000000000000, 103.4105893997321743, 32.50000000000000000 ) ) ;
#20267 = CARTESIAN_POINT ( 'NONE',  ( 3.000000000000000000, 2.935248768560057453, -3.903127820947815962E-15 ) ) ;
#20268 = VECTOR ( 'NONE', #27706, 1000.000000000000000 ) ;
#20269 = ORIENTED_EDGE ( 'NONE', *, *, #8533, .T. ) ;
#20270 = ORIENTED_EDGE ( 'NONE', *, *, #3782, .F. ) ;
#20271 = DIRECTION ( 'NONE',  ( -0.8660254037844455910, -0.4999999999999878431, 0.000000000000000000 ) ) ;
#20272 = AXIS2_PLACEMENT_3D ( 'NONE', #26419, #724, #6552 ) ;
#20273 = CARTESIAN_POINT ( 'NONE',  ( -31.74999999999995737, 3.673940397442060854E-16, -3.000000000000000888 ) ) ;
#20274 = CARTESIAN_POINT ( 'NONE',  ( 11.99999662536861855, 69.28203230275516944, -9.999999999999998224 ) ) ;
#20275 = CYLINDRICAL_SURFACE ( 'NONE', #37056, 2.000000000000000000 ) ;
#20276 = ORIENTED_EDGE ( 'NONE', *, *, #12048, .T. ) ;
#20277 = VECTOR ( 'NONE', #14522, 1000.000000000000000 ) ;
#20278 = CARTESIAN_POINT ( 'NONE',  ( 3.000000000000000000, 2.201436576420042535, 1.270999999999998353 ) ) ;
#20279 = CARTESIAN_POINT ( 'NONE',  ( -40.98360655737706537, 111.1639425680974682, -11.00000000000000355 ) ) ;
#20280 = CARTESIAN_POINT ( 'NONE',  ( 5.000000000000000888, -1.936377641173859798, -5.802630826755080129 ) ) ;
#20281 = VERTEX_POINT ( 'NONE', #20937 ) ;
#20282 = VECTOR ( 'NONE', #26129, 1000.000000000000000 ) ;
#20283 = LINE ( 'NONE', #392, #15996 ) ;
#20284 = ORIENTED_EDGE ( 'NONE', *, *, #5268, .F. ) ;
#20285 = ADVANCED_FACE ( 'NONE', ( #27100 ), #27283, .T. ) ;
#20286 = CIRCLE ( 'NONE', #3537, 2.000000000000001776 ) ;
#20287 = EDGE_CURVE ( 'NONE', #12924, #13995, #29535, .T. ) ;
#20288 = ORIENTED_EDGE ( 'NONE', *, *, #20287, .T. ) ;
#20289 = CIRCLE ( 'NONE', #25104, 95.00000000000001421 ) ;
#20290 = DIRECTION ( 'NONE',  ( -0.000000000000000000, -0.000000000000000000, 1.000000000000000000 ) ) ;
#20291 = CARTESIAN_POINT ( 'NONE',  ( 35.19434990244975126, -52.39915983220758022, -4.999999999999997335 ) ) ;
#20292 = ORIENTED_EDGE ( 'NONE', *, *, #3572, .F. ) ;
#20293 = ORIENTED_EDGE ( 'NONE', *, *, #11843, .T. ) ;
#20294 = FACE_OUTER_BOUND ( 'NONE', #25309, .T. ) ;
#20295 = DIRECTION ( 'NONE',  ( -1.000000000000000000, 0.000000000000000000, 0.000000000000000000 ) ) ;
#20296 = EDGE_CURVE ( 'NONE', #30820, #12760, #1606, .T. ) ;
#20297 = ORIENTED_EDGE ( 'NONE', *, *, #27040, .T. ) ;
#20298 = DIRECTION ( 'NONE',  ( 0.000000000000000000, 0.000000000000000000, 1.000000000000000000 ) ) ;
#20299 = AXIS2_PLACEMENT_3D ( 'NONE', #34101, #13655, #11202 ) ;
#20300 = FACE_BOUND ( 'NONE', #13443, .T. ) ;
#20301 = CARTESIAN_POINT ( 'NONE',  ( -94.55012560584668790, 9.234378588655390629, 32.50000000000000000 ) ) ;
#20302 = DIRECTION ( 'NONE',  ( -1.000000000000000000, 0.000000000000000000, -0.000000000000000000 ) ) ;
#20303 = CARTESIAN_POINT ( 'NONE',  ( -72.00000337463100664, 51.96152422706637708, 17.49999999999999645 ) ) ;
#20304 = DIRECTION ( 'NONE',  ( 0.000000000000000000, 0.000000000000000000, 1.000000000000000000 ) ) ;
#20305 = CARTESIAN_POINT ( 'NONE',  ( -65.00000337463104927, -25.98076211353322051, -9.999999999999998224 ) ) ;
#20306 = AXIS2_PLACEMENT_3D ( 'NONE', #6246, #2700, #3084 ) ;
#20307 = EDGE_CURVE ( 'NONE', #20787, #25733, #25387, .T. ) ;
#20308 = CARTESIAN_POINT ( 'NONE',  ( 3.000000000000000000, 2.935248768560057453, -3.903127820947815962E-15 ) ) ;
#20309 = ORIENTED_EDGE ( 'NONE', *, *, #1405, .T. ) ;
#20310 = CARTESIAN_POINT ( 'NONE',  ( -25.30168483247182820, 79.91940249752995840, -5.000000000000000000 ) ) ;
#20311 = DIRECTION ( 'NONE',  ( 1.000000000000000000, 0.000000000000000000, 0.000000000000000000 ) ) ;
#20312 = DIRECTION ( 'NONE',  ( -0.000000000000000000, -0.000000000000000000, 1.000000000000000000 ) ) ;
#20313 = MANIFOLD_SOLID_BREP ( 'CirPattern1', #8219 ) ;
#20314 = CIRCLE ( 'NONE', #8362, 2.000000000000001776 ) ;
#20315 = VERTEX_POINT ( 'NONE', #35198 ) ;
#20316 = VERTEX_POINT ( 'NONE', #30100 ) ;
#20317 = CIRCLE ( 'NONE', #34093, 2.000000000000001776 ) ;
#20318 = ORIENTED_EDGE ( 'NONE', *, *, #5572, .F. ) ;
#20319 = CARTESIAN_POINT ( 'NONE',  ( 7.999996625368625658, 86.60254037844397601, -9.999999999999998224 ) ) ;
#20320 = DIRECTION ( 'NONE',  ( 0.000000000000000000, 0.000000000000000000, 1.000000000000000000 ) ) ;
#20321 = CARTESIAN_POINT ( 'NONE',  ( 7.999996625368618552, 69.28203230275516944, 17.49999999999999645 ) ) ;
#20322 = ORIENTED_EDGE ( 'NONE', *, *, #15606, .F. ) ;
#20323 = DIRECTION ( 'NONE',  ( -0.000000000000000000, -0.000000000000000000, 1.000000000000000000 ) ) ;
#20324 = CIRCLE ( 'NONE', #10168, 3.750000000000001776 ) ;
#20325 = VERTEX_POINT ( 'NONE', #18679 ) ;
#20326 = EDGE_CURVE ( 'NONE', #12419, #34764, #34352, .T. ) ;
#20327 = CARTESIAN_POINT ( 'NONE',  ( -77.00000337463099243, -25.98076211353322051, -9.999999999999998224 ) ) ;
#20328 = VERTEX_POINT ( 'NONE', #12271 ) ;
#20329 = VECTOR ( 'NONE', #27341, 1000.000000000000000 ) ;
#20330 = CARTESIAN_POINT ( 'NONE',  ( 83.67878100130371877, -27.78182860042797131, -4.999999999999997335 ) ) ;
#20331 = EDGE_LOOP ( 'NONE', ( #18801, #36717, #15771, #21254 ) ) ;
#20332 = ORIENTED_EDGE ( 'NONE', *, *, #14503, .T. ) ;
#20333 = FACE_OUTER_BOUND ( 'NONE', #26034, .T. ) ;
#20334 = DIRECTION ( 'NONE',  ( -1.053683889111837881E-14, -1.000000000000000000, 0.000000000000000000 ) ) ;
#20335 = EDGE_CURVE ( 'NONE', #35643, #33480, #27751, .T. ) ;
#20336 = EDGE_LOOP ( 'NONE', ( #4868, #10710, #27501, #8001 ) ) ;
#20337 = FACE_OUTER_BOUND ( 'NONE', #3090, .T. ) ;
#20338 = CIRCLE ( 'NONE', #32927, 2.000000000000001776 ) ;
#20339 = CYLINDRICAL_SURFACE ( 'NONE', #29418, 2.000000000000001776 ) ;
#20340 = LINE ( 'NONE', #13963, #13974 ) ;
#20341 = CONICAL_SURFACE ( 'NONE', #4189, 2.445500000000000007, 0.7853981633974616017 ) ;
#20342 = EDGE_CURVE ( 'NONE', #3626, #11344, #6683, .T. ) ;
#20343 = EDGE_LOOP ( 'NONE', ( #27587, #6066 ) ) ;
#20344 = CARTESIAN_POINT ( 'NONE',  ( -12.97563234535667753, 90.60231327712331506, -4.999999999999997335 ) ) ;
#20345 = CARTESIAN_POINT ( 'NONE',  ( 71.99999662536839651, 17.32050807568879236, -9.999999999999998224 ) ) ;
#20346 = EDGE_LOOP ( 'NONE', ( #19142, #32372, #11810, #34351 ) ) ;
#20347 = VECTOR ( 'NONE', #18424, 999.9999999999998863 ) ;
#20348 = CARTESIAN_POINT ( 'NONE',  ( 32.99999662536855283, 60.62177826491078747, -9.999999999999998224 ) ) ;
#20349 = DIRECTION ( 'NONE',  ( 0.000000000000000000, 0.000000000000000000, 1.000000000000000000 ) ) ;
#20350 = CARTESIAN_POINT ( 'NONE',  ( 36.99999662536853862, 77.94228634059959404, -9.999999999999998224 ) ) ;
#20351 = CARTESIAN_POINT ( 'NONE',  ( -4.166666666666670515, 3.367876570272800407, -3.818275046351158775 ) ) ;
#20352 = CARTESIAN_POINT ( 'NONE',  ( 4.279621169095998212, -62.97617850287780072, 12.49999999999999822 ) ) ;
#20353 = CIRCLE ( 'NONE', #23951, 2.000000000000000000 ) ;
#20354 = VERTEX_POINT ( 'NONE', #15297 ) ;
#20355 = AXIS2_PLACEMENT_3D ( 'NONE', #34825, #9119, #31966 ) ;
#20356 = DIRECTION ( 'NONE',  ( 0.000000000000000000, 0.000000000000000000, -1.000000000000000000 ) ) ;
#20357 = CARTESIAN_POINT ( 'NONE',  ( -55.00000337463107059, 43.30127018922197379, 12.50000000000000000 ) ) ;
#20358 = ORIENTED_EDGE ( 'NONE', *, *, #12802, .T. ) ;
#20359 = EDGE_CURVE ( 'NONE', #7909, #19401, #11573, .T. ) ;
#20360 = ORIENTED_EDGE ( 'NONE', *, *, #31840, .T. ) ;
#20361 = VERTEX_POINT ( 'NONE', #6855 ) ;
#20362 = DIRECTION ( 'NONE',  ( 0.000000000000000000, 0.000000000000000000, -1.000000000000000000 ) ) ;
#20363 = CARTESIAN_POINT ( 'NONE',  ( 1.999996625368710257, -69.28203230275519786, 17.49999999999999645 ) ) ;
#20364 = CYLINDRICAL_SURFACE ( 'NONE', #13459, 2.000000000000001776 ) ;
#20365 = CIRCLE ( 'NONE', #17327, 17.55872235085559652 ) ;
#20366 = EDGE_CURVE ( 'NONE', #31806, #27793, #18294, .T. ) ;
#20367 = CARTESIAN_POINT ( 'NONE',  ( 24.99999662536859546, -77.94228634059960825, -9.999999999999998224 ) ) ;
#20368 = ORIENTED_EDGE ( 'NONE', *, *, #16332, .T. ) ;
#20369 = EDGE_CURVE ( 'NONE', #2346, #20659, #21292, .T. ) ;
#20370 = VECTOR ( 'NONE', #16527, 1000.000000000000000 ) ;
#20371 = CARTESIAN_POINT ( 'NONE',  ( 2.999996625368676728, -77.94228634059960825, -9.999999999999998224 ) ) ;
#20372 = VERTEX_POINT ( 'NONE', #7059 ) ;
#20374 = AXIS2_PLACEMENT_3D ( 'NONE', #21362, #1472, #26985 ) ;
#20373 = FACE_BOUND ( 'NONE', #28119, .T. ) ;
#20375 = FACE_OUTER_BOUND ( 'NONE', #32274, .T. ) ;
#20376 = VECTOR ( 'NONE', #35590, 1000.000000000000000 ) ;
#20377 = DIRECTION ( 'NONE',  ( 1.000000000000000000, 0.000000000000000000, 0.000000000000000000 ) ) ;
#20378 = DIRECTION ( 'NONE',  ( 0.000000000000000000, 0.000000000000000000, 1.000000000000000000 ) ) ;
#20379 = APPLICATION_PROTOCOL_DEFINITION ( 'draft international standard', 'automotive_design', 1998, #12741 ) ;
#20380 = CARTESIAN_POINT ( 'NONE',  ( 0.000000000000000000, 0.000000000000000000, 32.50000000000000000 ) ) ;
#20381 = EDGE_CURVE ( 'NONE', #33432, #33197, #5014, .T. ) ;
#20382 = DIRECTION ( 'NONE',  ( -1.000000000000000000, -0.000000000000000000, -0.000000000000000000 ) ) ;
#20383 = DIRECTION ( 'NONE',  ( 0.000000000000000000, 0.000000000000000000, -1.000000000000000000 ) ) ;
#20384 = EDGE_LOOP ( 'NONE', ( #34922, #19440 ) ) ;
#20385 = CIRCLE ( 'NONE', #19, 27.00000000000001421 ) ;
#20386 = DIRECTION ( 'NONE',  ( 0.000000000000000000, 0.000000000000000000, 1.000000000000000000 ) ) ;
#20387 = CARTESIAN_POINT ( 'NONE',  ( 19.99999662536857770, 86.60254037844397601, 17.49999999999999645 ) ) ;
#20388 = DIRECTION ( 'NONE',  ( -1.000000000000000000, 0.000000000000000000, 0.000000000000000000 ) ) ;
#20389 = ORIENTED_EDGE ( 'NONE', *, *, #12762, .F. ) ;
#20390 = ORIENTED_EDGE ( 'NONE', *, *, #27502, .T. ) ;
#20391 = CIRCLE ( 'NONE', #31161, 100.0000000000000142 ) ;
#20392 = ORIENTED_EDGE ( 'NONE', *, *, #34972, .F. ) ;
#20393 = DIRECTION ( 'NONE',  ( 1.000000000000000000, 0.000000000000000000, 0.000000000000000000 ) ) ;
#20394 = ADVANCED_FACE ( 'NONE', ( #7611 ), #34542, .F. ) ;
#20395 = CARTESIAN_POINT ( 'NONE',  ( 79.99999662536832545, -17.32050807568879591, 12.50000000000000000 ) ) ;
#20396 = FACE_OUTER_BOUND ( 'NONE', #13833, .T. ) ;
#20397 = EDGE_CURVE ( 'NONE', #17463, #3839, #31521, .T. ) ;
#20398 = DIRECTION ( 'NONE',  ( 3.554796214472773777E-16, 1.000000000000000000, -0.000000000000000000 ) ) ;
#20399 = CARTESIAN_POINT ( 'NONE',  ( -55.00000337463107059, 43.30127018922197379, -5.000000000000000000 ) ) ;
#20400 = ORIENTED_EDGE ( 'NONE', *, *, #35550, .T. ) ;
#20401 = EDGE_CURVE ( 'NONE', #30139, #36972, #6207, .T. ) ;
#20402 = ORIENTED_EDGE ( 'NONE', *, *, #11798, .T. ) ;
#20403 = CARTESIAN_POINT ( 'NONE',  ( -18.03953374218250971, 86.20686523360116382, 12.50000000000000000 ) ) ;
#20404 = FACE_OUTER_BOUND ( 'NONE', #5421, .T. ) ;
#20405 = LINE ( 'NONE', #11418, #30489 ) ;
#20406 = ADVANCED_FACE ( 'NONE', ( #5658 ), #22052, .T. ) ;
#20407 = ORIENTED_EDGE ( 'NONE', *, *, #28529, .T. ) ;
#20408 = ADVANCED_FACE ( 'NONE', ( #1801 ), #28339, .T. ) ;
#20409 = DIRECTION ( 'NONE',  ( -1.000000000000000000, 0.000000000000000000, 0.000000000000000000 ) ) ;
#20410 = ORIENTED_EDGE ( 'NONE', *, *, #18323, .T. ) ;
#20411 = ORIENTED_EDGE ( 'NONE', *, *, #22269, .T. ) ;
#20412 = VECTOR ( 'NONE', #20807, 1000.000000000000000 ) ;
#20413 = DIRECTION ( 'NONE',  ( 0.000000000000000000, 0.000000000000000000, 1.000000000000000000 ) ) ;
#20414 = EDGE_LOOP ( 'NONE', ( #3632, #27154 ) ) ;
#20415 = EDGE_CURVE ( 'NONE', #16670, #21710, #31363, .T. ) ;
#20416 = EDGE_CURVE ( 'NONE', #33988, #16224, #27486, .T. ) ;
#20417 = DIRECTION ( 'NONE',  ( 0.000000000000000000, 0.000000000000000000, 1.000000000000000000 ) ) ;
#20418 = ADVANCED_FACE ( 'NONE', ( #16242 ), #28726, .F. ) ;
#20419 = FACE_BOUND ( 'NONE', #27385, .T. ) ;
#20420 = ADVANCED_FACE ( 'NONE', ( #17099 ), #16916, .T. ) ;
#20421 = ORIENTED_EDGE ( 'NONE', *, *, #14115, .F. ) ;
#20422 = EDGE_CURVE ( 'NONE', #27517, #32313, #205, .T. ) ;
#20423 = ORIENTED_EDGE ( 'NONE', *, *, #642, .F. ) ;
#20424 = EDGE_LOOP ( 'NONE', ( #26990, #23606, #26876, #27371 ) ) ;
#20425 = VERTEX_POINT ( 'NONE', #19059 ) ;
#20426 = ORIENTED_EDGE ( 'NONE', *, *, #19945, .F. ) ;
#20427 = DIRECTION ( 'NONE',  ( 0.000000000000000000, 0.000000000000000000, 1.000000000000000000 ) ) ;
#20428 = DIRECTION ( 'NONE',  ( -0.000000000000000000, 0.000000000000000000, -1.000000000000000000 ) ) ;
#20429 = LINE ( 'NONE', #17269, #2299 ) ;
#20430 = CARTESIAN_POINT ( 'NONE',  ( 71.20511420343271425, 36.23716514913449060, 12.50000000000000000 ) ) ;
#20431 = CARTESIAN_POINT ( 'NONE',  ( -66.86787810013036903, 2.778182860042780700, -49.86348611802629449 ) ) ;
#20432 = EDGE_LOOP ( 'NONE', ( #24640, #26939, #25383, #35691, #23276, #30897 ) ) ;
#20433 = FACE_OUTER_BOUND ( 'NONE', #3823, .T. ) ;
#20434 = CARTESIAN_POINT ( 'NONE',  ( 79.99999662536832545, -17.32050807568879591, 12.50000000000000000 ) ) ;
#20435 = DIRECTION ( 'NONE',  ( 0.000000000000000000, 0.000000000000000000, 1.000000000000000000 ) ) ;
#20436 = EDGE_LOOP ( 'NONE', ( #4651, #32690 ) ) ;
#20437 = DIRECTION ( 'NONE',  ( -0.000000000000000000, 0.000000000000000000, -1.000000000000000000 ) ) ;
#20438 = CARTESIAN_POINT ( 'NONE',  ( 7.999996625368618552, 69.28203230275516944, -9.999999999999998224 ) ) ;
#20439 = ORIENTED_EDGE ( 'NONE', *, *, #27328, .F. ) ;
#20440 = VERTEX_POINT ( 'NONE', #13234 ) ;
#20441 = DIRECTION ( 'NONE',  ( 1.000000000000000000, 0.000000000000000000, 0.000000000000000000 ) ) ;
#20442 = CARTESIAN_POINT ( 'NONE',  ( -87.00000337463093558, -25.98076211353322051, -5.000000000000000000 ) ) ;
#20443 = CARTESIAN_POINT ( 'NONE',  ( -44.13139720814437794, -27.49999999999955591, 5.000000000000000888 ) ) ;
#20444 = ORIENTED_EDGE ( 'NONE', *, *, #4655, .F. ) ;
#20445 = DIRECTION ( 'NONE',  ( 1.000000000000000000, 0.000000000000000000, 0.000000000000000000 ) ) ;
#20446 = FACE_BOUND ( 'NONE', #29582, .T. ) ;
#20447 = CARTESIAN_POINT ( 'NONE',  ( -42.97377950131527058, 96.90768712682508124, -11.00000000000000000 ) ) ;
#20448 = ORIENTED_EDGE ( 'NONE', *, *, #18702, .F. ) ;
#20449 = AXIS2_PLACEMENT_3D ( 'NONE', #25017, #25203, #36255 ) ;
#20450 = CIRCLE ( 'NONE', #33649, 2.000000000000001776 ) ;
#20451 = CARTESIAN_POINT ( 'NONE',  ( 3.000000000000000000, 0.000000000000000000, 0.000000000000000000 ) ) ;
#20452 = VERTEX_POINT ( 'NONE', #28532 ) ;
#20453 = DIRECTION ( 'NONE',  ( 0.000000000000000000, 0.000000000000000000, 1.000000000000000000 ) ) ;
#20454 = ADVANCED_FACE ( 'NONE', ( #24679 ), #36111, .F. ) ;
#20455 = FACE_OUTER_BOUND ( 'NONE', #8448, .T. ) ;
#20456 = DIRECTION ( 'NONE',  ( 0.000000000000000000, 0.000000000000000000, 1.000000000000000000 ) ) ;
#20457 = EDGE_CURVE ( 'NONE', #11539, #32632, #18172, .T. ) ;
#20458 = VERTEX_POINT ( 'NONE', #1971 ) ;
#20459 = ORIENTED_EDGE ( 'NONE', *, *, #7100, .T. ) ;
#20460 = CARTESIAN_POINT ( 'NONE',  ( 4.279621169095998212, -62.97617850287780072, -4.999999999999997335 ) ) ;
#20461 = DIRECTION ( 'NONE',  ( 1.000000000000000000, 0.000000000000000000, 0.000000000000000000 ) ) ;
#20462 = CARTESIAN_POINT ( 'NONE',  ( 74.99999662536836809, -8.660254037844401509, -9.999999999999998224 ) ) ;
#20463 = EDGE_LOOP ( 'NONE', ( #6010, #10910, #6730, #748 ) ) ;
#20464 = DIRECTION ( 'NONE',  ( 0.000000000000000000, 0.000000000000000000, -1.000000000000000000 ) ) ;
#20465 = FACE_BOUND ( 'NONE', #32217, .T. ) ;
#20466 = CARTESIAN_POINT ( 'NONE',  ( -5.000000000000000000, -2.886751345948134428, -2.080000000000000071 ) ) ;
#20467 = DIRECTION ( 'NONE',  ( -0.000000000000000000, -0.000000000000000000, 1.000000000000000000 ) ) ;
#20468 = DIRECTION ( 'NONE',  ( 1.000000000000000000, 0.000000000000000000, 0.000000000000000000 ) ) ;
#20469 = CARTESIAN_POINT ( 'NONE',  ( 0.000000000000000000, 0.000000000000000000, 12.49999999999999822 ) ) ;
#20470 = DIRECTION ( 'NONE',  ( 0.000000000000000000, 0.000000000000000000, 1.000000000000000000 ) ) ;
#20471 = CIRCLE ( 'NONE', #3122, 2.000000000000001776 ) ;
#20472 = CARTESIAN_POINT ( 'NONE',  ( -35.00000337463116296, 60.62177826491077326, 17.49999999999999645 ) ) ;
#20473 = ORIENTED_EDGE ( 'NONE', *, *, #32436, .F. ) ;
#20474 = CARTESIAN_POINT ( 'NONE',  ( -75.00000337463097821, 8.660254037844374864, 17.49999999999999645 ) ) ;
#20475 = DIRECTION ( 'NONE',  ( 1.000000000000000000, 0.000000000000000000, 0.000000000000000000 ) ) ;
#20476 = DIRECTION ( 'NONE',  ( 0.000000000000000000, 1.000000000000000000, -1.625241993126352989E-15 ) ) ;
#20477 = EDGE_CURVE ( 'NONE', #24938, #25464, #43, .T. ) ;
#20478 = ORIENTED_EDGE ( 'NONE', *, *, #25765, .T. ) ;
#20479 = VERTEX_POINT ( 'NONE', #25547 ) ;
#20480 = ORIENTED_EDGE ( 'NONE', *, *, #8945, .F. ) ;
#20481 = CARTESIAN_POINT ( 'NONE',  ( -45.00000337463111322, -77.94228634059960825, -5.000000000000000000 ) ) ;
#20482 = DIRECTION ( 'NONE',  ( -1.000000000000000000, 0.000000000000000000, 0.000000000000000000 ) ) ;
#20483 = CYLINDRICAL_SURFACE ( 'NONE', #8839, 2.000000000000001776 ) ;
#20484 = ORIENTED_EDGE ( 'NONE', *, *, #27127, .F. ) ;
#20485 = EDGE_CURVE ( 'NONE', #2978, #19796, #17578, .T. ) ;
#20486 = CARTESIAN_POINT ( 'NONE',  ( -53.00000337463110611, -43.30127018922202353, -9.999999999999998224 ) ) ;
#20487 = AXIS2_PLACEMENT_3D ( 'NONE', #34721, #15016, #26269 ) ;
#20488 = EDGE_LOOP ( 'NONE', ( #26986, #19339, #27799, #23679 ) ) ;
#20489 = DIRECTION ( 'NONE',  ( 0.000000000000000000, 0.000000000000000000, -1.000000000000000000 ) ) ;
#20490 = ORIENTED_EDGE ( 'NONE', *, *, #6188, .T. ) ;
#20491 = DIRECTION ( 'NONE',  ( 0.000000000000000000, 0.000000000000000000, 1.000000000000000000 ) ) ;
#20492 = VERTEX_POINT ( 'NONE', #22746 ) ;
#20493 = EDGE_LOOP ( 'NONE', ( #25596, #28439 ) ) ;
#20494 = DIRECTION ( 'NONE',  ( 0.000000000000000000, 0.000000000000000000, -1.000000000000000000 ) ) ;
#20495 = FACE_BOUND ( 'NONE', #22395, .T. ) ;
#20496 = DIRECTION ( 'NONE',  ( 0.000000000000000000, 0.000000000000000000, 1.000000000000000000 ) ) ;
#20497 = EDGE_CURVE ( 'NONE', #20792, #34742, #25972, .T. ) ;
#20498 = ORIENTED_EDGE ( 'NONE', *, *, #36928, .F. ) ;
#20499 = DIRECTION ( 'NONE',  ( -0.000000000000000000, -0.000000000000000000, 1.000000000000000000 ) ) ;
#20500 = DIRECTION ( 'NONE',  ( 1.000000000000000000, 0.000000000000000000, 0.000000000000000000 ) ) ;
#20501 = CARTESIAN_POINT ( 'NONE',  ( -5.000000000000000888, 2.886751345948107783, -0.5999999999999836575 ) ) ;
#20502 = ORIENTED_EDGE ( 'NONE', *, *, #17249, .T. ) ;
#20503 = FACE_OUTER_BOUND ( 'NONE', #23994, .T. ) ;
#20504 = FACE_OUTER_BOUND ( 'NONE', #36936, .T. ) ;
#20505 = ORIENTED_EDGE ( 'NONE', *, *, #28258, .T. ) ;
#20506 = LINE ( 'NONE', #20348, #26210 ) ;
#20507 = DIRECTION ( 'NONE',  ( 1.000000000000000000, 0.000000000000000000, 0.000000000000000000 ) ) ;
#20508 = CARTESIAN_POINT ( 'NONE',  ( -5.244800587397359770, -2.026986389275642786, -4.190560292650622465 ) ) ;
#20509 = LINE ( 'NONE', #3827, #24267 ) ;
#20510 =( BOUNDED_CURVE ( )  B_SPLINE_CURVE ( 3, ( #6933, #12352, #23823, #35275 ),
 .UNSPECIFIED., .F., .T. ) 
 B_SPLINE_CURVE_WITH_KNOTS ( ( 4, 4 ),
 ( 4.712388980384679016, 6.283185307179586232 ),
 .UNSPECIFIED. ) 
 CURVE ( )  GEOMETRIC_REPRESENTATION_ITEM ( )  RATIONAL_B_SPLINE_CURVE ( ( 1.000000000000000000, 0.8047378541243626060, 0.8047378541243626060, 1.000000000000000000 ) ) 
 REPRESENTATION_ITEM ( '' )  );
#20511 = AXIS2_PLACEMENT_3D ( 'NONE', #35834, #18586, #21742 ) ;
#20512 = DIRECTION ( 'NONE',  ( 0.000000000000000000, 0.000000000000000000, 1.000000000000000000 ) ) ;
#20513 = EDGE_CURVE ( 'NONE', #35481, #11539, #30752, .T. ) ;
#20514 = DIRECTION ( 'NONE',  ( -0.000000000000000000, -0.000000000000000000, 1.000000000000000000 ) ) ;
#20515 = ORIENTED_EDGE ( 'NONE', *, *, #3699, .T. ) ;
#20516 = CARTESIAN_POINT ( 'NONE',  ( -42.00000337463114164, 69.28203230275516944, -9.999999999999998224 ) ) ;
#20517 = DIRECTION ( 'NONE',  ( 0.000000000000000000, 0.000000000000000000, -1.000000000000000000 ) ) ;
#20518 = CARTESIAN_POINT ( 'NONE',  ( 101.4252494179806661, -31.43181965332042438, 32.50001250000000397 ) ) ;
#20519 = EDGE_CURVE ( 'NONE', #34191, #8805, #35567, .T. ) ;
#20520 = ORIENTED_EDGE ( 'NONE', *, *, #249, .T. ) ;
#20521 = ORIENTED_EDGE ( 'NONE', *, *, #14901, .T. ) ;
#20522 = ORIENTED_EDGE ( 'NONE', *, *, #12762, .T. ) ;
#20523 = CIRCLE ( 'NONE', #28316, 2.000000000000001776 ) ;
#20524 = DIRECTION ( 'NONE',  ( 0.000000000000000000, 0.000000000000000000, 1.000000000000000000 ) ) ;
#20525 = DIRECTION ( 'NONE',  ( 0.000000000000000000, 0.000000000000000000, 1.000000000000000000 ) ) ;
#20526 = VECTOR ( 'NONE', #4789, 1000.000000000000000 ) ;
#20527 = EDGE_CURVE ( 'NONE', #8275, #911, #9031, .T. ) ;
#20528 = DIRECTION ( 'NONE',  ( 1.000000000000000000, 0.000000000000000000, 0.000000000000000000 ) ) ;
#20529 = ADVANCED_FACE ( 'NONE', ( #26284 ), #18196, .T. ) ;
#20530 = LINE ( 'NONE', #3500, #35653 ) ;
#20531 = ORIENTED_EDGE ( 'NONE', *, *, #16271, .F. ) ;
#20532 = DIRECTION ( 'NONE',  ( 1.000000000000000000, 0.000000000000000000, 0.000000000000000000 ) ) ;
#20533 = ORIENTED_EDGE ( 'NONE', *, *, #12830, .F. ) ;
#20534 = FACE_BOUND ( 'NONE', #18166, .T. ) ;
#20535 = AXIS2_PLACEMENT_3D ( 'NONE', #9331, #17241, #5990 ) ;
#20536 = CARTESIAN_POINT ( 'NONE',  ( 70.80619744049005249, 84.18124734178236679, 32.50000000000000000 ) ) ;
#20537 = DIRECTION ( 'NONE',  ( 0.000000000000000000, 0.000000000000000000, 1.000000000000000000 ) ) ;
#20538 = EDGE_CURVE ( 'NONE', #12874, #2651, #16415, .T. ) ;
#20539 = ORIENTED_EDGE ( 'NONE', *, *, #22393, .T. ) ;
#20540 = CARTESIAN_POINT ( 'NONE',  ( 0.000000000000000000, 0.000000000000000000, -5.324496230895142901 ) ) ;
#20541 = SHAPE_DEFINITION_REPRESENTATION ( #488, #34443 ) ;
#20542 = CIRCLE ( 'NONE', #883, 27.00000000000001421 ) ;
#20543 = DIRECTION ( 'NONE',  ( -0.000000000000000000, -0.000000000000000000, 1.000000000000000000 ) ) ;
#20544 = AXIS2_PLACEMENT_3D ( 'NONE', #23114, #34568, #31730 ) ;
#20545 = CARTESIAN_POINT ( 'NONE',  ( -3.374631289687624047E-06, -69.28203230275519786, -9.999999999999998224 ) ) ;
#20546 = LINE ( 'NONE', #511, #10752 ) ;
#20547 = ORIENTED_EDGE ( 'NONE', *, *, #9758, .T. ) ;
#20548 = CARTESIAN_POINT ( 'NONE',  ( 79.99999662536832545, -34.64101615137759183, -9.999999999999998224 ) ) ;
#20549 = DIRECTION ( 'NONE',  ( 1.000000000000000000, 0.000000000000000000, 0.000000000000000000 ) ) ;
#20550 = DIRECTION ( 'NONE',  ( -1.000000000000000000, 0.000000000000000000, 0.000000000000000000 ) ) ;
#20551 = VECTOR ( 'NONE', #477, 1000.000000000000000 ) ;
#20552 = EDGE_CURVE ( 'NONE', #5293, #15920, #25994, .T. ) ;
#20553 = ORIENTED_EDGE ( 'NONE', *, *, #32560, .T. ) ;
#20554 = VERTEX_POINT ( 'NONE', #34906 ) ;
#20555 = ADVANCED_FACE ( 'NONE', ( #20455 ), #17470, .F. ) ;
#20556 = EDGE_LOOP ( 'NONE', ( #23765, #20851 ) ) ;
#20557 = AXIS2_PLACEMENT_3D ( 'NONE', #33425, #27606, #7739 ) ;
#20558 = DIRECTION ( 'NONE',  ( 0.000000000000000000, 0.000000000000000000, 1.000000000000000000 ) ) ;
#20559 = AXIS2_PLACEMENT_3D ( 'NONE', #3711, #6323, #17964 ) ;
#20560 = DIRECTION ( 'NONE',  ( 0.000000000000000000, 0.000000000000000000, -1.000000000000000000 ) ) ;
#20561 = FACE_OUTER_BOUND ( 'NONE', #13542, .T. ) ;
#20562 = LINE ( 'NONE', #3331, #21296 ) ;
#20563 = EDGE_CURVE ( 'NONE', #2260, #19941, #33791, .T. ) ;
#20564 = CARTESIAN_POINT ( 'NONE',  ( -70.00000337463099243, 34.64101615137758472, 17.49999999999999645 ) ) ;
#20565 = DIRECTION ( 'NONE',  ( 1.000000000000000000, 0.000000000000000000, 0.000000000000000000 ) ) ;
#20566 = VERTEX_POINT ( 'NONE', #26838 ) ;
#20567 = VECTOR ( 'NONE', #29727, 1000.000000000000000 ) ;
#20568 = ORIENTED_EDGE ( 'NONE', *, *, #19200, .T. ) ;
#20569 = DIRECTION ( 'NONE',  ( 0.000000000000000000, 0.000000000000000000, 1.000000000000000000 ) ) ;
#20570 = EDGE_CURVE ( 'NONE', #21403, #942, #32268, .T. ) ;
#20571 = STYLED_ITEM ( 'NONE', ( #19343 ), #19388 ) ;
#20572 = DIRECTION ( 'NONE',  ( 0.000000000000000000, 0.000000000000000000, 1.000000000000000000 ) ) ;
#20573 = CARTESIAN_POINT ( 'NONE',  ( -35.00000337463116296, 77.94228634059957983, -9.999999999999998224 ) ) ;
#20574 = ORIENTED_EDGE ( 'NONE', *, *, #15163, .F. ) ;
#20575 = FACE_BOUND ( 'NONE', #8959, .T. ) ;
#20576 = ORIENTED_EDGE ( 'NONE', *, *, #28682, .T. ) ;
#20577 = EDGE_LOOP ( 'NONE', ( #26330, #5609, #12702, #15306 ) ) ;
#20578 = DIRECTION ( 'NONE',  ( 1.000000000000000000, 0.000000000000000000, 0.000000000000000000 ) ) ;
#20579 = ORIENTED_EDGE ( 'NONE', *, *, #19618, .F. ) ;
#20580 = PRESENTATION_STYLE_ASSIGNMENT (( #29774 ) ) ;
#20581 = AXIS2_PLACEMENT_3D ( 'NONE', #4040, #15482, #10734 ) ;
#20582 = DIRECTION ( 'NONE',  ( 0.000000000000000000, 0.000000000000000000, -1.000000000000000000 ) ) ;
#20583 = EDGE_CURVE ( 'NONE', #11389, #4196, #9202, .T. ) ;
#20584 = CARTESIAN_POINT ( 'NONE',  ( 3.346878500200757944, 3.841181488860379911, -5.948595712916174172 ) ) ;
#20585 = DIRECTION ( 'NONE',  ( 0.000000000000000000, 0.000000000000000000, 1.000000000000000000 ) ) ;
#20586 = VERTEX_POINT ( 'NONE', #17638 ) ;
#20587 = EDGE_LOOP ( 'NONE', ( #11434, #13828, #6486, #7973 ) ) ;
#20588 = ORIENTED_EDGE ( 'NONE', *, *, #7763, .F. ) ;
#20589 = CIRCLE ( 'NONE', #4454, 2.000000000000001776 ) ;
#20590 = EDGE_CURVE ( 'NONE', #3095, #34263, #11026, .T. ) ;
#20591 = ORIENTED_EDGE ( 'NONE', *, *, #5205, .T. ) ;
#20592 = EDGE_LOOP ( 'NONE', ( #2920, #34500, #16296, #11946 ) ) ;
#20593 = CARTESIAN_POINT ( 'NONE',  ( -8.000003374631281972, 86.60254037844397601, -5.000000000000000000 ) ) ;
#20594 = CIRCLE ( 'NONE', #14022, 2.000000000000001776 ) ;
#20595 = EDGE_CURVE ( 'NONE', #13905, #2028, #5036, .T. ) ;
#20596 = DIRECTION ( 'NONE',  ( -1.000000000000000000, 0.000000000000000000, 0.000000000000000000 ) ) ;
#20597 = EDGE_LOOP ( 'NONE', ( #9205, #759, #18391, #13217 ) ) ;
#20598 = EDGE_CURVE ( 'NONE', #21193, #18518, #24199, .T. ) ;
#20599 = DIRECTION ( 'NONE',  ( 1.000000000000000000, 0.000000000000000000, 0.000000000000000000 ) ) ;
#20600 = CARTESIAN_POINT ( 'NONE',  ( 95.09677333951634637, 69.00170213796093321, 32.49999999999999289 ) ) ;
#20601 = DIRECTION ( 'NONE',  ( -1.000000000000000000, 0.000000000000000000, 0.000000000000000000 ) ) ;
#20602 = VERTEX_POINT ( 'NONE', #29626 ) ;
#20603 = CARTESIAN_POINT ( 'NONE',  ( -20.00000337463123756, -69.28203230275522628, -5.000000000000000000 ) ) ;
#20604 = FACE_OUTER_BOUND ( 'NONE', #11257, .T. ) ;
#20605 = DIRECTION ( 'NONE',  ( 0.000000000000000000, 0.000000000000000000, 1.000000000000000000 ) ) ;
#20606 = ORIENTED_EDGE ( 'NONE', *, *, #23024, .F. ) ;
#20607 = DIRECTION ( 'NONE',  ( -0.000000000000000000, -0.000000000000000000, 1.000000000000000000 ) ) ;
#20608 = CIRCLE ( 'NONE', #18848, 2.000000000000001776 ) ;
#20609 = CARTESIAN_POINT ( 'NONE',  ( 69.99999662536841072, 51.96152422706640550, -9.999999999999998224 ) ) ;
#20610 = ORIENTED_EDGE ( 'NONE', *, *, #8068, .T. ) ;
#20611 = AXIS2_PLACEMENT_3D ( 'NONE', #14076, #188, #3196 ) ;
#20612 = ORIENTED_EDGE ( 'NONE', *, *, #32921, .F. ) ;
#20613 = CARTESIAN_POINT ( 'NONE',  ( 5.750000000000000000, 89.94802294027094547, 32.49999999999999289 ) ) ;
#20614 = EDGE_CURVE ( 'NONE', #22212, #25823, #17021, .T. ) ;
#20615 = CARTESIAN_POINT ( 'NONE',  ( 0.3000000000000016542, 6.123233995736766282E-16, -5.000000000000000000 ) ) ;
#20616 = CYLINDRICAL_SURFACE ( 'NONE', #7876, 2.000000000000001776 ) ;
#20617 = B_SPLINE_CURVE_WITH_KNOTS ( 'NONE', 3,
 ( #16820, #2387, #28607, #16625, #31235, #20168 ),
 .UNSPECIFIED., .F., .F.,
 ( 4, 2, 4 ),
 ( 0.002950759650825612868, 0.004429055062152258485, 0.005907350473478904102 ),
 .UNSPECIFIED. ) ;
#20618 = CARTESIAN_POINT ( 'NONE',  ( -35.00000337463116296, 60.62177826491077326, -9.999999999999998224 ) ) ;
#20619 = VERTEX_POINT ( 'NONE', #35299 ) ;
#20620 = CARTESIAN_POINT ( 'NONE',  ( -55.00000337463107059, 60.62177826491078747, -9.999999999999998224 ) ) ;
#20621 = DIRECTION ( 'NONE',  ( 0.000000000000000000, 0.000000000000000000, -1.000000000000000000 ) ) ;
#20622 = AXIS2_PLACEMENT_3D ( 'NONE', #27580, #36196, #7888 ) ;
#20623 = DIRECTION ( 'NONE',  ( -0.000000000000000000, -0.000000000000000000, 1.000000000000000000 ) ) ;
#20624 = VECTOR ( 'NONE', #30661, 1000.000000000000000 ) ;
#20625 = VERTEX_POINT ( 'NONE', #26091 ) ;
#20626 = DIRECTION ( 'NONE',  ( 0.000000000000000000, 0.000000000000000000, 1.000000000000000000 ) ) ;
#20627 = ORIENTED_EDGE ( 'NONE', *, *, #2368, .F. ) ;
#20628 = CARTESIAN_POINT ( 'NONE',  ( -87.00000337463093558, -8.660254037844422825, -9.999999999999998224 ) ) ;
#20629 = CARTESIAN_POINT ( 'NONE',  ( 0.000000000000000000, -55.00000000000000000, -5.000000000000000888 ) ) ;
#20630 = EDGE_CURVE ( 'NONE', #14854, #5583, #3214, .T. ) ;
#20631 = VECTOR ( 'NONE', #23198, 1000.000000000000000 ) ;
#20632 = DIRECTION ( 'NONE',  ( 0.000000000000000000, 0.000000000000000000, 1.000000000000000000 ) ) ;
#20633 = ORIENTED_EDGE ( 'NONE', *, *, #6588, .T. ) ;
#20634 = EDGE_CURVE ( 'NONE', #32102, #17303, #7447, .T. ) ;
#20635 = AXIS2_PLACEMENT_3D ( 'NONE', #4396, #30454, #27806 ) ;
#20636 = ORIENTED_EDGE ( 'NONE', *, *, #13716, .F. ) ;
#20637 = DIRECTION ( 'NONE',  ( -0.000000000000000000, -0.8660254037844419273, -0.4999999999999941158 ) ) ;
#20638 = CARTESIAN_POINT ( 'NONE',  ( -33.00000337463117006, -77.94228634059963667, -9.999999999999998224 ) ) ;
#20639 = DIRECTION ( 'NONE',  ( 0.000000000000000000, 0.000000000000000000, 1.000000000000000000 ) ) ;
#20640 = AXIS2_PLACEMENT_3D ( 'NONE', #11232, #22859, #19489 ) ;
#20641 = ORIENTED_EDGE ( 'NONE', *, *, #14936, .F. ) ;
#20642 = CARTESIAN_POINT ( 'NONE',  ( 3.000000000000000000, 0.000000000000000000, 0.000000000000000000 ) ) ;
#20643 = FACE_BOUND ( 'NONE', #20493, .T. ) ;
#20644 = EDGE_CURVE ( 'NONE', #21044, #2447, #13402, .T. ) ;
#20645 = DIRECTION ( 'NONE',  ( 0.000000000000000000, 0.000000000000000000, 1.000000000000000000 ) ) ;
#20646 = CARTESIAN_POINT ( 'NONE',  ( 4.166666666666665186, 3.367876570272815950, -3.818275046351160995 ) ) ;
#20647 = LINE ( 'NONE', #29286, #5164 ) ;
#20648 = EDGE_LOOP ( 'NONE', ( #23123, #19010 ) ) ;
#20649 = DIRECTION ( 'NONE',  ( 0.000000000000000000, 0.000000000000000000, 1.000000000000000000 ) ) ;
#20650 = CIRCLE ( 'NONE', #11077, 2.000000000000001776 ) ;
#20651 = VECTOR ( 'NONE', #18067, 999.9999999999998863 ) ;
#20652 = CARTESIAN_POINT ( 'NONE',  ( -33.00000337463116296, 60.62177826491077326, 12.50000000000000000 ) ) ;
#20653 = FILL_AREA_STYLE ('',( #21415 ) ) ;
#20654 = EDGE_LOOP ( 'NONE', ( #28075, #30711, #8427, #26008 ) ) ;
#20655 = CARTESIAN_POINT ( 'NONE',  ( -72.00000337463100664, -17.32050807568882078, 12.50000000000000000 ) ) ;
#20656 = DIRECTION ( 'NONE',  ( 0.000000000000000000, 0.000000000000000000, 1.000000000000000000 ) ) ;
#20657 = CARTESIAN_POINT ( 'NONE',  ( -83.00000337463092137, -25.98076211353322051, -5.000000000000000000 ) ) ;
#20658 = EDGE_CURVE ( 'NONE', #3324, #14961, #9595, .T. ) ;
#20659 = VERTEX_POINT ( 'NONE', #32450 ) ;
#20660 = EDGE_CURVE ( 'NONE', #3561, #31490, #6825, .T. ) ;
#20661 = ORIENTED_EDGE ( 'NONE', *, *, #8517, .T. ) ;
#20662 = ORIENTED_EDGE ( 'NONE', *, *, #11756, .T. ) ;
#20663 = ADVANCED_FACE ( 'NONE', ( #9954 ), #27747, .F. ) ;
#20664 = AXIS2_PLACEMENT_3D ( 'NONE', #5715, #19797, #2535 ) ;
#20665 = EDGE_CURVE ( 'NONE', #14875, #3002, #4720, .T. ) ;
#20666 = CYLINDRICAL_SURFACE ( 'NONE', #26490, 2.000000000000000000 ) ;
#20667 = DIRECTION ( 'NONE',  ( 0.000000000000000000, 0.000000000000000000, 1.000000000000000000 ) ) ;
#20668 = LINE ( 'NONE', #34936, #2861 ) ;
#20669 = ORIENTED_EDGE ( 'NONE', *, *, #23872, .T. ) ;
#20670 = EDGE_LOOP ( 'NONE', ( #25052, #28478, #11016, #5908 ) ) ;
#20671 = VERTEX_POINT ( 'NONE', #33190 ) ;
#20672 = AXIS2_PLACEMENT_3D ( 'NONE', #11087, #18806, #30222 ) ;
#20673 = MECHANICAL_DESIGN_GEOMETRIC_PRESENTATION_REPRESENTATION (  '', ( #19514 ), #31457 ) ;
#20674 = CARTESIAN_POINT ( 'NONE',  ( 62.99999662536839651, -60.62177826491080168, 12.50000000000000000 ) ) ;
#20675 = VERTEX_POINT ( 'NONE', #36201 ) ;
#20676 = DIRECTION ( 'NONE',  ( 0.000000000000000000, 0.000000000000000000, -1.000000000000000000 ) ) ;
#20677 = ORIENTED_EDGE ( 'NONE', *, *, #23295, .T. ) ;
#20678 = CYLINDRICAL_SURFACE ( 'NONE', #9369, 2.000000000000001776 ) ;
#20679 = ORIENTED_EDGE ( 'NONE', *, *, #22949, .F. ) ;
#20680 = AXIS2_PLACEMENT_3D ( 'NONE', #14352, #22967, #26148 ) ;
#20681 = ORIENTED_EDGE ( 'NONE', *, *, #455, .F. ) ;
#20682 = AXIS2_PLACEMENT_3D ( 'NONE', #3878, #26765, #1078 ) ;
#20683 = CARTESIAN_POINT ( 'NONE',  ( 56.67878100130369035, -27.78182860042797131, -49.86348611802629449 ) ) ;
#20684 = CARTESIAN_POINT ( 'NONE',  ( 2.744988726042924210, -4.188682711992893992, -0.5083873451168847701 ) ) ;
#20685 = CARTESIAN_POINT ( 'NONE',  ( -88.00000337463090716, -1.040834085586084257E-14, -9.999999999999998224 ) ) ;
#20686 = ORIENTED_EDGE ( 'NONE', *, *, #22714, .T. ) ;
#20687 = APPLICATION_CONTEXT ( 'automotive_design' ) ;
#20688 = VERTEX_POINT ( 'NONE', #13495 ) ;
#20689 = CARTESIAN_POINT ( 'NONE',  ( 145.0000000000000568, -5.056524707326808249E-13, 27.50000000000000000 ) ) ;
#20690 = ADVANCED_FACE ( 'NONE', ( #21756 ), #15767, .F. ) ;
#20691 = DIRECTION ( 'NONE',  ( 0.000000000000000000, 0.000000000000000000, 1.000000000000000000 ) ) ;
#20692 = CARTESIAN_POINT ( 'NONE',  ( -78.00000337463094979, 17.32050807568878525, -9.999999999999998224 ) ) ;
#20693 = AXIS2_PLACEMENT_3D ( 'NONE', #8864, #32284, #28904 ) ;
#20694 = ORIENTED_EDGE ( 'NONE', *, *, #26454, .F. ) ;
#20695 = DIRECTION ( 'NONE',  ( 0.000000000000000000, 0.000000000000000000, 1.000000000000000000 ) ) ;
#20696 = PLANE ( 'NONE',  #1811 ) ;
#20697 = VERTEX_POINT ( 'NONE', #24404 ) ;
#20698 = CARTESIAN_POINT ( 'NONE',  ( 34.99999662536853862, 77.94228634059959404, -9.999999999999998224 ) ) ;
#20699 = CIRCLE ( 'NONE', #27903, 2.000000000000000000 ) ;
#20700 = DIRECTION ( 'NONE',  ( -1.000000000000000000, 0.000000000000000000, 0.000000000000000000 ) ) ;
#20701 = DIRECTION ( 'NONE',  ( 1.000000000000000000, 0.000000000000000000, 0.000000000000000000 ) ) ;
#20702 = AXIS2_PLACEMENT_3D ( 'NONE', #12112, #29001, #17231 ) ;
#20703 = DIRECTION ( 'NONE',  ( -0.000000000000000000, -0.000000000000000000, 1.000000000000000000 ) ) ;
#20704 = DIRECTION ( 'NONE',  ( -0.000000000000000000, -0.000000000000000000, -1.000000000000000000 ) ) ;
#20705 = DIRECTION ( 'NONE',  ( 0.000000000000000000, 0.000000000000000000, -1.000000000000000000 ) ) ;
#20706 = ORIENTED_EDGE ( 'NONE', *, *, #28190, .T. ) ;
#20707 = DIRECTION ( 'NONE',  ( 1.000000000000000000, 0.000000000000000000, 0.000000000000000000 ) ) ;
#20708 = CIRCLE ( 'NONE', #12316, 33.00000000000001421 ) ;
#20709 = LINE ( 'NONE', #11714, #12279 ) ;
#20710 = FACE_OUTER_BOUND ( 'NONE', #27525, .T. ) ;
#20711 = ORIENTED_EDGE ( 'NONE', *, *, #32220, .F. ) ;
#20712 = CIRCLE ( 'NONE', #7557, 33.00000000000001421 ) ;
#20713 = ORIENTED_EDGE ( 'NONE', *, *, #9096, .F. ) ;
#20714 = VERTEX_POINT ( 'NONE', #7708 ) ;
#20715 = EDGE_CURVE ( 'NONE', #6695, #10470, #21397, .T. ) ;
#20716 = SURFACE_STYLE_USAGE ( .BOTH. , #23540 ) ;
#20717 = CARTESIAN_POINT ( 'NONE',  ( -43.19957991610399972, -47.04203867989563292, 12.49999999999999822 ) ) ;
#20718 = DIRECTION ( 'NONE',  ( 0.000000000000000000, 0.000000000000000000, 1.000000000000000000 ) ) ;
#20719 = CIRCLE ( 'NONE', #35701, 3.500000000000003109 ) ;
#20720 = DIRECTION ( 'NONE',  ( 0.000000000000000000, 0.000000000000000000, -1.000000000000000000 ) ) ;
#20721 = CIRCLE ( 'NONE', #33320, 6.000000000000005329 ) ;
#20722 = DIRECTION ( 'NONE',  ( 1.000000000000000000, 0.000000000000000000, 0.000000000000000000 ) ) ;
#20723 = ORIENTED_EDGE ( 'NONE', *, *, #35203, .F. ) ;
#20724 = LINE ( 'NONE', #6117, #11922 ) ;
#20725 = EDGE_LOOP ( 'NONE', ( #106, #6285 ) ) ;
#20726 = FACE_BOUND ( 'NONE', #34896, .T. ) ;
#20727 = CIRCLE ( 'NONE', #12940, 2.000000000000000000 ) ;
#20728 = CIRCLE ( 'NONE', #36907, 2.000000000000001776 ) ;
#20729 = AXIS2_PLACEMENT_3D ( 'NONE', #33555, #16120, #24916 ) ;
#20730 = CARTESIAN_POINT ( 'NONE',  ( -55.00000337463107059, 60.62177826491078747, -9.999999999999998224 ) ) ;
#20731 = FACE_BOUND ( 'NONE', #1649, .T. ) ;
#20732 = ORIENTED_EDGE ( 'NONE', *, *, #34386, .F. ) ;
#20733 = DIRECTION ( 'NONE',  ( 0.000000000000000000, 0.000000000000000000, 1.000000000000000000 ) ) ;
#20734 = EDGE_CURVE ( 'NONE', #5725, #393, #15202, .T. ) ;
#20735 = EDGE_CURVE ( 'NONE', #5193, #34910, #32629, .T. ) ;
#20736 = AXIS2_PLACEMENT_3D ( 'NONE', #33233, #35344, #9635 ) ;
#20737 = DIRECTION ( 'NONE',  ( 0.000000000000000000, 0.000000000000000000, -1.000000000000000000 ) ) ;
#20738 = CARTESIAN_POINT ( 'NONE',  ( 74.99999662536836809, 43.30127018922198801, -5.000000000000000000 ) ) ;
#20739 = DIRECTION ( 'NONE',  ( -1.000000000000000000, 0.000000000000000000, 0.000000000000000000 ) ) ;
#20740 = ORIENTED_EDGE ( 'NONE', *, *, #6843, .F. ) ;
#20741 = CARTESIAN_POINT ( 'NONE',  ( 51.99999662536848888, -51.96152422706640550, -9.999999999999998224 ) ) ;
#20742 = ADVANCED_FACE ( 'NONE', ( #12747 ), #1505, .F. ) ;
#20743 = DIRECTION ( 'NONE',  ( 1.000000000000000000, 0.000000000000000000, 0.000000000000000000 ) ) ;
#20744 = DIRECTION ( 'NONE',  ( -1.000000000000000000, 0.000000000000000000, 0.000000000000000000 ) ) ;
#20745 = VERTEX_POINT ( 'NONE', #2059 ) ;
#20746 = EDGE_CURVE ( 'NONE', #16300, #28642, #30189, .T. ) ;
#20747 = ORIENTED_EDGE ( 'NONE', *, *, #4159, .T. ) ;
#20748 = AXIS2_PLACEMENT_3D ( 'NONE', #13847, #25293, #2593 ) ;
#20749 = EDGE_LOOP ( 'NONE', ( #33881, #22071, #29232, #15363 ) ) ;
#20750 =( GEOMETRIC_REPRESENTATION_CONTEXT ( 3 ) GLOBAL_UNCERTAINTY_ASSIGNED_CONTEXT ( ( #10695 ) ) GLOBAL_UNIT_ASSIGNED_CONTEXT ( ( #4291, #27143, #33548 ) ) REPRESENTATION_CONTEXT ( 'NONE', 'WORKASPACE' ) );
#20751 = CARTESIAN_POINT ( 'NONE',  ( -56.52018970185234537, 35.83991598322119643, 12.49999999999999822 ) ) ;
#20752 = DIRECTION ( 'NONE',  ( 0.000000000000000000, 0.000000000000000000, 1.000000000000000000 ) ) ;
#20753 = AXIS2_PLACEMENT_3D ( 'NONE', #20460, #28538, #31880 ) ;
#20754 = VECTOR ( 'NONE', #36318, 1000.000000000000000 ) ;
#20755 = AXIS2_PLACEMENT_3D ( 'NONE', #32862, #10180, #18619 ) ;
#20756 = DIRECTION ( 'NONE',  ( -0.000000000000000000, -0.000000000000000000, 1.000000000000000000 ) ) ;
#20757 = CIRCLE ( 'NONE', #7576, 3.500000000000003109 ) ;
#20758 = VERTEX_POINT ( 'NONE', #12943 ) ;
#20759 = EDGE_CURVE ( 'NONE', #10548, #15799, #18405, .T. ) ;
#20760 = CARTESIAN_POINT ( 'NONE',  ( 36.99999662536855283, -60.62177826491080168, -9.999999999999998224 ) ) ;
#20761 = DIRECTION ( 'NONE',  ( 1.000000000000000000, 0.000000000000000000, 0.000000000000000000 ) ) ;
#20762 = CARTESIAN_POINT ( 'NONE',  ( 66.98486176412667703, -43.54685190870066691, 12.50000000000000000 ) ) ;
#20763 = VERTEX_POINT ( 'NONE', #15959 ) ;
#20764 = AXIS2_PLACEMENT_3D ( 'NONE', #9199, #20626, #17835 ) ;
#20765 = VERTEX_POINT ( 'NONE', #15592 ) ;
#20766 = DIRECTION ( 'NONE',  ( 1.000000000000000000, 0.000000000000000000, 0.000000000000000000 ) ) ;
#20767 = DIRECTION ( 'NONE',  ( 1.000000000000000000, 0.000000000000000000, 0.000000000000000000 ) ) ;
#20768 = ORIENTED_EDGE ( 'NONE', *, *, #34386, .T. ) ;
#20769 = CARTESIAN_POINT ( 'NONE',  ( -42.97377950131527058, 96.90768712682508124, -19.99999999999999645 ) ) ;
#20770 = ORIENTED_EDGE ( 'NONE', *, *, #23499, .F. ) ;
#20771 = CIRCLE ( 'NONE', #14289, 95.00000000000000000 ) ;
#20772 = AXIS2_PLACEMENT_3D ( 'NONE', #7270, #18705, #30861 ) ;
#20773 = AXIS2_PLACEMENT_3D ( 'NONE', #24775, #30942, #7899 ) ;
#20774 = TOROIDAL_SURFACE ( 'NONE', #4637, 6.532899837730827386, 0.5671001622691684840 ) ;
#20775 = FACE_BOUND ( 'NONE', #21161, .T. ) ;
#20776 = EDGE_LOOP ( 'NONE', ( #25701, #31673 ) ) ;
#20777 = ORIENTED_EDGE ( 'NONE', *, *, #1803, .F. ) ;
#20778 = EDGE_CURVE ( 'NONE', #14526, #9610, #23603, .T. ) ;
#20779 = LINE ( 'NONE', #7104, #23017 ) ;
#20780 = EDGE_LOOP ( 'NONE', ( #15993, #16883 ) ) ;
#20781 = FILL_AREA_STYLE_COLOUR ( '', #7044 ) ;
#20782 = VECTOR ( 'NONE', #1870, 1000.000000000000114 ) ;
#20783 = DIRECTION ( 'NONE',  ( 1.000000000000000000, 0.000000000000000000, 0.000000000000000000 ) ) ;
#20784 = AXIS2_PLACEMENT_3D ( 'NONE', #27452, #8126, #24467 ) ;
#20785 = CARTESIAN_POINT ( 'NONE',  ( 3.556264818047235821, 3.720292241887089624, -5.918341802876230240 ) ) ;
#20786 = FACE_OUTER_BOUND ( 'NONE', #9577, .T. ) ;
#20787 = VERTEX_POINT ( 'NONE', #33016 ) ;
#20788 = ORIENTED_EDGE ( 'NONE', *, *, #36220, .F. ) ;
#20789 = EDGE_CURVE ( 'NONE', #26833, #25364, #1328, .T. ) ;
#20790 = AXIS2_PLACEMENT_3D ( 'NONE', #24513, #27297, #35953 ) ;
#20791 = ORIENTED_EDGE ( 'NONE', *, *, #16787, .F. ) ;
#20792 = VERTEX_POINT ( 'NONE', #32838 ) ;
#20793 = EDGE_CURVE ( 'NONE', #24333, #25826, #35647, .T. ) ;
#20794 = ORIENTED_EDGE ( 'NONE', *, *, #2176, .T. ) ;
#20795 = CARTESIAN_POINT ( 'NONE',  ( -53.00000337463106348, 43.30127018922197379, 12.50000000000000000 ) ) ;
#20796 = AXIS2_PLACEMENT_3D ( 'NONE', #27515, #13426, #1441 ) ;
#20797 = FACE_OUTER_BOUND ( 'NONE', #15863, .T. ) ;
#20798 = ORIENTED_EDGE ( 'NONE', *, *, #7587, .T. ) ;
#20799 = AXIS2_PLACEMENT_3D ( 'NONE', #11914, #19989, #23374 ) ;
#20801 = CIRCLE ( 'NONE', #11227, 3.000000000000002665 ) ;
#20800 = DIRECTION ( 'NONE',  ( 0.000000000000000000, 0.000000000000000000, 1.000000000000000000 ) ) ;
#20802 = CARTESIAN_POINT ( 'NONE',  ( -70.00000337463100664, -17.32050807568882078, -9.999999999999998224 ) ) ;
#20803 = DIRECTION ( 'NONE',  ( 0.000000000000000000, 0.000000000000000000, 1.000000000000000000 ) ) ;
#20804 = ORIENTED_EDGE ( 'NONE', *, *, #5914, .F. ) ;
#20805 = CARTESIAN_POINT ( 'NONE',  ( -5.000000000000000888, -2.886751345948162406, -5.700000000000000178 ) ) ;
#20806 = AXIS2_PLACEMENT_3D ( 'NONE', #5025, #5581, #10849 ) ;
#20807 = DIRECTION ( 'NONE',  ( 0.000000000000000000, 0.000000000000000000, 1.000000000000000000 ) ) ;
#20808 = AXIS2_PLACEMENT_3D ( 'NONE', #30033, #30410, #24620 ) ;
#20809 = DIRECTION ( 'NONE',  ( 0.000000000000000000, 0.000000000000000000, 1.000000000000000000 ) ) ;
#20810 = VERTEX_POINT ( 'NONE', #30014 ) ;
#20811 = DIRECTION ( 'NONE',  ( 1.000000000000000000, 0.000000000000000000, 0.000000000000000000 ) ) ;
#20812 = DIRECTION ( 'NONE',  ( 1.000000000000000000, 0.000000000000000000, 0.000000000000000000 ) ) ;
#20813 = EDGE_LOOP ( 'NONE', ( #24549, #25831, #26491, #9008 ) ) ;
#20814 = AXIS2_PLACEMENT_3D ( 'NONE', #2988, #11762, #5794 ) ;
#20815 = VERTEX_POINT ( 'NONE', #1712 ) ;
#20816 = AXIS2_PLACEMENT_3D ( 'NONE', #25405, #34233, #7971 ) ;
#20817 = EDGE_CURVE ( 'NONE', #20354, #1224, #3828, .T. ) ;
#20818 = CARTESIAN_POINT ( 'NONE',  ( 42.97377950131527058, 96.90768712682506703, 27.49999999999999645 ) ) ;
#20819 = DIRECTION ( 'NONE',  ( 0.000000000000000000, 0.000000000000000000, 1.000000000000000000 ) ) ;
#20820 = DIRECTION ( 'NONE',  ( 0.000000000000000000, 0.000000000000000000, 1.000000000000000000 ) ) ;
#20821 = CARTESIAN_POINT ( 'NONE',  ( -4.999999999999999112, 0.2838785441256745923, -0.5080592402122393603 ) ) ;
#20822 = EDGE_LOOP ( 'NONE', ( #28645, #18150, #10899, #18371, #34588, #16560, #6943, #31517, #770, #28046, #2129, #2097 ) ) ;
#20823 = EDGE_CURVE ( 'NONE', #731, #17978, #1891, .T. ) ;
#20824 = DIRECTION ( 'NONE',  ( 1.000000000000000000, 0.000000000000000000, 0.000000000000000000 ) ) ;
#20825 = FACE_OUTER_BOUND ( 'NONE', #13003, .T. ) ;
#20826 = AXIS2_PLACEMENT_3D ( 'NONE', #6399, #20837, #32271 ) ;
#20827 = ORIENTED_EDGE ( 'NONE', *, *, #5215, .F. ) ;
#20828 = EDGE_CURVE ( 'NONE', #5579, #6874, #5649, .T. ) ;
#20829 = AXIS2_PLACEMENT_3D ( 'NONE', #2742, #25985, #6111 ) ;
#20830 = VECTOR ( 'NONE', #4532, 1000.000000000000000 ) ;
#20831 = CARTESIAN_POINT ( 'NONE',  ( -65.00000337463102085, 60.62177826491077326, -9.999999999999998224 ) ) ;
#20832 = VERTEX_POINT ( 'NONE', #19871 ) ;
#20833 = AXIS2_PLACEMENT_3D ( 'NONE', #17953, #9514, #32380 ) ;
#20834 = DIRECTION ( 'NONE',  ( -1.000000000000000000, 0.000000000000000000, 0.000000000000000000 ) ) ;
#20835 = CARTESIAN_POINT ( 'NONE',  ( 67.99999662536838230, -17.32050807568879947, -9.999999999999998224 ) ) ;
#20836 = AXIS2_PLACEMENT_3D ( 'NONE', #13893, #5294, #25886 ) ;
#20837 = DIRECTION ( 'NONE',  ( 0.000000000000000000, 0.000000000000000000, 1.000000000000000000 ) ) ;
#20838 = ORIENTED_EDGE ( 'NONE', *, *, #22016, .F. ) ;
#20839 = ORIENTED_EDGE ( 'NONE', *, *, #19027, .F. ) ;
#20840 = DIRECTION ( 'NONE',  ( -0.8660254037844381525, 0.5000000000000009992, 0.000000000000000000 ) ) ;
#20841 = CARTESIAN_POINT ( 'NONE',  ( 35.19434990244975126, -52.39915983220758022, -49.22241343995298024 ) ) ;
#20842 = AXIS2_PLACEMENT_3D ( 'NONE', #36734, #25478, #31650 ) ;
#20843 = EDGE_CURVE ( 'NONE', #17038, #21182, #19413, .T. ) ;
#20844 = ORIENTED_EDGE ( 'NONE', *, *, #8447, .T. ) ;
#20845 = DIRECTION ( 'NONE',  ( 0.000000000000000000, 0.000000000000000000, 1.000000000000000000 ) ) ;
#20846 = DIRECTION ( 'NONE',  ( 0.000000000000000000, 0.000000000000000000, 1.000000000000000000 ) ) ;
#20847 = DIRECTION ( 'NONE',  ( 1.000000000000000000, 0.000000000000000000, 0.000000000000000000 ) ) ;
#20848 = DIRECTION ( 'NONE',  ( -1.000000000000000000, 0.000000000000000000, 0.000000000000000000 ) ) ;
#20849 = AXIS2_PLACEMENT_3D ( 'NONE', #25456, #25838, #36896 ) ;
#20850 = DIRECTION ( 'NONE',  ( -0.7071067811865539010, -0.7071067811865411334, 0.000000000000000000 ) ) ;
#20851 = ORIENTED_EDGE ( 'NONE', *, *, #12302, .T. ) ;
#20852 = CARTESIAN_POINT ( 'NONE',  ( -77.00000337463097821, 43.30127018922197379, -9.999999999999998224 ) ) ;
#20853 = PRODUCT_DEFINITION_SHAPE ( 'NONE', 'NONE',  #37108 ) ;
#20854 = CYLINDRICAL_SURFACE ( 'NONE', #1212, 2.000000000000001776 ) ;
#20855 = VECTOR ( 'NONE', #3358, 999.9999999999998863 ) ;
#20856 = CARTESIAN_POINT ( 'NONE',  ( -73.00000337463097821, 25.98076211353318854, -9.999999999999998224 ) ) ;
#20857 = ORIENTED_EDGE ( 'NONE', *, *, #31569, .F. ) ;
#20858 = FACE_OUTER_BOUND ( 'NONE', #922, .T. ) ;
#20859 = CIRCLE ( 'NONE', #14869, 19.53925848833874213 ) ;
#20860 = DIRECTION ( 'NONE',  ( 1.000000000000000000, 0.000000000000000000, 0.000000000000000000 ) ) ;
#20861 = CARTESIAN_POINT ( 'NONE',  ( 31.99999662536857770, -69.28203230275519786, -9.999999999999998224 ) ) ;
#20862 = AXIS2_PLACEMENT_3D ( 'NONE', #10623, #2174, #13810 ) ;
#20863 = ORIENTED_EDGE ( 'NONE', *, *, #35904, .F. ) ;
#20864 = ORIENTED_EDGE ( 'NONE', *, *, #5534, .T. ) ;
#20865 = ADVANCED_FACE ( 'NONE', ( #13698 ), #33950, .T. ) ;
#20866 = EDGE_LOOP ( 'NONE', ( #3210, #33841, #32751, #35382 ) ) ;
#20867 = VECTOR ( 'NONE', #8238, 1000.000000000000000 ) ;
#20868 = DIRECTION ( 'NONE',  ( 0.000000000000000000, 0.000000000000000000, 1.000000000000000000 ) ) ;
#20869 = FACE_OUTER_BOUND ( 'NONE', #28845, .T. ) ;
#20870 = EDGE_CURVE ( 'NONE', #30055, #6269, #15224, .T. ) ;
#20871 = CARTESIAN_POINT ( 'NONE',  ( -1.324703144935793775, -5.008684974571242066, -0.8655517945778401501 ) ) ;
#20872 = VERTEX_POINT ( 'NONE', #10877 ) ;
#20873 = ORIENTED_EDGE ( 'NONE', *, *, #19034, .T. ) ;
#20874 = ORIENTED_EDGE ( 'NONE', *, *, #35635, .F. ) ;
#20875 = AXIS2_PLACEMENT_3D ( 'NONE', #29816, #3588, #12565 ) ;
#20876 = ADVANCED_FACE ( 'NONE', ( #22694 ), #5068, .T. ) ;
#20877 = DIRECTION ( 'NONE',  ( -0.000000000000000000, -0.000000000000000000, -1.000000000000000000 ) ) ;
#20878 = VERTEX_POINT ( 'NONE', #22318 ) ;
#20879 = CARTESIAN_POINT ( 'NONE',  ( 31.99999662536857770, -69.28203230275519786, -5.000000000000000000 ) ) ;
#20881 = EDGE_CURVE ( 'NONE', #36272, #20246, #17253, .T. ) ;
#20880 = ORIENTED_EDGE ( 'NONE', *, *, #1217, .F. ) ;
#20882 = CARTESIAN_POINT ( 'NONE',  ( -57.00000337463107059, 60.62177826491078747, -9.999999999999998224 ) ) ;
#20883 = ORIENTED_EDGE ( 'NONE', *, *, #25021, .F. ) ;
#20884 = EDGE_CURVE ( 'NONE', #31631, #31383, #20589, .T. ) ;
#20885 = EDGE_LOOP ( 'NONE', ( #21149, #36757, #31946, #23672 ) ) ;
#20886 = DIRECTION ( 'NONE',  ( -1.000000000000000000, 0.000000000000000000, 0.000000000000000000 ) ) ;
#20887 = CARTESIAN_POINT ( 'NONE',  ( 79.99999662536832545, -17.32050807568879591, -5.000000000000000000 ) ) ;
#20888 = AXIS2_PLACEMENT_3D ( 'NONE', #18156, #12897, #24554 ) ;
#20889 = CARTESIAN_POINT ( 'NONE',  ( 52.99999662536844625, 60.62177826491077326, -5.000000000000000000 ) ) ;
#20890 = EDGE_LOOP ( 'NONE', ( #16486, #34981, #30194, #31715 ) ) ;
#20891 = ORIENTED_EDGE ( 'NONE', *, *, #34466, .F. ) ;
#20892 = CARTESIAN_POINT ( 'NONE',  ( 67.99999662536836809, -34.64101615137759183, -9.999999999999998224 ) ) ;
#20893 = AXIS2_PLACEMENT_3D ( 'NONE', #21246, #15453, #9810 ) ;
#20894 = DIRECTION ( 'NONE',  ( 0.000000000000000000, 0.000000000000000000, -1.000000000000000000 ) ) ;
#20895 = ADVANCED_FACE ( 'NONE', ( #11051 ), #19505, .T. ) ;
#20896 = CARTESIAN_POINT ( 'NONE',  ( -20.00000337463123756, -86.60254037844400443, -9.999999999999998224 ) ) ;
#20897 = ADVANCED_FACE ( 'NONE', ( #5270 ), #10441, .T. ) ;
#20898 = DIRECTION ( 'NONE',  ( -1.000000000000000000, 0.000000000000000000, 0.000000000000000000 ) ) ;
#20899 = ADVANCED_FACE ( 'NONE', ( #22146 ), #22496, .F. ) ;
#20900 = ORIENTED_EDGE ( 'NONE', *, *, #5191, .F. ) ;
#20901 = LINE ( 'NONE', #11890, #35114 ) ;
#20902 = CARTESIAN_POINT ( 'NONE',  ( -65.00000000000000000, 0.000000000000000000, 5.000000000000000000 ) ) ;
#20903 = EDGE_CURVE ( 'NONE', #6546, #21552, #3876, .T. ) ;
#20904 = AXIS2_PLACEMENT_3D ( 'NONE', #29116, #3451, #26323 ) ;
#20905 = ORIENTED_EDGE ( 'NONE', *, *, #21513, .F. ) ;
#20906 = DIRECTION ( 'NONE',  ( 0.000000000000000000, 0.000000000000000000, 1.000000000000000000 ) ) ;
#20907 = EDGE_CURVE ( 'NONE', #1764, #11378, #25318, .T. ) ;
#20908 = DIRECTION ( 'NONE',  ( -1.000000000000000000, 0.000000000000000000, 0.000000000000000000 ) ) ;
#20909 = FACE_OUTER_BOUND ( 'NONE', #32872, .T. ) ;
#20910 = VECTOR ( 'NONE', #27377, 1000.000000000000000 ) ;
#20911 = CARTESIAN_POINT ( 'NONE',  ( 84.99999662536831124, -8.660254037844397956, -5.000000000000000000 ) ) ;
#20912 = CIRCLE ( 'NONE', #4756, 2.000000000000001776 ) ;
#20913 = FACE_OUTER_BOUND ( 'NONE', #9433, .T. ) ;
#20914 = FACE_OUTER_BOUND ( 'NONE', #11975, .T. ) ;
#20915 = CIRCLE ( 'NONE', #4758, 3.000000000000007105 ) ;
#20916 = ORIENTED_EDGE ( 'NONE', *, *, #28258, .F. ) ;
#20917 = CARTESIAN_POINT ( 'NONE',  ( -58.00000337463104216, 34.64101615137757051, -9.999999999999998224 ) ) ;
#20918 = CARTESIAN_POINT ( 'NONE',  ( 1.738710530748193150, 5.045296470309976300, -4.085927688751835873 ) ) ;
#20919 = CARTESIAN_POINT ( 'NONE',  ( -67.00000337463102085, 60.62177826491077326, -5.000000000000000000 ) ) ;
#20920 = EDGE_LOOP ( 'NONE', ( #23372, #34544 ) ) ;
#20921 = VERTEX_POINT ( 'NONE', #5452 ) ;
#20922 = ORIENTED_EDGE ( 'NONE', *, *, #29399, .F. ) ;
#20923 = CIRCLE ( 'NONE', #28701, 2.000000000000001776 ) ;
#20924 = CARTESIAN_POINT ( 'NONE',  ( -65.00000337463104927, -43.30127018922202353, -9.999999999999998224 ) ) ;
#20925 = CARTESIAN_POINT ( 'NONE',  ( 9.999996625368655856, -69.28203230275519786, -9.999999999999998224 ) ) ;
#20926 = AXIS2_PLACEMENT_3D ( 'NONE', #26418, #9347, #15158 ) ;
#20927 = DIRECTION ( 'NONE',  ( 1.000000000000000000, -3.846960960290410782E-15, 0.000000000000000000 ) ) ;
#20928 = CARTESIAN_POINT ( 'NONE',  ( 0.000000000000000000, 0.000000000000000000, 12.49999999999999822 ) ) ;
#20929 = DIRECTION ( 'NONE',  ( 1.000000000000000000, 0.000000000000000000, 0.000000000000000000 ) ) ;
#20930 = ORIENTED_EDGE ( 'NONE', *, *, #30865, .F. ) ;
#20931 =( REPRESENTATION_RELATIONSHIP ('NONE','NONE', #15268, #22738 ) REPRESENTATION_RELATIONSHIP_WITH_TRANSFORMATION ( #2162 )SHAPE_REPRESENTATION_RELATIONSHIP( ) );
#20932 = DIRECTION ( 'NONE',  ( -1.000000000000000000, 0.000000000000000000, 0.000000000000000000 ) ) ;
#20933 = EDGE_LOOP ( 'NONE', ( #6136, #17196 ) ) ;
#20934 = FACE_BOUND ( 'NONE', #11132, .T. ) ;
#20935 = AXIS2_PLACEMENT_3D ( 'NONE', #10055, #27099, #7608 ) ;
#20936 = DIRECTION ( 'NONE',  ( 1.000000000000000000, 0.000000000000000000, -0.000000000000000000 ) ) ;
#20937 = CARTESIAN_POINT ( 'NONE',  ( -18.00000337463124467, 69.28203230275516944, -5.000000000000000000 ) ) ;
#20938 = VERTEX_POINT ( 'NONE', #16878 ) ;
#20939 = PLANE ( 'NONE',  #15270 ) ;
#20940 = AXIS2_PLACEMENT_3D ( 'NONE', #16518, #21961, #21767 ) ;
#20941 = APPLICATION_PROTOCOL_DEFINITION ( 'draft international standard', 'automotive_design', 1998, #17321 ) ;
#20942 = CARTESIAN_POINT ( 'NONE',  ( -13.89091430021420237, -62.33939050065180254, 12.49999999999999822 ) ) ;
#20943 = CIRCLE ( 'NONE', #13778, 3.499999999999989342 ) ;
#20944 = LINE ( 'NONE', #26937, #27533 ) ;
#20945 = CARTESIAN_POINT ( 'NONE',  ( 0.000000000000000000, 0.000000000000000000, 2.266666666666999674 ) ) ;
#20946 = ADVANCED_FACE ( 'NONE', ( #14048 ), #25497, .F. ) ;
#20947 = EDGE_LOOP ( 'NONE', ( #28767, #2584 ) ) ;
#20948 = LINE ( 'NONE', #23563, #30383 ) ;
#20949 = CIRCLE ( 'NONE', #29315, 3.000000000000006217 ) ;
#20950 = CARTESIAN_POINT ( 'NONE',  ( 44.99999662536849598, 60.62177826491077326, -5.000000000000000000 ) ) ;
#20951 = DIRECTION ( 'NONE',  ( 1.000000000000000000, 0.000000000000000000, 0.000000000000000000 ) ) ;
#20952 = EDGE_LOOP ( 'NONE', ( #19434, #1292 ) ) ;
#20953 = EDGE_LOOP ( 'NONE', ( #22959, #35037 ) ) ;
#20954 = VERTEX_POINT ( 'NONE', #2817 ) ;
#20955 = DIRECTION ( 'NONE',  ( 0.000000000000000000, 0.000000000000000000, 1.000000000000000000 ) ) ;
#20956 = CARTESIAN_POINT ( 'NONE',  ( -70.00000337463099243, 51.96152422706637708, -9.999999999999998224 ) ) ;
#20957 = FACE_OUTER_BOUND ( 'NONE', #30170, .T. ) ;
#20958 = AXIS2_PLACEMENT_3D ( 'NONE', #10935, #2333, #16772 ) ;
#20959 = CARTESIAN_POINT ( 'NONE',  ( -23.49187026334539041, 103.5527527874234863, 27.49999400000000094 ) ) ;
#20960 = DIRECTION ( 'NONE',  ( -1.000000000000000000, 0.000000000000000000, 0.000000000000000000 ) ) ;
#20961 = AXIS2_PLACEMENT_3D ( 'NONE', #36366, #25122, #25290 ) ;
#20962 = DIRECTION ( 'NONE',  ( 1.000000000000000000, 0.000000000000000000, 0.000000000000000000 ) ) ;
#20963 = EDGE_CURVE ( 'NONE', #14395, #3448, #21844, .T. ) ;
#20964 = ORIENTED_EDGE ( 'NONE', *, *, #31020, .T. ) ;
#20965 = ORIENTED_EDGE ( 'NONE', *, *, #4492, .T. ) ;
#20966 = DIRECTION ( 'NONE',  ( 0.000000000000000000, 0.000000000000000000, 1.000000000000000000 ) ) ;
#20967 = VECTOR ( 'NONE', #8540, 1000.000000000000000 ) ;
#20968 = DIRECTION ( 'NONE',  ( 0.000000000000000000, 0.000000000000000000, -1.000000000000000000 ) ) ;
#20969 = ORIENTED_EDGE ( 'NONE', *, *, #22232, .F. ) ;
#20970 = CARTESIAN_POINT ( 'NONE',  ( -4.296971609540129577, -3.292644976428437342, -4.096693167836007454 ) ) ;
#20971 = ORIENTED_EDGE ( 'NONE', *, *, #12053, .F. ) ;
#20972 = AXIS2_PLACEMENT_3D ( 'NONE', #6510, #689, #11935 ) ;
#20973 = FACE_BOUND ( 'NONE', #12820, .T. ) ;
#20974 = ORIENTED_EDGE ( 'NONE', *, *, #36343, .T. ) ;
#20975 = ORIENTED_EDGE ( 'NONE', *, *, #21903, .F. ) ;
#20976 = VECTOR ( 'NONE', #23669, 1000.000000000000000 ) ;
#20977 = CARTESIAN_POINT ( 'NONE',  ( -48.00000337463109190, 69.28203230275518365, -9.999999999999998224 ) ) ;
#20978 = VERTEX_POINT ( 'NONE', #11428 ) ;
#20979 = FACE_OUTER_BOUND ( 'NONE', #10058, .T. ) ;
#20980 = DIRECTION ( 'NONE',  ( -1.000000000000000000, -1.798972493605576793E-15, 0.000000000000000000 ) ) ;
#20981 = CARTESIAN_POINT ( 'NONE',  ( 76.99999662536835388, -43.30127018922199511, -9.999999999999998224 ) ) ;
#20982 = CIRCLE ( 'NONE', #27579, 3.000000000000002665 ) ;
#20983 = ADVANCED_FACE ( 'NONE', ( #34310 ), #22873, .F. ) ;
#20984 = EDGE_LOOP ( 'NONE', ( #36874, #19855, #889, #8026 ) ) ;
#20985 = ORIENTED_EDGE ( 'NONE', *, *, #16995, .T. ) ;
#20986 = AXIS2_PLACEMENT_3D ( 'NONE', #30712, #10294, #16471 ) ;
#20987 = ORIENTED_EDGE ( 'NONE', *, *, #28216, .T. ) ;
#20988 = ORIENTED_EDGE ( 'NONE', *, *, #27397, .F. ) ;
#20989 = ORIENTED_EDGE ( 'NONE', *, *, #13290, .F. ) ;
#20990 = DIRECTION ( 'NONE',  ( -1.000000000000000000, 0.000000000000000000, 0.000000000000000000 ) ) ;
#20991 = CARTESIAN_POINT ( 'NONE',  ( 44.99999662536851019, -60.62177826491080168, 17.49999999999999645 ) ) ;
#20992 = EDGE_LOOP ( 'NONE', ( #26313, #34070 ) ) ;
#20993 = DIRECTION ( 'NONE',  ( 0.000000000000000000, 0.000000000000000000, -1.000000000000000000 ) ) ;
#20994 = CARTESIAN_POINT ( 'NONE',  ( 102.2320902944790788, 32.43306441797120243, 32.50000000000000000 ) ) ;
#20995 = CYLINDRICAL_SURFACE ( 'NONE', #24951, 2.000000000000001776 ) ;
#20996 = VERTEX_POINT ( 'NONE', #15157 ) ;
#20997 = DIRECTION ( 'NONE',  ( 0.000000000000000000, 0.000000000000000000, 1.000000000000000000 ) ) ;
#20998 = FACE_OUTER_BOUND ( 'NONE', #22213, .T. ) ;
#20999 = EDGE_CURVE ( 'NONE', #13946, #4610, #11591, .T. ) ;
#21000 = CARTESIAN_POINT ( 'NONE',  ( 68.19434990244977257, -52.39915983220758022, 12.49999999999999822 ) ) ;
#21001 = ORIENTED_EDGE ( 'NONE', *, *, #19962, .T. ) ;
#21002 = CARTESIAN_POINT ( 'NONE',  ( 124.4080600076931375, 12.15049814296589226, 32.50002500000000083 ) ) ;
#21003 = CYLINDRICAL_SURFACE ( 'NONE', #24394, 2.000000000000001776 ) ;
#21004 = EDGE_CURVE ( 'NONE', #7750, #35055, #24829, .T. ) ;
#21005 = ORIENTED_EDGE ( 'NONE', *, *, #28591, .F. ) ;
#21006 = ORIENTED_EDGE ( 'NONE', *, *, #27853, .T. ) ;
#21007 = CARTESIAN_POINT ( 'NONE',  ( -43.00000337463111322, 60.62177826491077326, 12.50000000000000000 ) ) ;
#21008 = CARTESIAN_POINT ( 'NONE',  ( -72.00000337463100664, 51.96152422706637708, -5.000000000000000000 ) ) ;
#21009 = AXIS2_PLACEMENT_3D ( 'NONE', #13849, #8236, #33367 ) ;
#21010 = CARTESIAN_POINT ( 'NONE',  ( 74.99999662536836809, 8.660254037844394404, -9.999999999999998224 ) ) ;
#21011 = CARTESIAN_POINT ( 'NONE',  ( -5.000000000000000000, 1.101175676120956348, -0.7375066809288767233 ) ) ;
#21012 = EDGE_CURVE ( 'NONE', #26378, #13656, #20243, .T. ) ;
#21013 = ORIENTED_EDGE ( 'NONE', *, *, #35465, .F. ) ;
#21014 = CYLINDRICAL_SURFACE ( 'NONE', #15354, 2.000000000000001776 ) ;
#21015 = DIRECTION ( 'NONE',  ( -0.000000000000000000, 0.000000000000000000, 1.000000000000000000 ) ) ;
#21016 = ADVANCED_FACE ( 'NONE', ( #3355 ), #14793, .T. ) ;
#21017 = VERTEX_POINT ( 'NONE', #903 ) ;
#21018 = CARTESIAN_POINT ( 'NONE',  ( -58.00000337463108480, -51.96152422706641971, 17.49999999999999645 ) ) ;
#21019 = ORIENTED_EDGE ( 'NONE', *, *, #9178, .F. ) ;
#21020 = CARTESIAN_POINT ( 'NONE',  ( 35.19434990244975126, -52.39915983220758022, 12.49999999999999822 ) ) ;
#21021 = DIRECTION ( 'NONE',  ( 0.000000000000000000, 0.000000000000000000, -1.000000000000000000 ) ) ;
#21022 = DIRECTION ( 'NONE',  ( -1.000000000000000000, 0.000000000000000000, 0.000000000000000000 ) ) ;
#21023 = ORIENTED_EDGE ( 'NONE', *, *, #34118, .T. ) ;
#21024 = ORIENTED_EDGE ( 'NONE', *, *, #16368, .T. ) ;
#21025 = AXIS2_PLACEMENT_3D ( 'NONE', #18941, #1697, #4504 ) ;
#21026 = DIRECTION ( 'NONE',  ( -0.000000000000000000, -0.000000000000000000, 1.000000000000000000 ) ) ;
#21027 = EDGE_CURVE ( 'NONE', #35994, #6252, #31981, .T. ) ;
#21028 = EDGE_LOOP ( 'NONE', ( #22715, #29773, #4348, #33486, #24217 ) ) ;
#21029 = DIRECTION ( 'NONE',  ( -0.000000000000000000, -0.000000000000000000, -1.000000000000000000 ) ) ;
#21030 = FACE_BOUND ( 'NONE', #7747, .T. ) ;
#21031 = DIRECTION ( 'NONE',  ( 0.000000000000000000, 0.000000000000000000, 1.000000000000000000 ) ) ;
#21032 = CARTESIAN_POINT ( 'NONE',  ( 82.99999662536832545, 8.660254037844394404, 17.49999999999999645 ) ) ;
#21033 = DIRECTION ( 'NONE',  ( 0.000000000000000000, 0.000000000000000000, 1.000000000000000000 ) ) ;
#21034 = ORIENTED_EDGE ( 'NONE', *, *, #31276, .F. ) ;
#21035 = LINE ( 'NONE', #20852, #35056 ) ;
#21036 = ADVANCED_FACE ( 'NONE', ( #20979 ), #6162, .F. ) ;
#21037 = DIRECTION ( 'NONE',  ( 0.000000000000000000, 0.000000000000000000, 1.000000000000000000 ) ) ;
#21038 = EDGE_CURVE ( 'NONE', #35651, #12099, #9547, .T. ) ;
#21039 = CARTESIAN_POINT ( 'NONE',  ( 9.999996625368655856, -69.28203230275519786, 12.50000000000000000 ) ) ;
#21040 = ORIENTED_EDGE ( 'NONE', *, *, #21621, .F. ) ;
#21041 = DIRECTION ( 'NONE',  ( -1.000000000000000000, 0.000000000000000000, 0.000000000000000000 ) ) ;
#21042 = DIRECTION ( 'NONE',  ( 0.000000000000000000, 0.000000000000000000, -1.000000000000000000 ) ) ;
#21043 = DIRECTION ( 'NONE',  ( -1.000000000000000000, 0.000000000000000000, 0.000000000000000000 ) ) ;
#21044 = VERTEX_POINT ( 'NONE', #31667 ) ;
#21045 = ORIENTED_EDGE ( 'NONE', *, *, #9196, .T. ) ;
#21046 = CIRCLE ( 'NONE', #24055, 2.000000000000001776 ) ;
#21047 = DIRECTION ( 'NONE',  ( 1.000000000000000000, 0.000000000000000000, 0.000000000000000000 ) ) ;
#21048 = DIRECTION ( 'NONE',  ( 1.000000000000000000, 0.000000000000000000, 0.000000000000000000 ) ) ;
#21049 = CARTESIAN_POINT ( 'NONE',  ( 0.000000000000000000, -2.935248768560059229, 3.469446951953614189E-15 ) ) ;
#21050 = ORIENTED_EDGE ( 'NONE', *, *, #13967, .T. ) ;
#21051 = CIRCLE ( 'NONE', #16281, 33.00000000000001421 ) ;
#21052 = ORIENTED_EDGE ( 'NONE', *, *, #31417, .T. ) ;
#21053 = ORIENTED_EDGE ( 'NONE', *, *, #25592, .T. ) ;
#21054 = DIRECTION ( 'NONE',  ( 0.000000000000000000, 0.000000000000000000, 1.000000000000000000 ) ) ;
#21055 = ADVANCED_FACE ( 'NONE', ( #9346 ), #12324, .F. ) ;
#21056 = ORIENTED_EDGE ( 'NONE', *, *, #21119, .F. ) ;
#21057 = ORIENTED_EDGE ( 'NONE', *, *, #19124, .F. ) ;
#21058 = DIRECTION ( 'NONE',  ( -0.000000000000000000, -0.000000000000000000, 1.000000000000000000 ) ) ;
#21059 = VERTEX_POINT ( 'NONE', #161 ) ;
#21060 = ORIENTED_EDGE ( 'NONE', *, *, #9445, .F. ) ;
#21061 = SHAPE_REPRESENTATION_RELATIONSHIP ( 'NONE' , 'NONE' ,  #26771, #20178 ) ;
#21062 = PLANE ( 'NONE',  #5843 ) ;
#21063 = LINE ( 'NONE', #3811, #8094 ) ;
#21064 = ORIENTED_EDGE ( 'NONE', *, *, #11420, .T. ) ;
#21065 = ORIENTED_EDGE ( 'NONE', *, *, #18233, .F. ) ;
#21066 = DIRECTION ( 'NONE',  ( 1.000000000000000000, 0.000000000000000000, 0.000000000000000000 ) ) ;
#21067 = DIRECTION ( 'NONE',  ( 0.000000000000000000, 0.000000000000000000, 1.000000000000000000 ) ) ;
#21068 = DIRECTION ( 'NONE',  ( 1.000000000000000000, 0.000000000000000000, 0.000000000000000000 ) ) ;
#21069 = CARTESIAN_POINT ( 'NONE',  ( 76.99999662536836809, 8.660254037844394404, 17.49999999999999645 ) ) ;
#21070 = EDGE_CURVE ( 'NONE', #14210, #21598, #5678, .T. ) ;
#21071 = ORIENTED_EDGE ( 'NONE', *, *, #29083, .T. ) ;
#21072 = CARTESIAN_POINT ( 'NONE',  ( -83.49774789488644444, 24.66044833507834610, -5.000000000000000000 ) ) ;
#21073 = DIRECTION ( 'NONE',  ( 0.000000000000000000, -0.8660254037844418162, -0.4999999999999945044 ) ) ;
#21074 = CIRCLE ( 'NONE', #13900, 2.000000000000001776 ) ;
#21075 = ORIENTED_EDGE ( 'NONE', *, *, #16868, .T. ) ;
#21076 = EDGE_CURVE ( 'NONE', #24584, #10304, #31415, .T. ) ;
#21077 = DIRECTION ( 'NONE',  ( -1.000000000000000000, -8.737866397512800437E-15, 0.000000000000000000 ) ) ;
#21078 = FACE_OUTER_BOUND ( 'NONE', #34358, .T. ) ;
#21079 = DIRECTION ( 'NONE',  ( 0.000000000000000000, 0.000000000000000000, 1.000000000000000000 ) ) ;
#21080 = DIRECTION ( 'NONE',  ( 0.000000000000000000, 0.000000000000000000, 1.000000000000000000 ) ) ;
#21081 = ADVANCED_FACE ( 'NONE', ( #11970, #9152 ), #25867, .T. ) ;
#21082 = CARTESIAN_POINT ( 'NONE',  ( 39.99999662536853151, 69.28203230275518365, -9.999999999999998224 ) ) ;
#21083 = EDGE_CURVE ( 'NONE', #9125, #12353, #9253, .T. ) ;
#21084 = CARTESIAN_POINT ( 'NONE',  ( -3.000000000000000888, 3.673940397442060854E-16, -25.03750572909317285 ) ) ;
#21085 = ORIENTED_EDGE ( 'NONE', *, *, #17225, .F. ) ;
#21086 = CARTESIAN_POINT ( 'NONE',  ( 66.99999662536839651, -43.30127018922199511, -5.000000000000000000 ) ) ;
#21087 = EDGE_CURVE ( 'NONE', #5560, #32910, #9847, .T. ) ;
#21088 = CARTESIAN_POINT ( 'NONE',  ( 4.379424050594064255, 3.527728022193126645, -4.190801088233093274 ) ) ;
#21089 = DIRECTION ( 'NONE',  ( -1.000000000000000000, 1.082992363797667670E-14, 0.000000000000000000 ) ) ;
#21090 = EDGE_CURVE ( 'NONE', #27516, #2053, #35615, .T. ) ;
#21091 = ORIENTED_EDGE ( 'NONE', *, *, #4326, .T. ) ;
#21092 = ORIENTED_EDGE ( 'NONE', *, *, #28214, .T. ) ;
#21093 = ORIENTED_EDGE ( 'NONE', *, *, #28684, .T. ) ;
#21094 = DIRECTION ( 'NONE',  ( 0.000000000000000000, 0.000000000000000000, -1.000000000000000000 ) ) ;
#21095 = CARTESIAN_POINT ( 'NONE',  ( 36.99999662536855283, 60.62177826491078747, -9.999999999999998224 ) ) ;
#21096 = LINE ( 'NONE', #12259, #310 ) ;
#21097 = ADVANCED_FACE ( 'NONE', ( #29022 ), #6346, .F. ) ;
#21098 = EDGE_CURVE ( 'NONE', #10841, #31248, #12229, .T. ) ;
#21099 = CARTESIAN_POINT ( 'NONE',  ( -5.000000000000000000, 0.000000000000000000, -6.000000000000000000 ) ) ;
#21100 = ADVANCED_FACE ( 'NONE', ( #23988 ), #21343, .F. ) ;
#21101 = CIRCLE ( 'NONE', #27681, 95.00000000000001421 ) ;
#21102 = CARTESIAN_POINT ( 'NONE',  ( 9.999996625368655856, -86.60254037844400443, 12.50000000000000000 ) ) ;
#21103 = ORIENTED_EDGE ( 'NONE', *, *, #28855, .T. ) ;
#21104 = DIRECTION ( 'NONE',  ( 0.000000000000000000, 0.000000000000000000, 1.000000000000000000 ) ) ;
#21105 = ORIENTED_EDGE ( 'NONE', *, *, #2085, .F. ) ;
#21106 = FACE_BOUND ( 'NONE', #7752, .T. ) ;
#21107 = DIRECTION ( 'NONE',  ( 0.000000000000000000, 0.000000000000000000, 1.000000000000000000 ) ) ;
#21108 = DIRECTION ( 'NONE',  ( 0.000000000000000000, 0.000000000000000000, 1.000000000000000000 ) ) ;
#21109 = CARTESIAN_POINT ( 'NONE',  ( 49.99999662536848177, -51.96152422706640550, 12.50000000000000000 ) ) ;
#21110 = ORIENTED_EDGE ( 'NONE', *, *, #6528, .T. ) ;
#21111 = LINE ( 'NONE', #17743, #35627 ) ;
#21112 = PRODUCT_CONTEXT ( 'NONE', #12741, 'mechanical' ) ;
#21113 = DIRECTION ( 'NONE',  ( -0.000000000000000000, -0.000000000000000000, -1.000000000000000000 ) ) ;
#21114 = CIRCLE ( 'NONE', #25908, 2.000000000000001776 ) ;
#21115 = EDGE_CURVE ( 'NONE', #34695, #34700, #14631, .T. ) ;
#21116 = FACE_OUTER_BOUND ( 'NONE', #11401, .T. ) ;
#21117 = DIRECTION ( 'NONE',  ( 0.000000000000000000, 0.000000000000000000, 1.000000000000000000 ) ) ;
#21118 = ORIENTED_EDGE ( 'NONE', *, *, #16812, .T. ) ;
#21119 = EDGE_CURVE ( 'NONE', #16233, #26674, #7718, .T. ) ;
#21120 = CARTESIAN_POINT ( 'NONE',  ( -55.00000337463109901, -60.62177826491083010, -5.000000000000000000 ) ) ;
#21121 = CARTESIAN_POINT ( 'NONE',  ( 110.2237710830536770, 101.7384897088147397, 32.50000000000000000 ) ) ;
#21122 = CARTESIAN_POINT ( 'NONE',  ( 37.50000000000000000, 103.4105893997321743, 27.49999999999999645 ) ) ;
#21123 = ORIENTED_EDGE ( 'NONE', *, *, #20457, .F. ) ;
#21124 = ORIENTED_EDGE ( 'NONE', *, *, #15294, .T. ) ;
#21125 = VECTOR ( 'NONE', #14015, 1000.000000000000000 ) ;
#21126 = ORIENTED_EDGE ( 'NONE', *, *, #34380, .T. ) ;
#21127 = VECTOR ( 'NONE', #11324, 1000.000000000000000 ) ;
#21128 = EDGE_CURVE ( 'NONE', #25525, #27555, #33347, .T. ) ;
#21129 = CARTESIAN_POINT ( 'NONE',  ( 77.99999662536832545, -34.64101615137759183, 17.49999999999999645 ) ) ;
#21130 = DIRECTION ( 'NONE',  ( -0.000000000000000000, 0.000000000000000000, -1.000000000000000000 ) ) ;
#21131 = DIRECTION ( 'NONE',  ( 0.000000000000000000, 0.000000000000000000, 1.000000000000000000 ) ) ;
#21132 = PLANE ( 'NONE',  #19406 ) ;
#21133 = DIRECTION ( 'NONE',  ( 1.000000000000000000, 0.000000000000000000, 0.000000000000000000 ) ) ;
#21134 = CIRCLE ( 'NONE', #36722, 3.499999999999996003 ) ;
#21135 = DIRECTION ( 'NONE',  ( 0.000000000000000000, 0.000000000000000000, 1.000000000000000000 ) ) ;
#21136 = EDGE_CURVE ( 'NONE', #19500, #25394, #28994, .T. ) ;
#21137 = ORIENTED_EDGE ( 'NONE', *, *, #28257, .F. ) ;
#21139 = ORIENTED_EDGE ( 'NONE', *, *, #615, .T. ) ;
#21138 = EDGE_CURVE ( 'NONE', #34583, #17059, #30799, .T. ) ;
#21140 = AXIS2_PLACEMENT_3D ( 'NONE', #12563, #21185, #24017 ) ;
#21141 = DIRECTION ( 'NONE',  ( 0.000000000000000000, 0.000000000000000000, 1.000000000000000000 ) ) ;
#21142 = ADVANCED_FACE ( 'NONE', ( #35986 ), #7107, .F. ) ;
#21143 = CARTESIAN_POINT ( 'NONE',  ( 39.99999662536853151, -69.28203230275519786, -5.000000000000000000 ) ) ;
#21145 = EDGE_CURVE ( 'NONE', #16311, #31164, #1661, .T. ) ;
#21144 = ORIENTED_EDGE ( 'NONE', *, *, #5992, .F. ) ;
#21146 = PLANE ( 'NONE',  #18532 ) ;
#21147 = VERTEX_POINT ( 'NONE', #18908 ) ;
#21148 = FACE_BOUND ( 'NONE', #18312, .T. ) ;
#21149 = ORIENTED_EDGE ( 'NONE', *, *, #16907, .F. ) ;
#21150 = AXIS2_PLACEMENT_3D ( 'NONE', #19932, #8503, #20116 ) ;
#21151 = ORIENTED_EDGE ( 'NONE', *, *, #20999, .F. ) ;
#21152 = CYLINDRICAL_SURFACE ( 'NONE', #11628, 2.000000000000001776 ) ;
#21153 = ORIENTED_EDGE ( 'NONE', *, *, #25592, .F. ) ;
#21154 = PRODUCT_DEFINITION_SHAPE ( 'NONE', 'NONE',  #37113 ) ;
#21155 = CARTESIAN_POINT ( 'NONE',  ( 22.99999662536859901, -77.94228634059960825, -9.999999999999998224 ) ) ;
#21156 = CARTESIAN_POINT ( 'NONE',  ( 0.000000000000000000, 86.49289592134881843, -29.01554445662268833 ) ) ;
#21157 = CARTESIAN_POINT ( 'NONE',  ( -4.166666666666667851, -3.367876570272852366, -3.818275046351169877 ) ) ;
#21158 = EDGE_LOOP ( 'NONE', ( #5459, #15739 ) ) ;
#21159 = ORIENTED_EDGE ( 'NONE', *, *, #1313, .F. ) ;
#21160 = CIRCLE ( 'NONE', #19377, 2.000000000000001776 ) ;
#21161 = EDGE_LOOP ( 'NONE', ( #28245, #20035 ) ) ;
#21162 = EDGE_CURVE ( 'NONE', #10635, #5101, #15854, .T. ) ;
#21163 = ORIENTED_EDGE ( 'NONE', *, *, #25784, .T. ) ;
#21164 = AXIS2_PLACEMENT_3D ( 'NONE', #21935, #33379, #17773 ) ;
#21165 = EDGE_LOOP ( 'NONE', ( #3900, #21272, #9074, #35390 ) ) ;
#21166 = DIRECTION ( 'NONE',  ( 1.000000000000000000, 0.000000000000000000, 0.000000000000000000 ) ) ;
#21167 = CYLINDRICAL_SURFACE ( 'NONE', #31734, 3.499999999999996003 ) ;
#21168 = VERTEX_POINT ( 'NONE', #15344 ) ;
#21169 = CARTESIAN_POINT ( 'NONE',  ( 0.000000000000000000, 89.94802294027088863, -23.27834620192013304 ) ) ;
#21170 = CARTESIAN_POINT ( 'NONE',  ( 88.03899772796695800, 71.83443712190781127, 32.50000000000000000 ) ) ;
#21171 = DIRECTION ( 'NONE',  ( 1.000000000000000000, 0.000000000000000000, 0.000000000000000000 ) ) ;
#21172 = ORIENTED_EDGE ( 'NONE', *, *, #6778, .T. ) ;
#21173 = FACE_BOUND ( 'NONE', #12821, .T. ) ;
#21174 = VECTOR ( 'NONE', #10607, 1000.000000000000000 ) ;
#21175 = DIRECTION ( 'NONE',  ( 0.000000000000000000, 0.000000000000000000, 1.000000000000000000 ) ) ;
#21176 = AXIS2_PLACEMENT_3D ( 'NONE', #14450, #25521, #34713 ) ;
#21177 = CARTESIAN_POINT ( 'NONE',  ( -72.00000337463100664, 17.32050807568877460, -9.999999999999998224 ) ) ;
#21178 = ORIENTED_EDGE ( 'NONE', *, *, #10307, .F. ) ;
#21179 = CARTESIAN_POINT ( 'NONE',  ( 2.094888803305880329E-14, 6.000000000000000000, 27.50000000000000000 ) ) ;
#21180 = DIRECTION ( 'NONE',  ( 0.000000000000000000, 0.000000000000000000, 1.000000000000000000 ) ) ;
#21181 = VECTOR ( 'NONE', #28789, 1000.000000000000000 ) ;
#21182 = VERTEX_POINT ( 'NONE', #1847 ) ;
#21183 = ORIENTED_EDGE ( 'NONE', *, *, #29747, .T. ) ;
#21184 = DIRECTION ( 'NONE',  ( 0.000000000000000000, 0.000000000000000000, 1.000000000000000000 ) ) ;
#21185 = DIRECTION ( 'NONE',  ( -0.000000000000000000, 0.000000000000000000, -1.000000000000000000 ) ) ;
#21186 = EDGE_CURVE ( 'NONE', #14195, #4901, #3266, .T. ) ;
#21187 = CARTESIAN_POINT ( 'NONE',  ( -40.00000337463113453, 69.28203230275516944, -5.000000000000000000 ) ) ;
#21188 = FACE_OUTER_BOUND ( 'NONE', #92, .T. ) ;
#21189 = EDGE_LOOP ( 'NONE', ( #31835, #28865, #3734, #1587 ) ) ;
#21190 = CARTESIAN_POINT ( 'NONE',  ( 4.999996625368676284, -77.94228634059960825, -5.000000000000000000 ) ) ;
#21191 = CYLINDRICAL_SURFACE ( 'NONE', #32696, 95.00000000000001421 ) ;
#21192 = AXIS2_PLACEMENT_3D ( 'NONE', #1264, #27311, #9705 ) ;
#21193 = VERTEX_POINT ( 'NONE', #16111 ) ;
#21194 = CYLINDRICAL_SURFACE ( 'NONE', #9395, 2.000000000000001776 ) ;
#21195 = ORIENTED_EDGE ( 'NONE', *, *, #12075, .F. ) ;
#21196 = CARTESIAN_POINT ( 'NONE',  ( -72.00000337463102085, -51.96152422706641971, -9.999999999999998224 ) ) ;
#21197 = CARTESIAN_POINT ( 'NONE',  ( -82.00000337463094979, -17.32050807568882078, -9.999999999999998224 ) ) ;
#21198 = AXIS2_PLACEMENT_3D ( 'NONE', #30166, #1688, #13123 ) ;
#21199 = CARTESIAN_POINT ( 'NONE',  ( 3.667169054266697703, 3.656261651251516032, -0.8603634151101352545 ) ) ;
#21200 = ORIENTED_EDGE ( 'NONE', *, *, #15748, .T. ) ;
#21201 = ORIENTED_EDGE ( 'NONE', *, *, #6688, .F. ) ;
#21202 = EDGE_CURVE ( 'NONE', #12455, #10468, #1467, .T. ) ;
#21203 = ORIENTED_EDGE ( 'NONE', *, *, #10096, .F. ) ;
#21204 = DIRECTION ( 'NONE',  ( -1.000000000000000000, 0.000000000000000000, 0.000000000000000000 ) ) ;
#21205 = CARTESIAN_POINT ( 'NONE',  ( 65.63757102168601421, 58.72612563608866765, 12.50000000000000000 ) ) ;
#21206 = EDGE_CURVE ( 'NONE', #34302, #11641, #22429, .T. ) ;
#21207 = DIRECTION ( 'NONE',  ( -0.8660254037844453689, -0.4999999999999882871, 0.000000000000000000 ) ) ;
#21208 = CARTESIAN_POINT ( 'NONE',  ( -60.00000337463104216, 51.96152422706639129, 17.49999999999999645 ) ) ;
#21209 = DIRECTION ( 'NONE',  ( 0.000000000000000000, 0.000000000000000000, 1.000000000000000000 ) ) ;
#21210 = EDGE_LOOP ( 'NONE', ( #2385, #21352, #899, #24663 ) ) ;
#21211 = DIRECTION ( 'NONE',  ( -0.000000000000000000, -0.000000000000000000, 1.000000000000000000 ) ) ;
#21212 = AXIS2_PLACEMENT_3D ( 'NONE', #19349, #26720, #32915 ) ;
#21213 = DIRECTION ( 'NONE',  ( 1.000000000000000000, 0.000000000000000000, 0.000000000000000000 ) ) ;
#21214 = ADVANCED_FACE ( 'NONE', ( #36157 ), #9721, .F. ) ;
#21215 = CARTESIAN_POINT ( 'NONE',  ( -78.00000337463094979, -2.428612866367529932E-14, -5.000000000000000000 ) ) ;
#21216 = ORIENTED_EDGE ( 'NONE', *, *, #4171, .T. ) ;
#21217 = DIRECTION ( 'NONE',  ( 1.000000000000000000, 0.000000000000000000, 0.000000000000000000 ) ) ;
#21218 = LINE ( 'NONE', #27210, #13568 ) ;
#21219 = CARTESIAN_POINT ( 'NONE',  ( 62.99999662536841072, 25.98076211353318854, -9.999999999999998224 ) ) ;
#21220 = AXIS2_PLACEMENT_3D ( 'NONE', #6550, #17984, #20582 ) ;
#21221 = EDGE_LOOP ( 'NONE', ( #20922, #9911, #26482, #6205 ) ) ;
#21222 = AXIS2_PLACEMENT_3D ( 'NONE', #4894, #36393, #10703 ) ;
#21223 = ORIENTED_EDGE ( 'NONE', *, *, #9133, .F. ) ;
#21224 = AXIS2_PLACEMENT_3D ( 'NONE', #11990, #9175, #29604 ) ;
#21225 = DIRECTION ( 'NONE',  ( 1.000000000000000000, 0.000000000000000000, 0.000000000000000000 ) ) ;
#21226 = EDGE_CURVE ( 'NONE', #13437, #33271, #21712, .T. ) ;
#21227 = CARTESIAN_POINT ( 'NONE',  ( -80.00000337463094979, 34.64101615137757051, -9.999999999999998224 ) ) ;
#21228 = CARTESIAN_POINT ( 'NONE',  ( -23.49154088336464241, -103.5526315789473699, 27.50000000000000000 ) ) ;
#21229 = ORIENTED_EDGE ( 'NONE', *, *, #17151, .T. ) ;
#21230 = VERTEX_POINT ( 'NONE', #26974 ) ;
#21231 = ORIENTED_EDGE ( 'NONE', *, *, #11932, .T. ) ;
#21232 = CYLINDRICAL_SURFACE ( 'NONE', #32866, 6.000000000000005329 ) ;
#21233 = AXIS2_PLACEMENT_3D ( 'NONE', #1303, #29991, #12718 ) ;
#21234 = ORIENTED_EDGE ( 'NONE', *, *, #8629, .F. ) ;
#21235 = VERTEX_POINT ( 'NONE', #35800 ) ;
#21236 = CARTESIAN_POINT ( 'NONE',  ( -70.80619744048887299, 84.18124734178336155, 32.50000000000000000 ) ) ;
#21237 = ORIENTED_EDGE ( 'NONE', *, *, #19426, .F. ) ;
#21238 = VERTEX_POINT ( 'NONE', #33145 ) ;
#21239 = ADVANCED_FACE ( 'NONE', ( #13098 ), #21541, .T. ) ;
#21240 = AXIS2_PLACEMENT_3D ( 'NONE', #3038, #11452, #25728 ) ;
#21241 = DIRECTION ( 'NONE',  ( 0.000000000000000000, 0.000000000000000000, 1.000000000000000000 ) ) ;
#21242 = EDGE_CURVE ( 'NONE', #10050, #7613, #17049, .T. ) ;
#21243 = CARTESIAN_POINT ( 'NONE',  ( -2.775557561562891351E-14, 19.94802294027085310, -19.99999999999999645 ) ) ;
#21244 = ORIENTED_EDGE ( 'NONE', *, *, #22097, .T. ) ;
#21245 = EDGE_LOOP ( 'NONE', ( #18762, #25120, #2991, #17429 ) ) ;
#21246 = CARTESIAN_POINT ( 'NONE',  ( 19.99999662536861678, -86.60254037844400443, -9.999999999999998224 ) ) ;
#21247 = CARTESIAN_POINT ( 'NONE',  ( 72.99999662536836809, 8.660254037844394404, -9.999999999999998224 ) ) ;
#21248 = AXIS2_PLACEMENT_3D ( 'NONE', #8404, #19834, #23005 ) ;
#21249 = EDGE_CURVE ( 'NONE', #31238, #35117, #13835, .T. ) ;
#21250 = CARTESIAN_POINT ( 'NONE',  ( -32.00000337463119848, -69.28203230275522628, 17.49999999999999645 ) ) ;
#21251 = LINE ( 'NONE', #32687, #33475 ) ;
#21252 = ORIENTED_EDGE ( 'NONE', *, *, #20415, .T. ) ;
#21253 = CARTESIAN_POINT ( 'NONE',  ( 72.99999662536836809, -8.660254037844401509, -9.999999999999998224 ) ) ;
#21254 = ORIENTED_EDGE ( 'NONE', *, *, #23035, .T. ) ;
#21255 = FACE_OUTER_BOUND ( 'NONE', #10669, .T. ) ;
#21256 = ADVANCED_FACE ( 'NONE', ( #8214 ), #27888, .F. ) ;
#21257 = DIRECTION ( 'NONE',  ( 0.000000000000000000, 0.000000000000000000, 1.000000000000000000 ) ) ;
#21258 = DIRECTION ( 'NONE',  ( 1.000000000000000000, 0.000000000000000000, 0.000000000000000000 ) ) ;
#21259 = DIRECTION ( 'NONE',  ( 1.000000000000000000, 0.000000000000000000, 0.000000000000000000 ) ) ;
#21260 = DIRECTION ( 'NONE',  ( -0.000000000000000000, 0.000000000000000000, -1.000000000000000000 ) ) ;
#21261 = EDGE_CURVE ( 'NONE', #1919, #36051, #28417, .T. ) ;
#21262 = AXIS2_PLACEMENT_3D ( 'NONE', #35944, #32934, #24503 ) ;
#21263 = DIRECTION ( 'NONE',  ( 0.000000000000000000, 0.000000000000000000, 1.000000000000000000 ) ) ;
#21264 = VERTEX_POINT ( 'NONE', #2211 ) ;
#21266 = CIRCLE ( 'NONE', #13472, 2.000000000000001776 ) ;
#21265 = LINE ( 'NONE', #6831, #18413 ) ;
#21267 = CARTESIAN_POINT ( 'NONE',  ( -52.00000337463109190, 69.28203230275518365, -9.999999999999998224 ) ) ;
#21268 = DIRECTION ( 'NONE',  ( 0.000000000000000000, 0.000000000000000000, 1.000000000000000000 ) ) ;
#21269 = VECTOR ( 'NONE', #10647, 1000.000000000000000 ) ;
#21270 = ORIENTED_EDGE ( 'NONE', *, *, #13040, .F. ) ;
#21271 = AXIS2_PLACEMENT_3D ( 'NONE', #11960, #34681, #29395 ) ;
#21272 = ORIENTED_EDGE ( 'NONE', *, *, #31911, .T. ) ;
#21273 = ORIENTED_EDGE ( 'NONE', *, *, #28990, .F. ) ;
#21274 = CARTESIAN_POINT ( 'NONE',  ( -4.999999999999997335, 0.000000000000000000, 0.000000000000000000 ) ) ;
#21275 = CARTESIAN_POINT ( 'NONE',  ( -52.00000337463112032, -51.96152422706641971, -5.000000000000000000 ) ) ;
#21276 = FACE_OUTER_BOUND ( 'NONE', #11522, .T. ) ;
#21277 = VERTEX_POINT ( 'NONE', #34098 ) ;
#21278 = CIRCLE ( 'NONE', #5120, 3.499999999999989342 ) ;
#21279 = CIRCLE ( 'NONE', #24281, 2.000000000000000000 ) ;
#21280 = DIRECTION ( 'NONE',  ( 1.000000000000000000, 0.000000000000000000, 0.000000000000000000 ) ) ;
#21281 = ADVANCED_FACE ( 'NONE', ( #5575 ), #27700, .F. ) ;
#21282 = DIRECTION ( 'NONE',  ( 1.000000000000000000, 0.000000000000000000, 0.000000000000000000 ) ) ;
#21283 = EDGE_LOOP ( 'NONE', ( #21573, #14798, #15024, #22962 ) ) ;
#21284 = FACE_BOUND ( 'NONE', #26870, .T. ) ;
#21285 = VERTEX_POINT ( 'NONE', #8572 ) ;
#21286 = CARTESIAN_POINT ( 'NONE',  ( 76.99999662536836809, 25.98076211353319565, 17.49999999999999645 ) ) ;
#21287 = EDGE_CURVE ( 'NONE', #6253, #3167, #27238, .T. ) ;
#21288 = CARTESIAN_POINT ( 'NONE',  ( -22.00000337463122690, 86.60254037844397601, 12.50000000000000000 ) ) ;
#21289 = CARTESIAN_POINT ( 'NONE',  ( 4.749999999999999112, 6.447547231611302361E-16, 0.000000000000000000 ) ) ;
#21290 = CIRCLE ( 'NONE', #11724, 2.000000000000001776 ) ;
#21291 = EDGE_CURVE ( 'NONE', #34992, #4407, #5708, .T. ) ;
#21292 = LINE ( 'NONE', #32733, #3212 ) ;
#21293 = AXIS2_PLACEMENT_3D ( 'NONE', #22205, #28189, #22373 ) ;
#21294 = ORIENTED_EDGE ( 'NONE', *, *, #34929, .F. ) ;
#21295 = CARTESIAN_POINT ( 'NONE',  ( 22.99999662536859901, -77.94228634059960825, -5.000000000000000000 ) ) ;
#21296 = VECTOR ( 'NONE', #8589, 1000.000000000000000 ) ;
#21297 = VECTOR ( 'NONE', #10359, 1000.000000000000000 ) ;
#21298 = AXIS2_PLACEMENT_3D ( 'NONE', #11916, #26367, #31610 ) ;
#21299 = AXIS2_PLACEMENT_3D ( 'NONE', #13261, #35779, #27323 ) ;
#21300 = DIRECTION ( 'NONE',  ( 1.000000000000000000, 0.000000000000000000, 0.000000000000000000 ) ) ;
#21301 = FACE_OUTER_BOUND ( 'NONE', #28787, .T. ) ;
#21302 = CARTESIAN_POINT ( 'NONE',  ( -70.80619744048887299, 84.18124734178336155, 32.50000000000000000 ) ) ;
#21303 = VERTEX_POINT ( 'NONE', #2768 ) ;
#21304 = DIRECTION ( 'NONE',  ( 1.000000000000000000, 0.000000000000000000, 0.000000000000000000 ) ) ;
#21305 = DIRECTION ( 'NONE',  ( 1.000000000000000000, 0.000000000000000000, 0.000000000000000000 ) ) ;
#21306 = CARTESIAN_POINT ( 'NONE',  ( -10.00000337463127842, -69.28203230275519786, -5.000000000000000000 ) ) ;
#21307 = VERTEX_POINT ( 'NONE', #16287 ) ;
#21308 = ORIENTED_EDGE ( 'NONE', *, *, #22194, .F. ) ;
#21309 = EDGE_CURVE ( 'NONE', #5741, #6801, #36254, .T. ) ;
#21310 = EDGE_LOOP ( 'NONE', ( #27616, #12791, #5763, #35792 ) ) ;
#21311 = FACE_OUTER_BOUND ( 'NONE', #33024, .T. ) ;
#21312 = CARTESIAN_POINT ( 'NONE',  ( -20.00000337463124112, 69.28203230275516944, -9.999999999999998224 ) ) ;
#21313 = CIRCLE ( 'NONE', #3354, 2.000000000000001776 ) ;
#21314 = DIRECTION ( 'NONE',  ( 0.000000000000000000, -0.000000000000000000, -1.000000000000000000 ) ) ;
#21315 = VERTEX_POINT ( 'NONE', #28261 ) ;
#21316 = AXIS2_PLACEMENT_3D ( 'NONE', #19172, #10336, #33030 ) ;
#21317 = CARTESIAN_POINT ( 'NONE',  ( -43.19957991610399972, -47.04203867989563292, 12.49999999999999822 ) ) ;
#21318 = DIRECTION ( 'NONE',  ( 0.000000000000000000, 0.000000000000000000, -1.000000000000000000 ) ) ;
#21319 = CIRCLE ( 'NONE', #26115, 2.000000000000001776 ) ;
#21320 = CYLINDRICAL_SURFACE ( 'NONE', #31007, 2.000000000000001776 ) ;
#21321 = AXIS2_PLACEMENT_3D ( 'NONE', #4327, #15583, #1701 ) ;
#21322 = ORIENTED_EDGE ( 'NONE', *, *, #33709, .T. ) ;
#21323 = AXIS2_PLACEMENT_3D ( 'NONE', #28558, #33650, #16389 ) ;
#21324 = EDGE_LOOP ( 'NONE', ( #7246, #33580 ) ) ;
#21325 = FACE_OUTER_BOUND ( 'NONE', #25455, .T. ) ;
#21326 = VECTOR ( 'NONE', #20639, 1000.000000000000000 ) ;
#21327 = ADVANCED_FACE ( 'NONE', ( #2580 ), #25452, .F. ) ;
#21328 = PLANE ( 'NONE',  #34347 ) ;
#21329 = ORIENTED_EDGE ( 'NONE', *, *, #18007, .F. ) ;
#21330 = EDGE_CURVE ( 'NONE', #29660, #24005, #19651, .T. ) ;
#21331 = CARTESIAN_POINT ( 'NONE',  ( -68.00000337463099243, 51.96152422706637708, -9.999999999999998224 ) ) ;
#21332 = ORIENTED_EDGE ( 'NONE', *, *, #10453, .F. ) ;
#21333 = DIRECTION ( 'NONE',  ( 0.000000000000000000, 0.000000000000000000, 1.000000000000000000 ) ) ;
#21334 = AXIS2_PLACEMENT_3D ( 'NONE', #14514, #14687, #12217 ) ;
#21335 = ADVANCED_FACE ( 'NONE', ( #36891 ), #5411, .F. ) ;
#21336 = FACE_BOUND ( 'NONE', #14260, .T. ) ;
#21337 = VERTEX_POINT ( 'NONE', #25109 ) ;
#21338 = EDGE_LOOP ( 'NONE', ( #15250, #5522, #32870, #33979, #3757, #26440, #19559 ) ) ;
#21339 = EDGE_CURVE ( 'NONE', #5803, #3751, #19465, .T. ) ;
#21340 = CARTESIAN_POINT ( 'NONE',  ( 34.99999662536855283, -60.62177826491080168, -9.999999999999998224 ) ) ;
#21341 = VERTEX_POINT ( 'NONE', #30700 ) ;
#21342 = ADVANCED_FACE ( 'NONE', ( #5020 ), #8700, .T. ) ;
#21343 = PLANE ( 'NONE',  #36224 ) ;
#21344 = AXIS2_PLACEMENT_3D ( 'NONE', #5588, #14721, #2427 ) ;
#21345 = DIRECTION ( 'NONE',  ( 1.000000000000000000, 0.000000000000000000, 0.000000000000000000 ) ) ;
#21346 = CARTESIAN_POINT ( 'NONE',  ( 0.000000000000000000, 0.000000000000000000, -0.3501037691048548561 ) ) ;
#21347 = ORIENTED_EDGE ( 'NONE', *, *, #2626, .T. ) ;
#21348 = DIRECTION ( 'NONE',  ( 0.000000000000000000, 0.000000000000000000, 1.000000000000000000 ) ) ;
#21349 = MECHANICAL_DESIGN_GEOMETRIC_PRESENTATION_REPRESENTATION (  '', ( #21944 ), #4613 ) ;
#21350 = VECTOR ( 'NONE', #22362, 1000.000000000000000 ) ;
#21351 = ADVANCED_FACE ( 'NONE', ( #30882 ), #28085, .F. ) ;
#21352 = ORIENTED_EDGE ( 'NONE', *, *, #28098, .F. ) ;
#21353 = AXIS2_PLACEMENT_3D ( 'NONE', #21668, #9850, #6851 ) ;
#21354 = CIRCLE ( 'NONE', #24962, 30.00000000000001421 ) ;
#21355 = EDGE_CURVE ( 'NONE', #28135, #35764, #1496, .T. ) ;
#21356 = ORIENTED_EDGE ( 'NONE', *, *, #6112, .T. ) ;
#21357 = AXIS2_PLACEMENT_3D ( 'NONE', #30669, #27847, #2175 ) ;
#21358 = EDGE_LOOP ( 'NONE', ( #34357, #27753, #30047, #11929 ) ) ;
#21359 = EDGE_CURVE ( 'NONE', #2691, #14593, #20071, .T. ) ;
#21360 = DIRECTION ( 'NONE',  ( 0.000000000000000000, 0.000000000000000000, -1.000000000000000000 ) ) ;
#21361 = EDGE_CURVE ( 'NONE', #3947, #35128, #26658, .T. ) ;
#21362 = CARTESIAN_POINT ( 'NONE',  ( -70.00000337463099243, -2.428612866367529932E-14, -9.999999999999998224 ) ) ;
#21363 = VERTEX_POINT ( 'NONE', #14950 ) ;
#21364 = CARTESIAN_POINT ( 'NONE',  ( -4.999999999999998224, -2.058885705017527989, -1.328630925609301183 ) ) ;
#21365 = CYLINDRICAL_SURFACE ( 'NONE', #24979, 2.000000000000001776 ) ;
#21366 = ORIENTED_EDGE ( 'NONE', *, *, #5992, .T. ) ;
#21367 = CARTESIAN_POINT ( 'NONE',  ( -42.00000337463114164, -69.28203230275519786, 12.50000000000000000 ) ) ;
#21368 = AXIS2_PLACEMENT_3D ( 'NONE', #17297, #29068, #6204 ) ;
#21369 = CARTESIAN_POINT ( 'NONE',  ( -70.00000337463100664, -17.32050807568882078, -9.999999999999998224 ) ) ;
#21370 = LINE ( 'NONE', #36372, #36202 ) ;
#21371 = CYLINDRICAL_SURFACE ( 'NONE', #8905, 2.000000000000001776 ) ;
#21372 = CYLINDRICAL_SURFACE ( 'NONE', #7604, 27.00000000000001066 ) ;
#21373 = FACE_OUTER_BOUND ( 'NONE', #34226, .T. ) ;
#21374 = VERTEX_POINT ( 'NONE', #34823 ) ;
#21375 = AXIS2_PLACEMENT_3D ( 'NONE', #25164, #36409, #22707 ) ;
#21376 = ORIENTED_EDGE ( 'NONE', *, *, #25271, .F. ) ;
#21377 = DIRECTION ( 'NONE',  ( 1.000000000000000000, 0.000000000000000000, 0.000000000000000000 ) ) ;
#21378 = CIRCLE ( 'NONE', #21344, 5.999999999999999112 ) ;
#21379 = AXIS2_PLACEMENT_3D ( 'NONE', #18195, #957, #3408 ) ;
#21380 = LINE ( 'NONE', #26825, #22940 ) ;
#21381 = CARTESIAN_POINT ( 'NONE',  ( 0.000000000000000000, 0.000000000000000000, -5.132899837730832360 ) ) ;
#21382 = DIRECTION ( 'NONE',  ( 1.000000000000000000, 0.000000000000000000, 0.000000000000000000 ) ) ;
#21383 = AXIS2_PLACEMENT_3D ( 'NONE', #23522, #32502, #1019 ) ;
#21384 = VERTEX_POINT ( 'NONE', #28632 ) ;
#21385 = AXIS2_PLACEMENT_3D ( 'NONE', #8896, #30384, #36396 ) ;
#21387 = AXIS2_PLACEMENT_3D ( 'NONE', #10135, #35630, #18380 ) ;
#21386 = CARTESIAN_POINT ( 'NONE',  ( 84.99999662536832545, 25.98076211353319565, 17.49999999999999645 ) ) ;
#21388 = CARTESIAN_POINT ( 'NONE',  ( 0.000000000000000000, 0.000000000000000000, -15.00000000000000000 ) ) ;
#21389 = AXIS2_PLACEMENT_3D ( 'NONE', #13697, #25153, #10876 ) ;
#21390 = CIRCLE ( 'NONE', #26178, 95.00000000000001421 ) ;
#21391 = ORIENTED_EDGE ( 'NONE', *, *, #11484, .T. ) ;
#21392 = FACE_OUTER_BOUND ( 'NONE', #27429, .T. ) ;
#21393 = ORIENTED_EDGE ( 'NONE', *, *, #25440, .F. ) ;
#21394 = AXIS2_PLACEMENT_3D ( 'NONE', #5378, #19614, #10621 ) ;
#21395 = CARTESIAN_POINT ( 'NONE',  ( -58.88972745734155723, 34.00000000000049027, -4.999999999999997335 ) ) ;
#21396 = CIRCLE ( 'NONE', #5238, 2.000000000000001776 ) ;
#21397 = LINE ( 'NONE', #21197, #25409 ) ;
#21398 = CARTESIAN_POINT ( 'NONE',  ( 2.739742549670660665, 4.191711593333631747, -0.5197061503823161566 ) ) ;
#21399 = ORIENTED_EDGE ( 'NONE', *, *, #11060, .F. ) ;
#21400 = ORIENTED_EDGE ( 'NONE', *, *, #24207, .F. ) ;
#21401 = CIRCLE ( 'NONE', #14225, 150.0000000000000284 ) ;
#21402 = CIRCLE ( 'NONE', #35206, 2.000000000000001776 ) ;
#21403 = VERTEX_POINT ( 'NONE', #9116 ) ;
#21404 = DIRECTION ( 'NONE',  ( -0.7071067811865388020, 0.7071067811865563435, 0.000000000000000000 ) ) ;
#21405 = EDGE_CURVE ( 'NONE', #16746, #10350, #23755, .T. ) ;
#21406 = FACE_BOUND ( 'NONE', #2477, .T. ) ;
#21407 = CARTESIAN_POINT ( 'NONE',  ( -5.000003374631307729, 77.94228634059957983, -9.999999999999998224 ) ) ;
#21408 = DIRECTION ( 'NONE',  ( 1.000000000000000000, 0.000000000000000000, 0.000000000000000000 ) ) ;
#21409 = DIRECTION ( 'NONE',  ( 1.000000000000000000, 0.000000000000000000, 0.000000000000000000 ) ) ;
#21410 =( GEOMETRIC_REPRESENTATION_CONTEXT ( 3 ) GLOBAL_UNCERTAINTY_ASSIGNED_CONTEXT ( ( #18945 ) ) GLOBAL_UNIT_ASSIGNED_CONTEXT ( ( #11779, #23041, #11247 ) ) REPRESENTATION_CONTEXT ( 'NONE', 'WORKASPACE' ) );
#21411 = ORIENTED_EDGE ( 'NONE', *, *, #23567, .F. ) ;
#21412 = DIRECTION ( 'NONE',  ( 0.000000000000000000, 0.000000000000000000, -1.000000000000000000 ) ) ;
#21413 = AXIS2_PLACEMENT_3D ( 'NONE', #27916, #18932, #30359 ) ;
#21414 = CARTESIAN_POINT ( 'NONE',  ( 0.000000000000000000, 0.000000000000000000, 0.000000000000000000 ) ) ;
#21415 = FILL_AREA_STYLE_COLOUR ( '', #18198 ) ;
#21416 = VERTEX_POINT ( 'NONE', #14749 ) ;
#21417 =( REPRESENTATION_RELATIONSHIP ('NONE','NONE', #15268, #33015 ) REPRESENTATION_RELATIONSHIP_WITH_TRANSFORMATION ( #36842 )SHAPE_REPRESENTATION_RELATIONSHIP( ) );
#21418 = DIRECTION ( 'NONE',  ( 0.000000000000000000, 0.000000000000000000, 1.000000000000000000 ) ) ;
#21419 = FACE_BOUND ( 'NONE', #6041, .T. ) ;
#21420 = VECTOR ( 'NONE', #34793, 1000.000000000000000 ) ;
#21421 = ORIENTED_EDGE ( 'NONE', *, *, #2064, .F. ) ;
#21422 = ORIENTED_EDGE ( 'NONE', *, *, #18072, .F. ) ;
#21423 = VECTOR ( 'NONE', #21426, 1000.000000000000000 ) ;
#21424 = CARTESIAN_POINT ( 'NONE',  ( 32.99999662536853862, 77.94228634059959404, -9.999999999999998224 ) ) ;
#21425 = LINE ( 'NONE', #27039, #23550 ) ;
#21426 = DIRECTION ( 'NONE',  ( 0.000000000000000000, 0.000000000000000000, 1.000000000000000000 ) ) ;
#21427 = ORIENTED_EDGE ( 'NONE', *, *, #30554, .T. ) ;
#21428 = ORIENTED_EDGE ( 'NONE', *, *, #35966, .T. ) ;
#21429 = CIRCLE ( 'NONE', #32197, 2.000000000000000000 ) ;
#21430 = EDGE_LOOP ( 'NONE', ( #23620, #14029, #13382, #4140 ) ) ;
#21431 = EDGE_CURVE ( 'NONE', #13150, #34663, #24854, .T. ) ;
#21432 = EDGE_CURVE ( 'NONE', #28343, #4869, #29617, .T. ) ;
#21433 = AXIS2_PLACEMENT_3D ( 'NONE', #12286, #11941, #3697 ) ;
#21434 = CYLINDRICAL_SURFACE ( 'NONE', #2135, 2.000000000000000000 ) ;
#21435 = AXIS2_PLACEMENT_3D ( 'NONE', #63, #16776, #5887 ) ;
#21436 = VERTEX_POINT ( 'NONE', #35207 ) ;
#21437 = ORIENTED_EDGE ( 'NONE', *, *, #6151, .T. ) ;
#21438 = DIRECTION ( 'NONE',  ( -0.000000000000000000, -0.000000000000000000, 1.000000000000000000 ) ) ;
#21439 = ORIENTED_EDGE ( 'NONE', *, *, #35048, .F. ) ;
#21440 = ORIENTED_EDGE ( 'NONE', *, *, #10435, .T. ) ;
#21441 = AXIS2_PLACEMENT_3D ( 'NONE', #2312, #36991, #11300 ) ;
#21442 = EDGE_CURVE ( 'NONE', #13349, #3694, #11653, .T. ) ;
#21443 = CARTESIAN_POINT ( 'NONE',  ( -72.00000337463102085, -34.64101615137762025, 17.49999999999999645 ) ) ;
#21444 = CARTESIAN_POINT ( 'NONE',  ( 37.50000000000000000, 103.4105893997321743, -11.00000000000000355 ) ) ;
#21445 = VERTEX_POINT ( 'NONE', #23558 ) ;
#21446 = ORIENTED_EDGE ( 'NONE', *, *, #1152, .F. ) ;
#21447 = DIRECTION ( 'NONE',  ( 1.000000000000000000, 0.000000000000000000, 0.000000000000000000 ) ) ;
#21448 = CIRCLE ( 'NONE', #10077, 2.000000000000001776 ) ;
#21449 = CARTESIAN_POINT ( 'NONE',  ( -15.00000337463125710, -77.94228634059960825, 12.50000000000000000 ) ) ;
#21450 = LINE ( 'NONE', #29498, #18678 ) ;
#21451 = CYLINDRICAL_SURFACE ( 'NONE', #1095, 2.000000000000001776 ) ;
#21452 = VERTEX_POINT ( 'NONE', #3312 ) ;
#21453 = DIRECTION ( 'NONE',  ( -1.000000000000000000, 0.000000000000000000, 0.000000000000000000 ) ) ;
#21454 = VECTOR ( 'NONE', #20456, 1000.000000000000000 ) ;
#21455 = VERTEX_POINT ( 'NONE', #11742 ) ;
#21456 = EDGE_CURVE ( 'NONE', #5647, #27967, #18248, .T. ) ;
#21457 = DIRECTION ( 'NONE',  ( 0.000000000000000000, 0.000000000000000000, 1.000000000000000000 ) ) ;
#21458 = CIRCLE ( 'NONE', #5306, 2.000000000000001776 ) ;
#21459 = CYLINDRICAL_SURFACE ( 'NONE', #13019, 2.000000000000001776 ) ;
#21460 = CYLINDRICAL_SURFACE ( 'NONE', #36363, 3.500000000000000888 ) ;
#21461 = CARTESIAN_POINT ( 'NONE',  ( -65.00000337463104927, -43.30127018922202353, -9.999999999999998224 ) ) ;
#21463 = CIRCLE ( 'NONE', #19001, 2.000000000000001776 ) ;
#21462 = FACE_OUTER_BOUND ( 'NONE', #9447, .T. ) ;
#21464 = CARTESIAN_POINT ( 'NONE',  ( 24.99999662536857059, 77.94228634059957983, -9.999999999999998224 ) ) ;
#21465 = CIRCLE ( 'NONE', #12453, 2.000000000000001776 ) ;
#21466 = FACE_OUTER_BOUND ( 'NONE', #6938, .T. ) ;
#21467 = ORIENTED_EDGE ( 'NONE', *, *, #17457, .F. ) ;
#21468 = DIRECTION ( 'NONE',  ( 0.000000000000000000, 0.000000000000000000, 1.000000000000000000 ) ) ;
#21469 = DIRECTION ( 'NONE',  ( 0.000000000000000000, 0.000000000000000000, 1.000000000000000000 ) ) ;
#21470 = DIRECTION ( 'NONE',  ( 0.000000000000000000, 0.000000000000000000, 1.000000000000000000 ) ) ;
#21471 = CIRCLE ( 'NONE', #586, 2.000000000000001776 ) ;
#21472 = ORIENTED_EDGE ( 'NONE', *, *, #15377, .T. ) ;
#21473 = AXIS2_PLACEMENT_3D ( 'NONE', #25916, #11307, #17307 ) ;
#21474 = EDGE_LOOP ( 'NONE', ( #6437, #8684 ) ) ;
#21475 = ORIENTED_EDGE ( 'NONE', *, *, #4874, .F. ) ;
#21476 = EDGE_CURVE ( 'NONE', #7527, #11869, #34433, .T. ) ;
#21477 = CARTESIAN_POINT ( 'NONE',  ( 66.98486176412667703, -43.54685190870066691, -5.000000000000000000 ) ) ;
#21478 = CARTESIAN_POINT ( 'NONE',  ( 64.99999662536839651, -60.62177826491080168, -9.999999999999998224 ) ) ;
#21479 = DIRECTION ( 'NONE',  ( 0.000000000000000000, 0.000000000000000000, 1.000000000000000000 ) ) ;
#21480 = ORIENTED_EDGE ( 'NONE', *, *, #5860, .F. ) ;
#21481 = AXIS2_PLACEMENT_3D ( 'NONE', #1066, #26750, #14565 ) ;
#21482 = EDGE_CURVE ( 'NONE', #24628, #35778, #23042, .T. ) ;
#21483 = CARTESIAN_POINT ( 'NONE',  ( 58.48108235278871803, 36.97203788308964789, -49.86561046011506448 ) ) ;
#21484 = AXIS2_PLACEMENT_3D ( 'NONE', #21955, #16505, #14254 ) ;
#21485 = DIRECTION ( 'NONE',  ( 0.000000000000000000, 0.000000000000000000, 1.000000000000000000 ) ) ;
#21486 = ORIENTED_EDGE ( 'NONE', *, *, #23539, .T. ) ;
#21487 = DIRECTION ( 'NONE',  ( 1.000000000000000000, 0.000000000000000000, 0.000000000000000000 ) ) ;
#21488 = ADVANCED_FACE ( 'NONE', ( #29373 ), #26551, .F. ) ;
#21489 = ORIENTED_EDGE ( 'NONE', *, *, #36702, .T. ) ;
#21490 = AXIS2_PLACEMENT_3D ( 'NONE', #119, #14744, #25997 ) ;
#21491 = DIRECTION ( 'NONE',  ( 1.000000000000000000, 0.000000000000000000, -0.000000000000000000 ) ) ;
#21492 = EDGE_CURVE ( 'NONE', #12315, #20659, #3294, .T. ) ;
#21493 = DIRECTION ( 'NONE',  ( -1.000000000000000000, 0.000000000000000000, 0.000000000000000000 ) ) ;
#21494 = LINE ( 'NONE', #10795, #30526 ) ;
#21495 = AXIS2_PLACEMENT_3D ( 'NONE', #2906, #31372, #34225 ) ;
#21496 = ORIENTED_EDGE ( 'NONE', *, *, #22695, .T. ) ;
#21497 = DIRECTION ( 'NONE',  ( -1.000000000000000000, 0.000000000000000000, 0.000000000000000000 ) ) ;
#21498 = CIRCLE ( 'NONE', #32873, 27.00000000000001776 ) ;
#21499 = CARTESIAN_POINT ( 'NONE',  ( -70.47608876694631874, -59.13646009116124702, -49.22241343995298024 ) ) ;
#21500 = CARTESIAN_POINT ( 'NONE',  ( -67.00000337463106348, -60.62177826491083010, -9.999999999999998224 ) ) ;
#21501 = CARTESIAN_POINT ( 'NONE',  ( 74.99999662536836809, 8.660254037844394404, 12.50000000000000000 ) ) ;
#21502 = ORIENTED_EDGE ( 'NONE', *, *, #10501, .T. ) ;
#21503 = DIRECTION ( 'NONE',  ( 0.000000000000000000, 0.000000000000000000, 1.000000000000000000 ) ) ;
#21504 = DIRECTION ( 'NONE',  ( 0.000000000000000000, 0.000000000000000000, 1.000000000000000000 ) ) ;
#21505 = DIRECTION ( 'NONE',  ( 1.000000000000000000, 0.000000000000000000, 0.000000000000000000 ) ) ;
#21506 = EDGE_CURVE ( 'NONE', #15689, #16094, #6877, .T. ) ;
#21507 = ORIENTED_EDGE ( 'NONE', *, *, #1810, .T. ) ;
#21508 = VECTOR ( 'NONE', #1664, 1000.000000000000000 ) ;
#21509 = ORIENTED_EDGE ( 'NONE', *, *, #28916, .F. ) ;
#21510 = CIRCLE ( 'NONE', #20926, 2.000000000000001776 ) ;
#21511 = DIRECTION ( 'NONE',  ( 1.000000000000000000, 0.000000000000000000, 0.000000000000000000 ) ) ;
#21512 = DIRECTION ( 'NONE',  ( 0.000000000000000000, 0.000000000000000000, 1.000000000000000000 ) ) ;
#21513 = EDGE_CURVE ( 'NONE', #3560, #36161, #26196, .T. ) ;
#21514 = CARTESIAN_POINT ( 'NONE',  ( -10.00000337463128197, 86.60254037844397601, -9.999999999999998224 ) ) ;
#21515 = EDGE_LOOP ( 'NONE', ( #6593, #24693 ) ) ;
#21516 = VECTOR ( 'NONE', #13223, 1000.000000000000000 ) ;
#21517 = ADVANCED_FACE ( 'NONE', ( #20198 ), #8947, .F. ) ;
#21518 = DIRECTION ( 'NONE',  ( -1.000000000000000000, 0.000000000000000000, 0.000000000000000000 ) ) ;
#21519 = DIRECTION ( 'NONE',  ( -0.000000000000000000, -0.000000000000000000, 1.000000000000000000 ) ) ;
#21520 = CYLINDRICAL_SURFACE ( 'NONE', #22580, 25.00000000000000000 ) ;
#21522 = CARTESIAN_POINT ( 'NONE',  ( -107.0107044000184402, 51.13684811647830486, 32.50000000000000000 ) ) ;
#21521 = AXIS2_PLACEMENT_3D ( 'NONE', #35978, #2202, #2009 ) ;
#21523 = ORIENTED_EDGE ( 'NONE', *, *, #10155, .F. ) ;
#21524 = ORIENTED_EDGE ( 'NONE', *, *, #4522, .T. ) ;
#21525 = CARTESIAN_POINT ( 'NONE',  ( -83.00000337463092137, 25.98076211353317433, -5.000000000000000000 ) ) ;
#21526 = AXIS2_PLACEMENT_3D ( 'NONE', #33667, #21669, #33097 ) ;
#21527 = DIRECTION ( 'NONE',  ( -1.000000000000000000, 0.000000000000000000, 0.000000000000000000 ) ) ;
#21528 = VERTEX_POINT ( 'NONE', #5961 ) ;
#21529 = CIRCLE ( 'NONE', #16748, 2.000000000000001776 ) ;
#21530 = FACE_OUTER_BOUND ( 'NONE', #24562, .T. ) ;
#21531 = ORIENTED_EDGE ( 'NONE', *, *, #23866, .T. ) ;
#21532 = LINE ( 'NONE', #27877, #35693 ) ;
#21533 = EDGE_CURVE ( 'NONE', #18729, #32725, #33245, .T. ) ;
#21534 = CARTESIAN_POINT ( 'NONE',  ( 76.99999662536836809, -8.660254037844401509, -9.999999999999998224 ) ) ;
#21535 = AXIS2_PLACEMENT_3D ( 'NONE', #12491, #1615, #865 ) ;
#21536 = ORIENTED_EDGE ( 'NONE', *, *, #35053, .T. ) ;
#21537 = ORIENTED_EDGE ( 'NONE', *, *, #24552, .F. ) ;
#21538 = AXIS2_PLACEMENT_3D ( 'NONE', #4675, #7467, #7288 ) ;
#21539 = CARTESIAN_POINT ( 'NONE',  ( 69.99999662536841072, 51.96152422706640550, -9.999999999999998224 ) ) ;
#21540 = EDGE_LOOP ( 'NONE', ( #26586, #34171 ) ) ;
#21541 = PLANE ( 'NONE',  #27211 ) ;
#21542 = DIRECTION ( 'NONE',  ( 0.000000000000000000, 0.000000000000000000, 1.000000000000000000 ) ) ;
#21543 = CARTESIAN_POINT ( 'NONE',  ( -58.88972745734203329, -33.99999999999965894, 12.49999999999999822 ) ) ;
#21544 = VERTEX_POINT ( 'NONE', #14560 ) ;
#21545 = DIRECTION ( 'NONE',  ( 1.000000000000000000, 0.000000000000000000, 0.000000000000000000 ) ) ;
#21546 = CARTESIAN_POINT ( 'NONE',  ( 59.99999662536843914, -34.64101615137759893, -5.000000000000000000 ) ) ;
#21547 = AXIS2_PLACEMENT_3D ( 'NONE', #35932, #13036, #1409 ) ;
#21548 = ORIENTED_EDGE ( 'NONE', *, *, #31934, .F. ) ;
#21549 = EDGE_LOOP ( 'NONE', ( #34879, #14405, #11457, #36208 ) ) ;
#21550 = CIRCLE ( 'NONE', #5397, 2.000000000000001776 ) ;
#21551 = EDGE_CURVE ( 'NONE', #2028, #13905, #20650, .T. ) ;
#21552 = VERTEX_POINT ( 'NONE', #30296 ) ;
#21553 = CARTESIAN_POINT ( 'NONE',  ( -1.084202172485504434E-14, -5.773502691896260863, -2.080000000000000071 ) ) ;
#21554 = AXIS2_PLACEMENT_3D ( 'NONE', #22375, #19382, #10771 ) ;
#21555 = DIRECTION ( 'NONE',  ( -0.7071067811865539010, -0.7071067811865411334, 0.000000000000000000 ) ) ;
#21556 = EDGE_CURVE ( 'NONE', #32159, #33756, #30824, .T. ) ;
#21557 = ORIENTED_EDGE ( 'NONE', *, *, #31094, .F. ) ;
#21558 = DIRECTION ( 'NONE',  ( 1.000000000000000000, 0.000000000000000000, 0.000000000000000000 ) ) ;
#21559 = CIRCLE ( 'NONE', #34150, 3.500000000000003109 ) ;
#21560 = CARTESIAN_POINT ( 'NONE',  ( 0.000000000000000000, 89.94802294027088863, -19.99999999999999645 ) ) ;
#21561 = ORIENTED_EDGE ( 'NONE', *, *, #22493, .T. ) ;
#21562 = DIRECTION ( 'NONE',  ( -0.8660254037844378194, 0.5000000000000014433, 0.000000000000000000 ) ) ;
#21563 = EDGE_CURVE ( 'NONE', #18966, #8725, #29020, .T. ) ;
#21564 = DIRECTION ( 'NONE',  ( 0.000000000000000000, 0.000000000000000000, -1.000000000000000000 ) ) ;
#21565 = VECTOR ( 'NONE', #21073, 1000.000000000000114 ) ;
#21566 = CARTESIAN_POINT ( 'NONE',  ( 82.99999662536832545, 25.98076211353319565, -9.999999999999998224 ) ) ;
#21567 = CARTESIAN_POINT ( 'NONE',  ( 79.99999662536833966, 34.64101615137759183, -5.000000000000000000 ) ) ;
#21568 = EDGE_CURVE ( 'NONE', #25550, #16224, #17658, .T. ) ;
#21569 = AXIS2_PLACEMENT_3D ( 'NONE', #13965, #2373, #36504 ) ;
#21570 = CARTESIAN_POINT ( 'NONE',  ( 61.99999662536842493, 51.96152422706639129, 17.49999999999999645 ) ) ;
#21571 = ADVANCED_FACE ( 'NONE', ( #15303 ), #29931, .T. ) ;
#21572 = DIRECTION ( 'NONE',  ( 0.000000000000000000, 0.000000000000000000, 1.000000000000000000 ) ) ;
#21573 = ORIENTED_EDGE ( 'NONE', *, *, #26979, .F. ) ;
#21574 = ORIENTED_EDGE ( 'NONE', *, *, #33249, .F. ) ;
#21575 = CARTESIAN_POINT ( 'NONE',  ( 39.99999662536853151, -69.28203230275519786, -9.999999999999998224 ) ) ;
#21576 = DIRECTION ( 'NONE',  ( -1.000000000000000000, 0.000000000000000000, 0.000000000000000000 ) ) ;
#21577 = CARTESIAN_POINT ( 'NONE',  ( -62.33939050065184517, 13.89091430021398565, 12.49999999999999822 ) ) ;
#21578 = CIRCLE ( 'NONE', #30570, 2.000000000000001776 ) ;
#21579 = CARTESIAN_POINT ( 'NONE',  ( -34.00000000000000000, -103.4105893997321743, 32.50000000000000000 ) ) ;
#21580 = EDGE_LOOP ( 'NONE', ( #17950, #4949, #7371, #13094, #8401, #9066, #22585, #20411, #19354, #4501 ) ) ;
#21581 = EDGE_CURVE ( 'NONE', #8343, #27735, #26746, .T. ) ;
#21582 = DIRECTION ( 'NONE',  ( 1.000000000000000000, 0.000000000000000000, 0.000000000000000000 ) ) ;
#21583 = ADVANCED_FACE ( 'NONE', ( #23950 ), #18113, .F. ) ;
#21584 = CARTESIAN_POINT ( 'NONE',  ( -43.00000337463111322, 60.62177826491077326, -9.999999999999998224 ) ) ;
#21585 = EDGE_CURVE ( 'NONE', #5993, #281, #27290, .T. ) ;
#21586 = CARTESIAN_POINT ( 'NONE',  ( 0.000000000000000000, -55.00000000000000000, -10.00000000000000000 ) ) ;
#21587 = ORIENTED_EDGE ( 'NONE', *, *, #28206, .T. ) ;
#21588 = EDGE_CURVE ( 'NONE', #31151, #27157, #12288, .T. ) ;
#21589 = VECTOR ( 'NONE', #35065, 1000.000000000000000 ) ;
#21590 = EDGE_CURVE ( 'NONE', #10255, #17870, #29731, .T. ) ;
#21591 = CARTESIAN_POINT ( 'NONE',  ( -85.00000337463092137, 8.660254037844389075, -5.000000000000000000 ) ) ;
#21592 = AXIS2_PLACEMENT_3D ( 'NONE', #36956, #14440, #8812 ) ;
#21593 = EDGE_LOOP ( 'NONE', ( #21472, #12606, #26452, #19827 ) ) ;
#21594 = CARTESIAN_POINT ( 'NONE',  ( 3.000000000000000000, 2.935248768560057453, -3.903127820947815962E-15 ) ) ;
#21595 = CARTESIAN_POINT ( 'NONE',  ( 0.000000000000000000, -55.00000000000000000, -15.00000000000000000 ) ) ;
#21596 = CARTESIAN_POINT ( 'NONE',  ( -31.02796211690907668, 59.29837256189569672, 12.49999999999999645 ) ) ;
#21597 = VERTEX_POINT ( 'NONE', #3860 ) ;
#21598 = VERTEX_POINT ( 'NONE', #1423 ) ;
#21599 = ORIENTED_EDGE ( 'NONE', *, *, #2684, .T. ) ;
#21600 = DIRECTION ( 'NONE',  ( 0.000000000000000000, 0.000000000000000000, 1.000000000000000000 ) ) ;
#21601 = FACE_BOUND ( 'NONE', #35654, .T. ) ;
#21602 = DIRECTION ( 'NONE',  ( 0.000000000000000000, 0.000000000000000000, 1.000000000000000000 ) ) ;
#21603 = CYLINDRICAL_SURFACE ( 'NONE', #18125, 3.750000000000001776 ) ;
#21604 = LINE ( 'NONE', #35661, #12326 ) ;
#21605 = ORIENTED_EDGE ( 'NONE', *, *, #34648, .T. ) ;
#21606 = FACE_OUTER_BOUND ( 'NONE', #22678, .T. ) ;
#21607 = DIRECTION ( 'NONE',  ( 0.000000000000000000, 0.000000000000000000, 1.000000000000000000 ) ) ;
#21608 = AXIS2_PLACEMENT_3D ( 'NONE', #27910, #2235, #28822 ) ;
#21609 = DIRECTION ( 'NONE',  ( -0.000000000000000000, -0.000000000000000000, 1.000000000000000000 ) ) ;
#21610 = ORIENTED_EDGE ( 'NONE', *, *, #12224, .F. ) ;
#21611 = DIRECTION ( 'NONE',  ( 0.000000000000000000, 0.000000000000000000, -1.000000000000000000 ) ) ;
#21612 = CARTESIAN_POINT ( 'NONE',  ( 0.000000000000000000, 0.000000000000000000, -0.3501037691048548561 ) ) ;
#21613 = ORIENTED_EDGE ( 'NONE', *, *, #31791, .F. ) ;
#21614 = EDGE_LOOP ( 'NONE', ( #16400, #34324, #3458, #7043 ) ) ;
#21615 = CYLINDRICAL_SURFACE ( 'NONE', #19313, 2.000000000000001776 ) ;
#21616 = DIRECTION ( 'NONE',  ( 0.000000000000000000, 0.000000000000000000, 1.000000000000000000 ) ) ;
#21617 = CARTESIAN_POINT ( 'NONE',  ( -106.0139510964988290, -39.63064057142699426, 32.49999999999999289 ) ) ;
#21618 = EDGE_LOOP ( 'NONE', ( #7865, #15037, #19078, #30523 ) ) ;
#21619 = VERTEX_POINT ( 'NONE', #26935 ) ;
#21620 = ORIENTED_EDGE ( 'NONE', *, *, #14498, .T. ) ;
#21621 = EDGE_CURVE ( 'NONE', #26836, #4724, #28472, .T. ) ;
#21622 = DIRECTION ( 'NONE',  ( -0.000000000000000000, -0.000000000000000000, 1.000000000000000000 ) ) ;
#21623 = EDGE_CURVE ( 'NONE', #32378, #18828, #25488, .T. ) ;
#21624 = ORIENTED_EDGE ( 'NONE', *, *, #20634, .F. ) ;
#21625 = ADVANCED_FACE ( 'NONE', ( #32375 ), #12667, .F. ) ;
#21626 = EDGE_LOOP ( 'NONE', ( #31017, #23759 ) ) ;
#21627 = LINE ( 'NONE', #32879, #23195 ) ;
#21628 = ORIENTED_EDGE ( 'NONE', *, *, #10435, .F. ) ;
#21629 = VERTEX_POINT ( 'NONE', #32543 ) ;
#21630 = DIRECTION ( 'NONE',  ( -0.000000000000000000, 0.000000000000000000, -1.000000000000000000 ) ) ;
#21631 = FACE_OUTER_BOUND ( 'NONE', #11092, .T. ) ;
#21632 = ORIENTED_EDGE ( 'NONE', *, *, #12735, .T. ) ;
#21633 = ORIENTED_EDGE ( 'NONE', *, *, #30612, .T. ) ;
#21634 = CYLINDRICAL_SURFACE ( 'NONE', #19692, 2.000000000000001776 ) ;
#21635 = CARTESIAN_POINT ( 'NONE',  ( -18.00000337463123046, 86.60254037844397601, -5.000000000000000000 ) ) ;
#21636 = CARTESIAN_POINT ( 'NONE',  ( 1.999996625368665182, 69.28203230275516944, 17.49999999999999645 ) ) ;
#21637 = CARTESIAN_POINT ( 'NONE',  ( 59.29837256189581041, 31.02796211690886707, -49.86561046011506448 ) ) ;
#21638 = EDGE_LOOP ( 'NONE', ( #15631, #1550, #16793, #21605, #16187, #5780 ) ) ;
#21639 = DIRECTION ( 'NONE',  ( 0.000000000000000000, 0.000000000000000000, -1.000000000000000000 ) ) ;
#21640 = ORIENTED_EDGE ( 'NONE', *, *, #11005, .T. ) ;
#21641 = DIRECTION ( 'NONE',  ( 0.000000000000000000, 0.4999999999999944489, -0.8660254037844418162 ) ) ;
#21642 = DIRECTION ( 'NONE',  ( 1.000000000000000000, 0.000000000000000000, 0.000000000000000000 ) ) ;
#21643 = DIRECTION ( 'NONE',  ( 0.000000000000000000, 0.000000000000000000, -1.000000000000000000 ) ) ;
#21644 = CARTESIAN_POINT ( 'NONE',  ( 59.13646009116148150, -70.47608876694609137, -49.22241343995298024 ) ) ;
#21645 = EDGE_CURVE ( 'NONE', #14355, #5803, #18303, .T. ) ;
#21646 = CARTESIAN_POINT ( 'NONE',  ( -67.00000337463104927, -43.30127018922202353, -9.999999999999998224 ) ) ;
#21647 = CYLINDRICAL_SURFACE ( 'NONE', #7748, 6.000000000000005329 ) ;
#21648 = DIRECTION ( 'NONE',  ( 0.000000000000000000, 0.000000000000000000, 1.000000000000000000 ) ) ;
#21649 = ORIENTED_EDGE ( 'NONE', *, *, #7559, .T. ) ;
#21650 = DIRECTION ( 'NONE',  ( 1.000000000000000000, 0.000000000000000000, 0.000000000000000000 ) ) ;
#21651 = CIRCLE ( 'NONE', #5485, 3.499999999999987566 ) ;
#21652 = CARTESIAN_POINT ( 'NONE',  ( 0.000000000000000000, -55.00000000000000000, -10.00000000000000000 ) ) ;
#21653 = DIRECTION ( 'NONE',  ( -1.000000000000000000, 0.000000000000000000, 0.000000000000000000 ) ) ;
#21654 = ORIENTED_EDGE ( 'NONE', *, *, #13092, .F. ) ;
#21655 = EDGE_CURVE ( 'NONE', #25696, #25394, #12894, .T. ) ;
#21656 = ORIENTED_EDGE ( 'NONE', *, *, #25903, .T. ) ;
#21657 = VERTEX_POINT ( 'NONE', #35753 ) ;
#21658 = FACE_OUTER_BOUND ( 'NONE', #33927, .T. ) ;
#21659 = DIRECTION ( 'NONE',  ( 0.000000000000000000, 0.000000000000000000, 1.000000000000000000 ) ) ;
#21660 = VERTEX_POINT ( 'NONE', #10064 ) ;
#21661 = DIRECTION ( 'NONE',  ( 1.000000000000000000, 0.000000000000000000, 0.000000000000000000 ) ) ;
#21662 = DIRECTION ( 'NONE',  ( 1.000000000000000000, 0.000000000000000000, 0.000000000000000000 ) ) ;
#21663 = ORIENTED_EDGE ( 'NONE', *, *, #35108, .T. ) ;
#21664 = ADVANCED_FACE ( 'NONE', ( #24505 ), #7425, .T. ) ;
#21665 = FACE_BOUND ( 'NONE', #24852, .T. ) ;
#21666 = VERTEX_POINT ( 'NONE', #7249 ) ;
#21667 = FACE_BOUND ( 'NONE', #33537, .T. ) ;
#21668 = CARTESIAN_POINT ( 'NONE',  ( -82.27241335952113843, 47.50000000000096634, 32.50002500000000083 ) ) ;
#21669 = DIRECTION ( 'NONE',  ( 0.000000000000000000, 0.000000000000000000, 1.000000000000000000 ) ) ;
#21670 = CARTESIAN_POINT ( 'NONE',  ( -31.02796211690907668, 59.29837256189569672, -49.86561046011506448 ) ) ;
#21671 = ORIENTED_EDGE ( 'NONE', *, *, #615, .F. ) ;
#21672 = DIRECTION ( 'NONE',  ( 0.7071067811865435759, -0.7071067811865514585, 0.000000000000000000 ) ) ;
#21673 = APPLICATION_PROTOCOL_DEFINITION ( 'draft international standard', 'automotive_design', 1998, #17085 ) ;
#21674 = CARTESIAN_POINT ( 'NONE',  ( -47.63139720814438505, -27.49999999999955591, -10.00000000000000178 ) ) ;
#21675 = DIRECTION ( 'NONE',  ( 1.000000000000000000, 0.000000000000000000, 0.000000000000000000 ) ) ;
#21676 = CYLINDRICAL_SURFACE ( 'NONE', #24580, 3.000000000000002665 ) ;
#21677 = DIRECTION ( 'NONE',  ( 0.000000000000000000, 0.000000000000000000, 1.000000000000000000 ) ) ;
#21678 = ADVANCED_FACE ( 'NONE', ( #18686, #4624 ), #35947, .T. ) ;
#21679 = ORIENTED_EDGE ( 'NONE', *, *, #4095, .F. ) ;
#21680 = CARTESIAN_POINT ( 'NONE',  ( -13.00000337463126066, 77.94228634059957983, -9.999999999999998224 ) ) ;
#21681 = FACE_OUTER_BOUND ( 'NONE', #12607, .T. ) ;
#21682 = CARTESIAN_POINT ( 'NONE',  ( 21.99999662536857770, 86.60254037844397601, 17.49999999999999645 ) ) ;
#21683 = ADVANCED_FACE ( 'NONE', ( #22601 ), #34054, .F. ) ;
#21684 = ORIENTED_EDGE ( 'NONE', *, *, #3027, .T. ) ;
#21685 = ORIENTED_EDGE ( 'NONE', *, *, #18987, .T. ) ;
#21686 = EDGE_CURVE ( 'NONE', #29469, #10997, #30852, .T. ) ;
#21687 = CARTESIAN_POINT ( 'NONE',  ( -36.97203788308986105, 58.48108235278859013, -49.86561046011506448 ) ) ;
#21688 = CARTESIAN_POINT ( 'NONE',  ( 17.99999662536861678, -86.60254037844400443, -9.999999999999998224 ) ) ;
#21689 = CARTESIAN_POINT ( 'NONE',  ( 84.99999662536832545, 25.98076211353319565, 12.50000000000000000 ) ) ;
#21690 = EDGE_CURVE ( 'NONE', #15799, #23723, #26067, .T. ) ;
#21691 = ORIENTED_EDGE ( 'NONE', *, *, #5790, .T. ) ;
#21692 = AXIS2_PLACEMENT_3D ( 'NONE', #22158, #32851, #10335 ) ;
#21693 = DIRECTION ( 'NONE',  ( -0.5000000000000094369, -0.8660254037844332675, 0.000000000000000000 ) ) ;
#21694 = DIRECTION ( 'NONE',  ( 1.000000000000000000, 0.000000000000000000, 0.000000000000000000 ) ) ;
#21695 = DIRECTION ( 'NONE',  ( -1.000000000000000000, 0.000000000000000000, 0.000000000000000000 ) ) ;
#21696 = DIRECTION ( 'NONE',  ( 1.000000000000000000, 0.000000000000000000, 0.000000000000000000 ) ) ;
#21697 = EDGE_LOOP ( 'NONE', ( #32169, #33647, #21366, #35494 ) ) ;
#21698 = VERTEX_POINT ( 'NONE', #5370 ) ;
#21699 = LINE ( 'NONE', #27131, #17711 ) ;
#21700 = DIRECTION ( 'NONE',  ( 1.000000000000000000, 0.000000000000000000, 0.000000000000000000 ) ) ;
#21701 = EDGE_LOOP ( 'NONE', ( #35624, #26346 ) ) ;
#21702 = EDGE_CURVE ( 'NONE', #5554, #28759, #28391, .T. ) ;
#21703 = PLANE ( 'NONE',  #28103 ) ;
#21704 = ORIENTED_EDGE ( 'NONE', *, *, #5784, .F. ) ;
#21705 = DIRECTION ( 'NONE',  ( 0.000000000000000000, -0.8660254037844388186, -0.4999999999999997224 ) ) ;
#21706 = AXIS2_PLACEMENT_3D ( 'NONE', #1916, #30418, #4747 ) ;
#21707 = DIRECTION ( 'NONE',  ( 0.000000000000000000, 0.000000000000000000, 1.000000000000000000 ) ) ;
#21708 = ORIENTED_EDGE ( 'NONE', *, *, #5444, .T. ) ;
#21709 = DIRECTION ( 'NONE',  ( 0.000000000000000000, 0.000000000000000000, -1.000000000000000000 ) ) ;
#21710 = VERTEX_POINT ( 'NONE', #16609 ) ;
#21711 = EDGE_CURVE ( 'NONE', #33530, #29480, #29644, .T. ) ;
#21712 = LINE ( 'NONE', #21155, #7474 ) ;
#21713 = AXIS2_PLACEMENT_3D ( 'NONE', #1724, #10718, #13712 ) ;
#21714 = FACE_OUTER_BOUND ( 'NONE', #30202, .T. ) ;
#21715 = CARTESIAN_POINT ( 'NONE',  ( 71.99999662536839651, -17.32050807568879947, -9.999999999999998224 ) ) ;
#21716 = EDGE_CURVE ( 'NONE', #31750, #11964, #33499, .T. ) ;
#21717 = EDGE_LOOP ( 'NONE', ( #24877, #10976, #2750, #19637, #19869, #29122, #36649, #28446, #11360, #11338, #23739, #10174, #19502, #7588, #32766, #35504, #36333, #33352, #22603, #9363, #9987, #5807, #22640, #31478 ) ) ;
#21718 = VECTOR ( 'NONE', #21268, 1000.000000000000000 ) ;
#21719 = LINE ( 'NONE', #36355, #35838 ) ;
#21720 = CARTESIAN_POINT ( 'NONE',  ( -106.2330357599457642, 40.32855561135241373, 32.50000000000000000 ) ) ;
#21721 = DIRECTION ( 'NONE',  ( -1.000000000000000000, 0.000000000000000000, 0.000000000000000000 ) ) ;
#21722 = ORIENTED_EDGE ( 'NONE', *, *, #6583, .F. ) ;
#21723 = VERTEX_POINT ( 'NONE', #19799 ) ;
#21724 = ORIENTED_EDGE ( 'NONE', *, *, #15929, .T. ) ;
#21725 = DIRECTION ( 'NONE',  ( -0.000000000000000000, -0.000000000000000000, 1.000000000000000000 ) ) ;
#21726 = VERTEX_POINT ( 'NONE', #19414 ) ;
#21727 = ADVANCED_FACE ( 'NONE', ( #4979 ), #1976, .F. ) ;
#21728 = CARTESIAN_POINT ( 'NONE',  ( 2.999996625368676728, -77.94228634059960825, 12.50000000000000000 ) ) ;
#21729 = DIRECTION ( 'NONE',  ( 0.8660254037844415942, 0.4999999999999949485, 0.000000000000000000 ) ) ;
#21730 = DIRECTION ( 'NONE',  ( 0.000000000000000000, 0.000000000000000000, 1.000000000000000000 ) ) ;
#21731 = AXIS2_PLACEMENT_3D ( 'NONE', #33003, #4321, #4703 ) ;
#21732 = CARTESIAN_POINT ( 'NONE',  ( 17.99999662536861678, -86.60254037844400443, 12.50000000000000000 ) ) ;
#21733 = ADVANCED_FACE ( 'NONE', ( #31040 ), #4816, .F. ) ;
#21734 = CARTESIAN_POINT ( 'NONE',  ( -149.8799519615616873, -5.999999999998430589, 27.50000000000000000 ) ) ;
#21735 = CARTESIAN_POINT ( 'NONE',  ( 77.99999662536832545, -17.32050807568879591, -5.000000000000000000 ) ) ;
#21736 = LINE ( 'NONE', #1133, #26176 ) ;
#21737 = LINE ( 'NONE', #30362, #16656 ) ;
#21738 = ORIENTED_EDGE ( 'NONE', *, *, #30281, .F. ) ;
#21739 = ORIENTED_EDGE ( 'NONE', *, *, #24800, .F. ) ;
#21740 = DIRECTION ( 'NONE',  ( 1.000000000000000000, 0.000000000000000000, 0.000000000000000000 ) ) ;
#21741 = CIRCLE ( 'NONE', #34917, 2.000000000000001776 ) ;
#21742 = DIRECTION ( 'NONE',  ( 1.000000000000000000, 0.000000000000000000, 0.000000000000000000 ) ) ;
#21743 = LINE ( 'NONE', #24586, #33022 ) ;
#21744 = CARTESIAN_POINT ( 'NONE',  ( -87.00000337463093558, -25.98076211353322051, -9.999999999999998224 ) ) ;
#21745 = VERTEX_POINT ( 'NONE', #36667 ) ;
#21746 = DIRECTION ( 'NONE',  ( -1.000000000000000000, 0.000000000000000000, 0.000000000000000000 ) ) ;
#21747 = LINE ( 'NONE', #36388, #12304 ) ;
#21748 = EDGE_CURVE ( 'NONE', #33109, #14753, #33297, .T. ) ;
#21749 = DIRECTION ( 'NONE',  ( 0.000000000000000000, 0.000000000000000000, 1.000000000000000000 ) ) ;
#21750 = ORIENTED_EDGE ( 'NONE', *, *, #15282, .T. ) ;
#21751 = CARTESIAN_POINT ( 'NONE',  ( 79.99999662536832545, -34.64101615137759183, -9.999999999999998224 ) ) ;
#21752 = AXIS2_PLACEMENT_3D ( 'NONE', #34768, #34581, #25582 ) ;
#21753 = ORIENTED_EDGE ( 'NONE', *, *, #36993, .T. ) ;
#21754 = CARTESIAN_POINT ( 'NONE',  ( 86.99999662536831124, -8.660254037844397956, -5.000000000000000000 ) ) ;
#21755 = EDGE_CURVE ( 'NONE', #9228, #23602, #14691, .T. ) ;
#21756 = FACE_OUTER_BOUND ( 'NONE', #17237, .T. ) ;
#21757 = CARTESIAN_POINT ( 'NONE',  ( 3.035766082959412415E-15, 5.773502691896260863, -2.080000000000000071 ) ) ;
#21758 = EDGE_CURVE ( 'NONE', #9216, #11639, #11685, .T. ) ;
#21759 = EDGE_LOOP ( 'NONE', ( #30312, #1187, #36169, #8642 ) ) ;
#21760 = VERTEX_POINT ( 'NONE', #14154 ) ;
#21761 = EDGE_CURVE ( 'NONE', #32044, #16751, #25608, .T. ) ;
#21762 = CIRCLE ( 'NONE', #31421, 6.726859516510129922 ) ;
#21763 = CARTESIAN_POINT ( 'NONE',  ( -68.00000337463102085, -34.64101615137762025, 17.49999999999999645 ) ) ;
#21764 = EDGE_LOOP ( 'NONE', ( #21237, #12034 ) ) ;
#21765 = CARTESIAN_POINT ( 'NONE',  ( 47.99999662536846756, -69.28203230275519786, 12.50000000000000000 ) ) ;
#21766 = AXIS2_PLACEMENT_3D ( 'NONE', #30253, #30802, #19578 ) ;
#21767 = DIRECTION ( 'NONE',  ( -1.000000000000000000, 0.000000000000000000, 0.000000000000000000 ) ) ;
#21768 = DIRECTION ( 'NONE',  ( 0.000000000000000000, 0.000000000000000000, -1.000000000000000000 ) ) ;
#21769 = DIRECTION ( 'NONE',  ( 0.000000000000000000, 0.000000000000000000, 1.000000000000000000 ) ) ;
#21770 = DIRECTION ( 'NONE',  ( 0.000000000000000000, -0.8660254037844418162, -0.4999999999999945044 ) ) ;
#21771 = ORIENTED_EDGE ( 'NONE', *, *, #12668, .T. ) ;
#21772 = CIRCLE ( 'NONE', #5606, 2.000000000000001776 ) ;
#21773 = CARTESIAN_POINT ( 'NONE',  ( -16.49657687835743403, 93.55673653615991725, 12.49999999999999822 ) ) ;
#21774 = DIRECTION ( 'NONE',  ( -1.000000000000000000, 0.000000000000000000, 0.000000000000000000 ) ) ;
#21775 = EDGE_CURVE ( 'NONE', #14243, #7403, #31219, .T. ) ;
#21776 = ORIENTED_EDGE ( 'NONE', *, *, #34579, .T. ) ;
#21777 = DIRECTION ( 'NONE',  ( 0.000000000000000000, 0.000000000000000000, 1.000000000000000000 ) ) ;
#21778 = FACE_BOUND ( 'NONE', #26220, .T. ) ;
#21779 = EDGE_LOOP ( 'NONE', ( #25435, #22790, #26538, #28489, #761 ) ) ;
#21780 = CONICAL_SURFACE ( 'NONE', #5615, 2.541999999999999815, 1.047197551196591858 ) ;
#21781 = VERTEX_POINT ( 'NONE', #16805 ) ;
#21782 = DIRECTION ( 'NONE',  ( 0.000000000000000000, 0.000000000000000000, 1.000000000000000000 ) ) ;
#21783 = CARTESIAN_POINT ( 'NONE',  ( 4.319324222803831326, -3.279739689143214232, -3.838711833381958538 ) ) ;
#21784 = CARTESIAN_POINT ( 'NONE',  ( -78.00000337463094979, -17.32050807568882078, -9.999999999999998224 ) ) ;
#21785 = ORIENTED_EDGE ( 'NONE', *, *, #10289, .F. ) ;
#21786 = ORIENTED_EDGE ( 'NONE', *, *, #13456, .F. ) ;
#21787 = EDGE_LOOP ( 'NONE', ( #31195, #10330 ) ) ;
#21788 = AXIS2_PLACEMENT_3D ( 'NONE', #21109, #15114, #12662 ) ;
#21789 = DIRECTION ( 'NONE',  ( -1.000000000000000000, 0.000000000000000000, 0.000000000000000000 ) ) ;
#21790 = EDGE_CURVE ( 'NONE', #36317, #7201, #3321, .T. ) ;
#21791 = CIRCLE ( 'NONE', #17581, 3.000000000000002665 ) ;
#21792 = ORIENTED_EDGE ( 'NONE', *, *, #35996, .F. ) ;
#21793 = EDGE_CURVE ( 'NONE', #27693, #5293, #32647, .T. ) ;
#21794 = CARTESIAN_POINT ( 'NONE',  ( -80.69570745083950669, 15.44540918807064500, 12.50000000000000000 ) ) ;
#21795 = ORIENTED_EDGE ( 'NONE', *, *, #20069, .F. ) ;
#21796 = ORIENTED_EDGE ( 'NONE', *, *, #4596, .T. ) ;
#21797 = EDGE_CURVE ( 'NONE', #35238, #8932, #13962, .T. ) ;
#21798 = DIRECTION ( 'NONE',  ( 0.000000000000000000, 0.000000000000000000, 1.000000000000000000 ) ) ;
#21799 = DIRECTION ( 'NONE',  ( 0.000000000000000000, -0.000000000000000000, 1.000000000000000000 ) ) ;
#21800 = EDGE_LOOP ( 'NONE', ( #11308, #19951 ) ) ;
#21801 = ORIENTED_EDGE ( 'NONE', *, *, #17143, .T. ) ;
#21802 = ADVANCED_FACE ( 'NONE', ( #11694 ), #14700, .F. ) ;
#21803 = DIRECTION ( 'NONE',  ( 0.000000000000000000, 0.000000000000000000, 1.000000000000000000 ) ) ;
#21804 = DIRECTION ( 'NONE',  ( -0.4999999999999979461, 0.8660254037844397068, 0.000000000000000000 ) ) ;
#21805 = CARTESIAN_POINT ( 'NONE',  ( 19.31922176934805435, 76.99660315353983719, -19.99999999999999645 ) ) ;
#21806 = DIRECTION ( 'NONE',  ( -0.000000000000000000, -0.000000000000000000, 1.000000000000000000 ) ) ;
#21807 = AXIS2_PLACEMENT_3D ( 'NONE', #18667, #21094, #36609 ) ;
#21808 = VERTEX_POINT ( 'NONE', #29325 ) ;
#21809 = FACE_OUTER_BOUND ( 'NONE', #17357, .T. ) ;
#21810 = ORIENTED_EDGE ( 'NONE', *, *, #28649, .F. ) ;
#21811 = CARTESIAN_POINT ( 'NONE',  ( 52.99999662536844625, 43.30127018922198801, -5.000000000000000000 ) ) ;
#21812 = DIRECTION ( 'NONE',  ( 0.7071067811865435759, -0.7071067811865514585, 0.000000000000000000 ) ) ;
#21813 = PLANE ( 'NONE',  #36975 ) ;
#21814 = CARTESIAN_POINT ( 'NONE',  ( 41.00000000000000000, 103.4105893997321743, 27.49999999999999645 ) ) ;
#21815 = ADVANCED_FACE ( 'NONE', ( #17515 ), #15079, .F. ) ;
#21816 = CYLINDRICAL_SURFACE ( 'NONE', #17064, 2.000000000000001776 ) ;
#21817 = AXIS2_PLACEMENT_3D ( 'NONE', #18961, #4519, #10158 ) ;
#21818 = EDGE_CURVE ( 'NONE', #34844, #9855, #36864, .T. ) ;
#21819 = FACE_OUTER_BOUND ( 'NONE', #19822, .T. ) ;
#21820 = ADVANCED_FACE ( 'NONE', ( #9076 ), #31761, .T. ) ;
#21821 = AXIS2_PLACEMENT_3D ( 'NONE', #2038, #7873, #30720 ) ;
#21822 = EDGE_CURVE ( 'NONE', #24921, #17786, #30272, .T. ) ;
#21823 = CARTESIAN_POINT ( 'NONE',  ( -2.448772250512182280E-15, 99.94802294027086020, 27.49999999999999645 ) ) ;
#21824 = ORIENTED_EDGE ( 'NONE', *, *, #19574, .F. ) ;
#21825 = DIRECTION ( 'NONE',  ( 1.000000000000000000, 0.000000000000000000, 0.000000000000000000 ) ) ;
#21826 = CARTESIAN_POINT ( 'NONE',  ( 3.000000000000000000, -2.935248768560059229, 3.469446951953614189E-15 ) ) ;
#21827 = CARTESIAN_POINT ( 'NONE',  ( 64.99999662536839651, -60.62177826491080168, -9.999999999999998224 ) ) ;
#21828 = VERTEX_POINT ( 'NONE', #12056 ) ;
#21829 = ORIENTED_EDGE ( 'NONE', *, *, #10349, .T. ) ;
#21830 = VERTEX_POINT ( 'NONE', #17898 ) ;
#21831 = AXIS2_PLACEMENT_3D ( 'NONE', #35861, #9777, #10175 ) ;
#21832 = CARTESIAN_POINT ( 'NONE',  ( 72.99999662536836809, 8.660254037844394404, -9.999999999999998224 ) ) ;
#21833 = CYLINDRICAL_SURFACE ( 'NONE', #10963, 2.000000000000001776 ) ;
#21834 = CIRCLE ( 'NONE', #27820, 2.000000000000001776 ) ;
#21835 = EDGE_LOOP ( 'NONE', ( #16347, #5422, #33495, #19488, #33021 ) ) ;
#21836 = AXIS2_PLACEMENT_3D ( 'NONE', #14281, #25890, #17283 ) ;
#21837 = DIRECTION ( 'NONE',  ( -1.000000000000000000, 0.000000000000000000, 0.000000000000000000 ) ) ;
#21838 = DIRECTION ( 'NONE',  ( 0.000000000000000000, 0.000000000000000000, 1.000000000000000000 ) ) ;
#21839 = ORIENTED_EDGE ( 'NONE', *, *, #9666, .T. ) ;
#21840 = FACE_BOUND ( 'NONE', #3700, .T. ) ;
#21841 = ORIENTED_EDGE ( 'NONE', *, *, #23999, .F. ) ;
#21842 = FACE_BOUND ( 'NONE', #3009, .T. ) ;
#21843 = ADVANCED_FACE ( 'NONE', ( #14899 ), #23151, .F. ) ;
#21844 = CIRCLE ( 'NONE', #26013, 3.500000000000003109 ) ;
#21845 = AXIS2_PLACEMENT_3D ( 'NONE', #26036, #17046, #17589 ) ;
#21846 = VECTOR ( 'NONE', #35387, 1000.000000000000000 ) ;
#21847 = DIRECTION ( 'NONE',  ( 0.000000000000000000, 0.000000000000000000, -1.000000000000000000 ) ) ;
#21848 = DIRECTION ( 'NONE',  ( 0.000000000000000000, 0.000000000000000000, 1.000000000000000000 ) ) ;
#21849 = AXIS2_PLACEMENT_3D ( 'NONE', #34604, #8904, #17516 ) ;
#21850 = CARTESIAN_POINT ( 'NONE',  ( -65.00000337463102085, 43.30127018922198801, -9.999999999999998224 ) ) ;
#21851 = ORIENTED_EDGE ( 'NONE', *, *, #7592, .T. ) ;
#21852 = CARTESIAN_POINT ( 'NONE',  ( 30.89873427475420442, -67.49533964939347186, 12.50000000000000000 ) ) ;
#21853 = APPLICATION_PROTOCOL_DEFINITION ( 'draft international standard', 'automotive_design', 1998, #1266 ) ;
#21854 = DIRECTION ( 'NONE',  ( -0.7071067811865382469, 0.000000000000000000, 0.7071067811865568986 ) ) ;
#21855 = CYLINDRICAL_SURFACE ( 'NONE', #19445, 3.500000000000003109 ) ;
#21856 = CIRCLE ( 'NONE', #6275, 2.000000000000001776 ) ;
#21857 = ORIENTED_EDGE ( 'NONE', *, *, #14837, .T. ) ;
#21858 = DIRECTION ( 'NONE',  ( 0.000000000000000000, 0.000000000000000000, 1.000000000000000000 ) ) ;
#21859 = CARTESIAN_POINT ( 'NONE',  ( 64.99999662536839651, 60.62177826491078747, 12.50000000000000000 ) ) ;
#21860 = VERTEX_POINT ( 'NONE', #3651 ) ;
#21861 = CARTESIAN_POINT ( 'NONE',  ( 0.000000000000000000, 2.935248768560057453, -3.903127820947815962E-15 ) ) ;
#21862 = VECTOR ( 'NONE', #9267, 1000.000000000000000 ) ;
#21863 = LINE ( 'NONE', #13244, #31014 ) ;
#21864 = DIRECTION ( 'NONE',  ( 0.000000000000000000, -0.000000000000000000, -1.000000000000000000 ) ) ;
#21865 =( GEOMETRIC_REPRESENTATION_CONTEXT ( 3 ) GLOBAL_UNCERTAINTY_ASSIGNED_CONTEXT ( ( #18590 ) ) GLOBAL_UNIT_ASSIGNED_CONTEXT ( ( #18939, #30567, #33745 ) ) REPRESENTATION_CONTEXT ( 'NONE', 'WORKASPACE' ) );
#21866 = ORIENTED_EDGE ( 'NONE', *, *, #11658, .T. ) ;
#21867 = EDGE_CURVE ( 'NONE', #1598, #19410, #22262, .T. ) ;
#21868 = ORIENTED_EDGE ( 'NONE', *, *, #3160, .F. ) ;
#21869 = PLANE ( 'NONE',  #3984 ) ;
#21870 = DIRECTION ( 'NONE',  ( -1.000000000000000000, 0.000000000000000000, 0.000000000000000000 ) ) ;
#21871 = CIRCLE ( 'NONE', #6878, 2.000000000000001776 ) ;
#21872 = DIRECTION ( 'NONE',  ( -0.8660254037844449249, -0.4999999999999888978, 0.000000000000000000 ) ) ;
#21873 = EDGE_LOOP ( 'NONE', ( #2030, #17156, #13405, #25964 ) ) ;
#21874 = VERTEX_POINT ( 'NONE', #31386 ) ;
#21875 = DIRECTION ( 'NONE',  ( 0.000000000000000000, 0.000000000000000000, 1.000000000000000000 ) ) ;
#21876 = CARTESIAN_POINT ( 'NONE',  ( -1.898848305348268983, 4.677202111653171457, -0.6020238742160447520 ) ) ;
#21877 = CARTESIAN_POINT ( 'NONE',  ( 0.000000000000000000, 101.4480229402710592, -24.99999999999999645 ) ) ;
#21878 = DIRECTION ( 'NONE',  ( 0.000000000000000000, 0.000000000000000000, 1.000000000000000000 ) ) ;
#21879 = ORIENTED_EDGE ( 'NONE', *, *, #12635, .T. ) ;
#21880 = ORIENTED_EDGE ( 'NONE', *, *, #31104, .T. ) ;
#21881 = CARTESIAN_POINT ( 'NONE',  ( 69.99999662536839651, 17.32050807568879236, -9.999999999999998224 ) ) ;
#21882 = AXIS2_PLACEMENT_3D ( 'NONE', #13236, #4060, #9856 ) ;
#21883 = DIRECTION ( 'NONE',  ( 0.000000000000000000, 0.000000000000000000, -1.000000000000000000 ) ) ;
#21884 = EDGE_LOOP ( 'NONE', ( #18612, #9561 ) ) ;
#21885 = CIRCLE ( 'NONE', #4524, 3.000000000000002665 ) ;
#21886 = CYLINDRICAL_SURFACE ( 'NONE', #2979, 2.000000000000001776 ) ;
#21887 = ORIENTED_EDGE ( 'NONE', *, *, #22710, .F. ) ;
#21888 = LINE ( 'NONE', #2011, #6338 ) ;
#21889 = EDGE_CURVE ( 'NONE', #13878, #32590, #26339, .T. ) ;
#21890 = AXIS2_PLACEMENT_3D ( 'NONE', #17629, #26276, #3402 ) ;
#21891 = AXIS2_PLACEMENT_3D ( 'NONE', #33536, #27871, #2007 ) ;
#21892 = ADVANCED_FACE ( 'NONE', ( #647 ), #20339, .F. ) ;
#21893 = AXIS2_PLACEMENT_3D ( 'NONE', #3488, #8920, #17531 ) ;
#21894 = CIRCLE ( 'NONE', #2550, 2.000000000000001776 ) ;
#21895 = CARTESIAN_POINT ( 'NONE',  ( -5.000000000000000000, 2.886751345948137981, -5.553418012614792509 ) ) ;
#21896 = ORIENTED_EDGE ( 'NONE', *, *, #29456, .F. ) ;
#21897 = EDGE_CURVE ( 'NONE', #17282, #12923, #22802, .T. ) ;
#21898 = CARTESIAN_POINT ( 'NONE',  ( 1.582370436567959393, 4.859920694386045348, -3.719399823475519895 ) ) ;
#21899 = VERTEX_POINT ( 'NONE', #28775 ) ;
#21900 =( LENGTH_UNIT ( ) NAMED_UNIT ( * ) SI_UNIT ( .MILLI., .METRE. ) );
#21901 = CIRCLE ( 'NONE', #16495, 2.000000000000001776 ) ;
#21902 = CARTESIAN_POINT ( 'NONE',  ( 79.99999662536832545, -34.64101615137759183, 12.50000000000000000 ) ) ;
#21903 = EDGE_CURVE ( 'NONE', #2842, #32102, #31246, .T. ) ;
#21904 = CARTESIAN_POINT ( 'NONE',  ( 47.63139720814400846, -27.50000000000022737, -5.000000000000000000 ) ) ;
#21905 = DIRECTION ( 'NONE',  ( 1.000000000000000000, 0.000000000000000000, 0.000000000000000000 ) ) ;
#21906 = VERTEX_POINT ( 'NONE', #6262 ) ;
#21907 = DIRECTION ( 'NONE',  ( 0.000000000000000000, 0.000000000000000000, 1.000000000000000000 ) ) ;
#21908 = CARTESIAN_POINT ( 'NONE',  ( 0.3000000000000016542, 5.755839955992559655E-16, -4.700000000000000178 ) ) ;
#21909 = DIRECTION ( 'NONE',  ( 0.000000000000000000, 0.000000000000000000, 1.000000000000000000 ) ) ;
#21910 = ORIENTED_EDGE ( 'NONE', *, *, #33894, .T. ) ;
#21911 = ORIENTED_EDGE ( 'NONE', *, *, #1391, .T. ) ;
#21912 = ORIENTED_EDGE ( 'NONE', *, *, #14885, .F. ) ;
#21913 = CIRCLE ( 'NONE', #1533, 2.000000000000000000 ) ;
#21914 = EDGE_CURVE ( 'NONE', #12792, #13768, #25962, .T. ) ;
#21915 = CARTESIAN_POINT ( 'NONE',  ( -124.4080600076929954, 12.15049814296761888, 27.50000000000000000 ) ) ;
#21916 = EDGE_LOOP ( 'NONE', ( #24184, #25221, #29864, #22863, #587 ) ) ;
#21917 = CARTESIAN_POINT ( 'NONE',  ( -45.00000337463111322, -77.94228634059960825, 12.50000000000000000 ) ) ;
#21918 = CARTESIAN_POINT ( 'NONE',  ( -55.00000337463110611, -43.30127018922202353, 17.49999999999999645 ) ) ;
#21919 = CIRCLE ( 'NONE', #17708, 2.000000000000001776 ) ;
#21920 = AXIS2_PLACEMENT_3D ( 'NONE', #12831, #1407, #20722 ) ;
#21921 = CIRCLE ( 'NONE', #3365, 2.000000000000000000 ) ;
#21922 = FACE_OUTER_BOUND ( 'NONE', #8461, .T. ) ;
#21923 = AXIS2_PLACEMENT_3D ( 'NONE', #2025, #34107, #13842 ) ;
#21924 = FACE_OUTER_BOUND ( 'NONE', #5862, .T. ) ;
#21925 = CARTESIAN_POINT ( 'NONE',  ( 35.19434990244975126, -52.39915983220758022, -4.999999999999997335 ) ) ;
#21926 = CARTESIAN_POINT ( 'NONE',  ( -101.6270506563345606, -63.51409607572428229, 32.50000000000000711 ) ) ;
#21927 = DIRECTION ( 'NONE',  ( 1.000000000000000000, 0.000000000000000000, 0.000000000000000000 ) ) ;
#21928 = CIRCLE ( 'NONE', #7554, 3.000000000000002665 ) ;
#21929 = DIRECTION ( 'NONE',  ( 0.000000000000000000, 0.000000000000000000, 1.000000000000000000 ) ) ;
#21930 = EDGE_LOOP ( 'NONE', ( #26496, #35517, #3352, #16644 ) ) ;
#21931 = VECTOR ( 'NONE', #35786, 1000.000000000000000 ) ;
#21932 = ORIENTED_EDGE ( 'NONE', *, *, #20401, .F. ) ;
#21933 = CARTESIAN_POINT ( 'NONE',  ( -43.00000337463111322, 77.94228634059959404, 17.49999999999999645 ) ) ;
#21934 = ADVANCED_FACE ( 'NONE', ( #29135 ), #5718, .F. ) ;
#21935 = CARTESIAN_POINT ( 'NONE',  ( 47.63139720814418610, 27.49999999999988987, -5.000000000000000000 ) ) ;
#21936 = DIRECTION ( 'NONE',  ( 0.000000000000000000, 0.000000000000000000, 1.000000000000000000 ) ) ;
#21937 = CARTESIAN_POINT ( 'NONE',  ( 52.99999662536844625, 60.62177826491077326, -9.999999999999998224 ) ) ;
#21938 = ORIENTED_EDGE ( 'NONE', *, *, #17262, .F. ) ;
#21939 = CARTESIAN_POINT ( 'NONE',  ( 0.000000000000000000, 0.000000000000000000, 27.50000000000000000 ) ) ;
#21940 = VECTOR ( 'NONE', #34507, 1000.000000000000000 ) ;
#21941 = CARTESIAN_POINT ( 'NONE',  ( 3.000000000000000000, 2.935248768560057453, -3.903127820947815962E-15 ) ) ;
#21942 = ORIENTED_EDGE ( 'NONE', *, *, #23634, .F. ) ;
#21943 = EDGE_CURVE ( 'NONE', #10270, #3670, #16274, .T. ) ;
#21944 = STYLED_ITEM ( 'NONE', ( #10458 ), #23302 ) ;
#21945 = CARTESIAN_POINT ( 'NONE',  ( 56.99999662536844625, -60.62177826491080168, -9.999999999999998224 ) ) ;
#21946 = VERTEX_POINT ( 'NONE', #34958 ) ;
#21947 = CIRCLE ( 'NONE', #4583, 30.00000000000000000 ) ;
#21948 = AXIS2_PLACEMENT_3D ( 'NONE', #21449, #33062, #18644 ) ;
#21949 = AXIS2_PLACEMENT_3D ( 'NONE', #1320, #3530, #15519 ) ;
#21950 = DIRECTION ( 'NONE',  ( 0.000000000000000000, 0.000000000000000000, 1.000000000000000000 ) ) ;
#21951 = AXIS2_PLACEMENT_3D ( 'NONE', #21612, #12402, #15617 ) ;
#21952 = DIRECTION ( 'NONE',  ( 0.000000000000000000, 0.000000000000000000, 1.000000000000000000 ) ) ;
#21953 = AXIS2_PLACEMENT_3D ( 'NONE', #15309, #1255, #21505 ) ;
#21954 = EDGE_CURVE ( 'NONE', #5770, #21147, #33043, .T. ) ;
#21955 = CARTESIAN_POINT ( 'NONE',  ( 0.000000000000000000, 0.000000000000000000, 15.00000000000000000 ) ) ;
#21956 = EDGE_LOOP ( 'NONE', ( #35383, #11099, #1982, #31826, #12042 ) ) ;
#21957 = EDGE_LOOP ( 'NONE', ( #22378, #11564, #29482, #15075 ) ) ;
#21958 = CIRCLE ( 'NONE', #10585, 3.499999999999991562 ) ;
#21959 = VERTEX_POINT ( 'NONE', #15642 ) ;
#21960 = CARTESIAN_POINT ( 'NONE',  ( -56.67878100130369035, 27.78182860042797131, 12.49999999999999822 ) ) ;
#21961 = DIRECTION ( 'NONE',  ( 0.000000000000000000, 0.000000000000000000, -1.000000000000000000 ) ) ;
#21962 = DIRECTION ( 'NONE',  ( 0.000000000000000000, 0.000000000000000000, 1.000000000000000000 ) ) ;
#21963 = CARTESIAN_POINT ( 'NONE',  ( 69.99999662536839651, 17.32050807568879236, -9.999999999999998224 ) ) ;
#21964 = CARTESIAN_POINT ( 'NONE',  ( -52.00000337463109190, 51.96152422706637708, -9.999999999999998224 ) ) ;
#21965 = ORIENTED_EDGE ( 'NONE', *, *, #28677, .T. ) ;
#21966 = DIRECTION ( 'NONE',  ( 0.000000000000000000, 0.000000000000000000, 1.000000000000000000 ) ) ;
#21967 = EDGE_CURVE ( 'NONE', #7306, #17105, #95, .T. ) ;
#21968 = FACE_OUTER_BOUND ( 'NONE', #24052, .T. ) ;
#21969 = CIRCLE ( 'NONE', #9970, 2.000000000000001776 ) ;
#21970 = CARTESIAN_POINT ( 'NONE',  ( 69.99999662536838230, -51.96152422706639840, -9.999999999999998224 ) ) ;
#21971 = ORIENTED_EDGE ( 'NONE', *, *, #607, .T. ) ;
#21972 = DIRECTION ( 'NONE',  ( -1.000000000000000000, 8.737866397512802015E-15, 0.000000000000000000 ) ) ;
#21973 = CARTESIAN_POINT ( 'NONE',  ( -75.00000337463097821, 43.30127018922197379, 12.50000000000000000 ) ) ;
#21974 = AXIS2_PLACEMENT_3D ( 'NONE', #16240, #30282, #23945 ) ;
#21975 = VERTEX_POINT ( 'NONE', #26892 ) ;
#21976 = EDGE_CURVE ( 'NONE', #8413, #31278, #1562, .T. ) ;
#21977 = CIRCLE ( 'NONE', #19600, 2.000000000000001776 ) ;
#21978 = ORIENTED_EDGE ( 'NONE', *, *, #21405, .T. ) ;
#21979 = AXIS2_PLACEMENT_3D ( 'NONE', #1941, #36637, #4778 ) ;
#21980 = EDGE_CURVE ( 'NONE', #27665, #1500, #21046, .T. ) ;
#21981 = CYLINDRICAL_SURFACE ( 'NONE', #29479, 2.000000000000001776 ) ;
#21982 = DIRECTION ( 'NONE',  ( -0.000000000000000000, -0.000000000000000000, -1.000000000000000000 ) ) ;
#21983 = CYLINDRICAL_SURFACE ( 'NONE', #27464, 3.500000000000003109 ) ;
#21984 = VERTEX_POINT ( 'NONE', #12438 ) ;
#21985 = ORIENTED_EDGE ( 'NONE', *, *, #11357, .T. ) ;
#21986 = ORIENTED_EDGE ( 'NONE', *, *, #24153, .T. ) ;
#21987 = VECTOR ( 'NONE', #8481, 1000.000000000000000 ) ;
#21988 = FACE_BOUND ( 'NONE', #3259, .T. ) ;
#21989 = VERTEX_POINT ( 'NONE', #18249 ) ;
#21990 = AXIS2_PLACEMENT_3D ( 'NONE', #31350, #28739, #34203 ) ;
#21991 = CYLINDRICAL_SURFACE ( 'NONE', #23779, 2.000000000000001776 ) ;
#21992 = ORIENTED_EDGE ( 'NONE', *, *, #17873, .T. ) ;
#21993 = AXIS2_PLACEMENT_3D ( 'NONE', #6562, #17799, #25875 ) ;
#21994 = VERTEX_POINT ( 'NONE', #23702 ) ;
#21995 = DIRECTION ( 'NONE',  ( 0.000000000000000000, 0.000000000000000000, 1.000000000000000000 ) ) ;
#21996 = EDGE_CURVE ( 'NONE', #6695, #21745, #702, .T. ) ;
#21997 = AXIS2_PLACEMENT_3D ( 'NONE', #27637, #27812, #4595 ) ;
#21998 = CARTESIAN_POINT ( 'NONE',  ( -38.00000337463113453, 69.28203230275516944, 17.49999999999999645 ) ) ;
#21999 = VERTEX_POINT ( 'NONE', #21636 ) ;
#22000 = ORIENTED_EDGE ( 'NONE', *, *, #16787, .T. ) ;
#22001 = CARTESIAN_POINT ( 'NONE',  ( 49.99999662536846756, 69.28203230275516944, 12.50000000000000000 ) ) ;
#22002 = CARTESIAN_POINT ( 'NONE',  ( 19.99999662536861678, -69.28203230275519786, -9.999999999999998224 ) ) ;
#22003 = AXIS2_PLACEMENT_3D ( 'NONE', #30826, #5162, #1969 ) ;
#22004 = AXIS2_PLACEMENT_3D ( 'NONE', #34842, #23409, #34471 ) ;
#22005 = CARTESIAN_POINT ( 'NONE',  ( 111.8061974404898962, 19.22934205794938478, 32.50000000000000000 ) ) ;
#22006 = CARTESIAN_POINT ( 'NONE',  ( -5.236872748402767286, 0.5081686017868760619, -4.057689166958444282 ) ) ;
#22007 = VECTOR ( 'NONE', #23512, 1000.000000000000000 ) ;
#22008 = ORIENTED_EDGE ( 'NONE', *, *, #27736, .T. ) ;
#22009 = DIRECTION ( 'NONE',  ( 0.000000000000000000, 0.000000000000000000, 1.000000000000000000 ) ) ;
#22010 = FACE_BOUND ( 'NONE', #13260, .T. ) ;
#22011 = DIRECTION ( 'NONE',  ( -1.000000000000000000, 0.000000000000000000, 0.000000000000000000 ) ) ;
#22012 = FACE_BOUND ( 'NONE', #355, .T. ) ;
#22013 = AXIS2_PLACEMENT_3D ( 'NONE', #14955, #31632, #12100 ) ;
#22014 = CARTESIAN_POINT ( 'NONE',  ( 24.99999662536859546, -77.94228634059960825, 12.50000000000000000 ) ) ;
#22015 = CARTESIAN_POINT ( 'NONE',  ( 14.99999662536863632, -77.94228634059960825, -9.999999999999998224 ) ) ;
#22016 = EDGE_CURVE ( 'NONE', #33332, #2655, #7893, .T. ) ;
#22017 = DIRECTION ( 'NONE',  ( -0.000000000000000000, -0.000000000000000000, 1.000000000000000000 ) ) ;
#22018 = VECTOR ( 'NONE', #3631, 1000.000000000000114 ) ;
#22019 = CARTESIAN_POINT ( 'NONE',  ( 3.000000000000000000, 2.935248768560057453, -3.903127820947815962E-15 ) ) ;
#22020 = ORIENTED_EDGE ( 'NONE', *, *, #21581, .F. ) ;
#22021 = EDGE_CURVE ( 'NONE', #9668, #30108, #10008, .T. ) ;
#22022 = CARTESIAN_POINT ( 'NONE',  ( -80.00000337463094979, -2.428612866367529932E-14, -5.000000000000000000 ) ) ;
#22023 = AXIS2_PLACEMENT_3D ( 'NONE', #670, #31783, #28964 ) ;
#22024 = CIRCLE ( 'NONE', #35820, 2.000000000000001776 ) ;
#22025 = CARTESIAN_POINT ( 'NONE',  ( -2.000003374631334818, 69.28203230275516944, 17.49999999999999645 ) ) ;
#22026 = LINE ( 'NONE', #19225, #33720 ) ;
#22027 = AXIS2_PLACEMENT_3D ( 'NONE', #14481, #28540, #31717 ) ;
#22028 = EDGE_LOOP ( 'NONE', ( #29119, #2652, #31844, #8631 ) ) ;
#22029 = ADVANCED_FACE ( 'NONE', ( #24250 ), #12230, .F. ) ;
#22030 = ORIENTED_EDGE ( 'NONE', *, *, #31399, .T. ) ;
#22031 = ORIENTED_EDGE ( 'NONE', *, *, #15370, .F. ) ;
#22032 = CIRCLE ( 'NONE', #2272, 27.00000000000001776 ) ;
#22033 = DIRECTION ( 'NONE',  ( 1.000000000000000000, 0.000000000000000000, 0.000000000000000000 ) ) ;
#22034 = CYLINDRICAL_SURFACE ( 'NONE', #15763, 2.000000000000001776 ) ;
#22035 = EDGE_CURVE ( 'NONE', #35263, #28024, #29884, .T. ) ;
#22036 = VERTEX_POINT ( 'NONE', #21250 ) ;
#22037 = EDGE_CURVE ( 'NONE', #2002, #13910, #21450, .T. ) ;
#22038 = CARTESIAN_POINT ( 'NONE',  ( -75.00000337463099243, -25.98076211353322051, -9.999999999999998224 ) ) ;
#22039 = CARTESIAN_POINT ( 'NONE',  ( 0.000000000000000000, 0.000000000000000000, -10.00000000000000000 ) ) ;
#22040 = ORIENTED_EDGE ( 'NONE', *, *, #31, .T. ) ;
#22041 = FACE_BOUND ( 'NONE', #2734, .T. ) ;
#22042 = ORIENTED_EDGE ( 'NONE', *, *, #35104, .F. ) ;
#22043 = FACE_BOUND ( 'NONE', #12012, .T. ) ;
#22044 = CIRCLE ( 'NONE', #8259, 150.0000000000000284 ) ;
#22045 = EDGE_CURVE ( 'NONE', #26530, #11321, #15814, .T. ) ;
#22046 = EDGE_CURVE ( 'NONE', #17563, #17956, #24457, .T. ) ;
#22047 = CARTESIAN_POINT ( 'NONE',  ( -70.00000337463102085, -51.96152422706641971, -5.000000000000000000 ) ) ;
#22048 = CARTESIAN_POINT ( 'NONE',  ( 4.378301941662549268, -3.528365556573306527, -4.190643565754943900 ) ) ;
#22049 = ADVANCED_FACE ( 'NONE', ( #27239 ), #14470, .F. ) ;
#22050 = AXIS2_PLACEMENT_3D ( 'NONE', #6045, #3767, #28728 ) ;
#22051 = ADVANCED_FACE ( 'NONE', ( #35357 ), #4383, .F. ) ;
#22052 = CYLINDRICAL_SURFACE ( 'NONE', #15800, 5.000000000000000000 ) ;
#22053 = ADVANCED_FACE ( 'NONE', ( #1376 ), #1207, .T. ) ;
#22054 = ORIENTED_EDGE ( 'NONE', *, *, #13309, .F. ) ;
#22055 = CARTESIAN_POINT ( 'NONE',  ( 25.30168577890723469, -79.91940132325416357, -5.000000000000000000 ) ) ;
#22056 = AXIS2_PLACEMENT_3D ( 'NONE', #32714, #29912, #9670 ) ;
#22057 = VECTOR ( 'NONE', #6365, 1000.000000000000000 ) ;
#22058 = ITEM_DEFINED_TRANSFORMATION ( 'NONE', 'NONE', #35119,  #21385 ) ;
#22059 = AXIS2_PLACEMENT_3D ( 'NONE', #20950, #3140, #32180 ) ;
#22060 = CARTESIAN_POINT ( 'NONE',  ( -30.00000337463118427, 69.28203230275516944, 17.49999999999999645 ) ) ;
#22061 = CARTESIAN_POINT ( 'NONE',  ( 124.4080600076931375, 12.15049814296589226, 27.50000000000000000 ) ) ;
#22062 = CIRCLE ( 'NONE', #15471, 2.000000000000001776 ) ;
#22063 = ORIENTED_EDGE ( 'NONE', *, *, #17378, .F. ) ;
#22064 = DIRECTION ( 'NONE',  ( 1.000000000000000000, 0.000000000000000000, 0.000000000000000000 ) ) ;
#22065 = CARTESIAN_POINT ( 'NONE',  ( 79.99999662536833966, 17.32050807568879236, 12.50000000000000000 ) ) ;
#22066 = ORIENTED_EDGE ( 'NONE', *, *, #20658, .T. ) ;
#22067 = CARTESIAN_POINT ( 'NONE',  ( 32.99999662536855283, 60.62177826491078747, 17.49999999999999645 ) ) ;
#22068 = CARTESIAN_POINT ( 'NONE',  ( -63.00000337463102085, 43.30127018922198801, 12.50000000000000000 ) ) ;
#22069 = CARTESIAN_POINT ( 'NONE',  ( 34.99999662536855283, -77.94228634059960825, -5.000000000000000000 ) ) ;
#22070 = VECTOR ( 'NONE', #1015, 1000.000000000000000 ) ;
#22071 = ORIENTED_EDGE ( 'NONE', *, *, #2366, .T. ) ;
#22072 = EDGE_LOOP ( 'NONE', ( #398, #12524 ) ) ;
#22073 = LINE ( 'NONE', #21687, #9977 ) ;
#22074 = TOROIDAL_SURFACE ( 'NONE', #23238, 4.700000000000000178, 0.2999999999999999889 ) ;
#22075 = CARTESIAN_POINT ( 'NONE',  ( -5.000000000000000888, 2.886751345948107783, -3.984345921091764886 ) ) ;
#22076 = CARTESIAN_POINT ( 'NONE',  ( -2.500000000000006217, -4.330127018922186544, 0.000000000000000000 ) ) ;
#22077 = VERTEX_POINT ( 'NONE', #18821 ) ;
#22078 = EDGE_LOOP ( 'NONE', ( #20839, #13547, #12151, #5389, #6423 ) ) ;
#22079 = VECTOR ( 'NONE', #28133, 1000.000000000000000 ) ;
#22080 = CARTESIAN_POINT ( 'NONE',  ( 37.50000000000000000, 103.4105893997321743, 18.49999999999999645 ) ) ;
#22081 = CARTESIAN_POINT ( 'NONE',  ( -0.1714266706912549731, 5.674529457426383594, -1.878862934774786275 ) ) ;
#22082 = CIRCLE ( 'NONE', #1084, 2.000000000000001776 ) ;
#22083 = DIRECTION ( 'NONE',  ( -1.000000000000000000, 0.000000000000000000, 0.000000000000000000 ) ) ;
#22084 = LINE ( 'NONE', #33528, #20376 ) ;
#22085 = ORIENTED_EDGE ( 'NONE', *, *, #30510, .F. ) ;
#22086 = ORIENTED_EDGE ( 'NONE', *, *, #1170, .F. ) ;
#22087 = CARTESIAN_POINT ( 'NONE',  ( 2.778182860043481472, 66.86787810013034061, -4.999999999999997335 ) ) ;
#22088 = AXIS2_PLACEMENT_3D ( 'NONE', #21567, #4314, #32996 ) ;
#22089 = FACE_OUTER_BOUND ( 'NONE', #28492, .T. ) ;
#22090 = ORIENTED_EDGE ( 'NONE', *, *, #25143, .T. ) ;
#22091 = ADVANCED_FACE ( 'NONE', ( #6813 ), #29680, .T. ) ;
#22092 = CARTESIAN_POINT ( 'NONE',  ( -0.7030283904595745481, -5.367609061417498495, -4.096693167834930982 ) ) ;
#22093 = EDGE_LOOP ( 'NONE', ( #2805, #19332 ) ) ;
#22094 = DIRECTION ( 'NONE',  ( 0.000000000000000000, 0.000000000000000000, 1.000000000000000000 ) ) ;
#22095 = CIRCLE ( 'NONE', #4133, 65.00000000000000000 ) ;
#22096 = CARTESIAN_POINT ( 'NONE',  ( -3.374631289687624047E-06, -69.28203230275519786, -9.999999999999998224 ) ) ;
#22097 = EDGE_CURVE ( 'NONE', #3118, #26973, #31810, .T. ) ;
#22098 = FACE_OUTER_BOUND ( 'NONE', #5515, .T. ) ;
#22099 = ORIENTED_EDGE ( 'NONE', *, *, #7074, .T. ) ;
#22100 = B_SPLINE_CURVE_WITH_KNOTS ( 'NONE', 3,
 ( #9194, #32047, #15392, #27382 ),
 .UNSPECIFIED., .F., .F.,
 ( 4, 4 ),
 ( 2.380735200807732181E-07, 0.002921158011986708155 ),
 .UNSPECIFIED. ) ;
#22101 = PRODUCT_DEFINITION_SHAPE ( 'NONE', 'NONE',  #37116 ) ;
#22102 = DIRECTION ( 'NONE',  ( 1.000000000000000000, 0.000000000000000000, 0.000000000000000000 ) ) ;
#22103 = AXIS2_PLACEMENT_3D ( 'NONE', #2583, #11009, #25454 ) ;
#22104 = DIRECTION ( 'NONE',  ( 1.000000000000000000, 0.000000000000000000, 0.000000000000000000 ) ) ;
#22105 = PLANE ( 'NONE',  #17923 ) ;
#22106 = ORIENTED_EDGE ( 'NONE', *, *, #27672, .F. ) ;
#22107 = CARTESIAN_POINT ( 'NONE',  ( 69.99999662536839651, 17.32050807568879236, -5.000000000000000000 ) ) ;
#22108 = CIRCLE ( 'NONE', #33489, 2.000000000000001776 ) ;
#22109 = DIRECTION ( 'NONE',  ( -0.000000000000000000, -0.000000000000000000, -1.000000000000000000 ) ) ;
#22110 = CARTESIAN_POINT ( 'NONE',  ( -48.00000337463109190, 69.28203230275518365, 12.50000000000000000 ) ) ;
#22111 = ORIENTED_EDGE ( 'NONE', *, *, #16808, .F. ) ;
#22112 = ORIENTED_EDGE ( 'NONE', *, *, #2638, .T. ) ;
#22113 = VECTOR ( 'NONE', #22219, 1000.000000000000000 ) ;
#22114 = CARTESIAN_POINT ( 'NONE',  ( 0.000000000000000000, 101.4480229402710734, 32.49999999999999289 ) ) ;
#22115 = ORIENTED_EDGE ( 'NONE', *, *, #31811, .F. ) ;
#22116 = DIRECTION ( 'NONE',  ( 0.000000000000000000, 0.000000000000000000, 1.000000000000000000 ) ) ;
#22117 = DIRECTION ( 'NONE',  ( -1.000000000000000000, 0.000000000000000000, 0.000000000000000000 ) ) ;
#22118 = AXIS2_PLACEMENT_3D ( 'NONE', #537, #4099, #11963 ) ;
#22119 = EDGE_CURVE ( 'NONE', #16067, #18894, #27634, .T. ) ;
#22120 = PLANE ( 'NONE',  #13226 ) ;
#22121 = VECTOR ( 'NONE', #16283, 1000.000000000000000 ) ;
#22122 = DIRECTION ( 'NONE',  ( 1.000000000000000000, 0.000000000000000000, 0.000000000000000000 ) ) ;
#22123 = AXIS2_PLACEMENT_3D ( 'NONE', #32511, #6826, #18262 ) ;
#22124 = CARTESIAN_POINT ( 'NONE',  ( 107.2801987736736180, -45.32358462409808197, 32.50000000000000711 ) ) ;
#22125 = DIRECTION ( 'NONE',  ( 0.000000000000000000, 0.000000000000000000, -1.000000000000000000 ) ) ;
#22126 = LINE ( 'NONE', #19676, #20209 ) ;
#22127 = CARTESIAN_POINT ( 'NONE',  ( 0.000000000000000000, 92.82302294027091705, 37.47964607176054130 ) ) ;
#22128 = ORIENTED_EDGE ( 'NONE', *, *, #28832, .T. ) ;
#22129 = ORIENTED_EDGE ( 'NONE', *, *, #6240, .F. ) ;
#22130 = AXIS2_PLACEMENT_3D ( 'NONE', #12941, #16329, #1889 ) ;
#22131 = DIRECTION ( 'NONE',  ( 0.000000000000000000, 0.000000000000000000, -1.000000000000000000 ) ) ;
#22132 = CIRCLE ( 'NONE', #25719, 2.000000000000001776 ) ;
#22133 = DIRECTION ( 'NONE',  ( 0.000000000000000000, 0.000000000000000000, 1.000000000000000000 ) ) ;
#22134 = CARTESIAN_POINT ( 'NONE',  ( 69.61830985333858735, 36.60425714729669977, 12.50000000000000000 ) ) ;
#22135 = DIRECTION ( 'NONE',  ( 0.000000000000000000, 0.000000000000000000, 1.000000000000000000 ) ) ;
#22136 = VERTEX_POINT ( 'NONE', #36449 ) ;
#22137 = B_SPLINE_CURVE_WITH_KNOTS ( 'NONE', 3,
 ( #19729, #28328, #11283, #8640, #22902, #14285 ),
 .UNSPECIFIED., .F., .F.,
 ( 4, 2, 4 ),
 ( -3.988673288088376993E-06, 0.0002483701411510744260, 0.0005007289555902372366 ),
 .UNSPECIFIED. ) ;
#22138 = DIRECTION ( 'NONE',  ( 1.000000000000000000, 0.000000000000000000, 0.000000000000000000 ) ) ;
#22139 = DIRECTION ( 'NONE',  ( 0.000000000000000000, 0.000000000000000000, 1.000000000000000000 ) ) ;
#22140 = ORIENTED_EDGE ( 'NONE', *, *, #26612, .F. ) ;
#22141 = EDGE_CURVE ( 'NONE', #28369, #7532, #16760, .T. ) ;
#22142 = FACE_OUTER_BOUND ( 'NONE', #26151, .T. ) ;
#22143 = ORIENTED_EDGE ( 'NONE', *, *, #14543, .T. ) ;
#22144 = AXIS2_PLACEMENT_3D ( 'NONE', #26964, #14979, #35031 ) ;
#22145 = CARTESIAN_POINT ( 'NONE',  ( 76.99999662536835388, -25.98076211353319565, 17.49999999999999645 ) ) ;
#22146 = FACE_OUTER_BOUND ( 'NONE', #1454, .T. ) ;
#22147 = AXIS2_PLACEMENT_3D ( 'NONE', #3093, #2361, #85 ) ;
#22148 = CARTESIAN_POINT ( 'NONE',  ( -88.00000337463090716, -1.040834085586084257E-14, -9.999999999999998224 ) ) ;
#22149 = ORIENTED_EDGE ( 'NONE', *, *, #9684, .F. ) ;
#22150 = VERTEX_POINT ( 'NONE', #10923 ) ;
#22151 = AXIS2_PLACEMENT_3D ( 'NONE', #13006, #18258, #33069 ) ;
#22152 = ORIENTED_EDGE ( 'NONE', *, *, #28430, .F. ) ;
#22153 = DIRECTION ( 'NONE',  ( 0.000000000000000000, 0.000000000000000000, 1.000000000000000000 ) ) ;
#22154 = EDGE_CURVE ( 'NONE', #20878, #18995, #9081, .T. ) ;
#22155 = DIRECTION ( 'NONE',  ( -0.000000000000000000, -0.000000000000000000, 1.000000000000000000 ) ) ;
#22156 = AXIS2_PLACEMENT_3D ( 'NONE', #19836, #22449, #19653 ) ;
#22157 = CARTESIAN_POINT ( 'NONE',  ( -62.00000337463108480, -51.96152422706641971, 17.49999999999999645 ) ) ;
#22158 = CARTESIAN_POINT ( 'NONE',  ( 52.39915983220795681, 35.19434990244919703, 12.49999999999999822 ) ) ;
#22159 = FACE_OUTER_BOUND ( 'NONE', #33357, .T. ) ;
#22160 = EDGE_CURVE ( 'NONE', #28884, #35505, #11103, .T. ) ;
#22161 = ORIENTED_EDGE ( 'NONE', *, *, #22187, .F. ) ;
#22162 = DIRECTION ( 'NONE',  ( 0.000000000000000000, 0.000000000000000000, 1.000000000000000000 ) ) ;
#22163 = CARTESIAN_POINT ( 'NONE',  ( -66.50936994187880202, 41.98909163213660634, 12.50000000000000000 ) ) ;
#22164 = DIRECTION ( 'NONE',  ( -1.000000000000000000, 0.000000000000000000, 0.000000000000000000 ) ) ;
#22165 = ORIENTED_EDGE ( 'NONE', *, *, #6465, .T. ) ;
#22166 = CARTESIAN_POINT ( 'NONE',  ( 4.279621169095998212, -62.97617850287780072, -4.999999999999997335 ) ) ;
#22167 = ADVANCED_FACE ( 'NONE', ( #27995, #27623 ), #13554, .F. ) ;
#22168 = CARTESIAN_POINT ( 'NONE',  ( -31.74999999999995737, 0.000000000000000000, 0.000000000000000000 ) ) ;
#22169 = AXIS2_PLACEMENT_3D ( 'NONE', #9240, #17339, #20489 ) ;
#22170 = ORIENTED_EDGE ( 'NONE', *, *, #27375, .T. ) ;
#22171 = ORIENTED_EDGE ( 'NONE', *, *, #8694, .T. ) ;
#22172 = EDGE_CURVE ( 'NONE', #15168, #19680, #9685, .T. ) ;
#22173 = CYLINDRICAL_SURFACE ( 'NONE', #22397, 5.000000000000000000 ) ;
#22174 = DIRECTION ( 'NONE',  ( -1.156482317317870344E-14, -1.000000000000000000, 0.000000000000000000 ) ) ;
#22175 = VECTOR ( 'NONE', #25380, 1000.000000000000000 ) ;
#22176 = CARTESIAN_POINT ( 'NONE',  ( -90.60231327712325822, -15.97563234535699017, 12.49999999999999822 ) ) ;
#22177 = CARTESIAN_POINT ( 'NONE',  ( 4.999999999999999112, -2.886751345948144198, -3.984345921091770659 ) ) ;
#22178 = ORIENTED_EDGE ( 'NONE', *, *, #32355, .F. ) ;
#22179 = ORIENTED_EDGE ( 'NONE', *, *, #25459, .T. ) ;
#22180 = CIRCLE ( 'NONE', #12574, 45.00000000000000711 ) ;
#22181 = CARTESIAN_POINT ( 'NONE',  ( 51.13139720814419320, 27.49999999999988987, -5.000000000000000888 ) ) ;
#22182 = CIRCLE ( 'NONE', #14387, 27.00000000000001421 ) ;
#22183 = ORIENTED_EDGE ( 'NONE', *, *, #35808, .F. ) ;
#22184 = FACE_OUTER_BOUND ( 'NONE', #4387, .T. ) ;
#22185 = ORIENTED_EDGE ( 'NONE', *, *, #15843, .F. ) ;
#22186 = VERTEX_POINT ( 'NONE', #7764 ) ;
#22187 = EDGE_CURVE ( 'NONE', #21959, #19593, #32417, .T. ) ;
#22188 = CARTESIAN_POINT ( 'NONE',  ( -23.00000337463120559, 77.94228634059957983, 12.50000000000000000 ) ) ;
#22189 = DIRECTION ( 'NONE',  ( 1.000000000000000000, 0.000000000000000000, -0.000000000000000000 ) ) ;
#22190 = ORIENTED_EDGE ( 'NONE', *, *, #35057, .T. ) ;
#22191 = ORIENTED_EDGE ( 'NONE', *, *, #18620, .T. ) ;
#22192 = PLANE ( 'NONE',  #31090 ) ;
#22193 = DIRECTION ( 'NONE',  ( -0.000000000000000000, -0.000000000000000000, -1.000000000000000000 ) ) ;
#22194 = EDGE_CURVE ( 'NONE', #9891, #3388, #30620, .T. ) ;
#22195 = DIRECTION ( 'NONE',  ( -1.000000000000000000, 0.000000000000000000, 0.000000000000000000 ) ) ;
#22196 = DIRECTION ( 'NONE',  ( 1.000000000000000000, 0.000000000000000000, 0.000000000000000000 ) ) ;
#22197 = ORIENTED_EDGE ( 'NONE', *, *, #33351, .T. ) ;
#22198 = CARTESIAN_POINT ( 'NONE',  ( -65.00000337463104927, -25.98076211353322051, -9.999999999999998224 ) ) ;
#22199 = EDGE_CURVE ( 'NONE', #14210, #9631, #19207, .T. ) ;
#22200 = CIRCLE ( 'NONE', #35967, 3.499999999999989342 ) ;
#22201 = FACE_BOUND ( 'NONE', #17793, .T. ) ;
#22202 = DIRECTION ( 'NONE',  ( 0.000000000000000000, 0.000000000000000000, -1.000000000000000000 ) ) ;
#22203 = DIRECTION ( 'NONE',  ( 1.000000000000000000, 0.000000000000000000, -0.000000000000000000 ) ) ;
#22204 = FACE_OUTER_BOUND ( 'NONE', #1046, .T. ) ;
#22205 = CARTESIAN_POINT ( 'NONE',  ( -15.00000337463126066, 77.94228634059957983, -9.999999999999998224 ) ) ;
#22206 = CARTESIAN_POINT ( 'NONE',  ( 34.99999662536855283, 60.62177826491078747, -9.999999999999998224 ) ) ;
#22207 = CARTESIAN_POINT ( 'NONE',  ( 47.99999662536848177, -51.96152422706640550, -9.999999999999998224 ) ) ;
#22208 = EDGE_LOOP ( 'NONE', ( #18056, #13888 ) ) ;
#22209 = LINE ( 'NONE', #18658, #26197 ) ;
#22210 = CARTESIAN_POINT ( 'NONE',  ( 6.000000000000000000, 0.000000000000000000, 0.000000000000000000 ) ) ;
#22211 = DIRECTION ( 'NONE',  ( 1.000000000000000000, 0.000000000000000000, 0.000000000000000000 ) ) ;
#22212 = VERTEX_POINT ( 'NONE', #13921 ) ;
#22213 = EDGE_LOOP ( 'NONE', ( #12550, #32256, #27212, #27772 ) ) ;
#22214 = VERTEX_POINT ( 'NONE', #7566 ) ;
#22215 = ADVANCED_FACE ( 'NONE', ( #22363 ), #30994, .F. ) ;
#22216 = CARTESIAN_POINT ( 'NONE',  ( 29.97040607558719572, -71.28181339061548272, 12.50000000000000000 ) ) ;
#22217 = CARTESIAN_POINT ( 'NONE',  ( 49.99999662536846756, 51.96152422706637708, -9.999999999999998224 ) ) ;
#22218 = ORIENTED_EDGE ( 'NONE', *, *, #30281, .T. ) ;
#22219 = DIRECTION ( 'NONE',  ( 0.000000000000000000, 0.000000000000000000, 1.000000000000000000 ) ) ;
#22220 = DIRECTION ( 'NONE',  ( 0.000000000000000000, 0.000000000000000000, 1.000000000000000000 ) ) ;
#22221 = EDGE_LOOP ( 'NONE', ( #24645, #14551, #17757, #4842, #1812, #24953, #35958, #6417, #32393, #25639, #4990, #8712 ) ) ;
#22222 = CIRCLE ( 'NONE', #35411, 27.00000000000001421 ) ;
#22223 = CARTESIAN_POINT ( 'NONE',  ( 54.99999662536844625, 43.30127018922198801, -9.999999999999998224 ) ) ;
#22224 = ORIENTED_EDGE ( 'NONE', *, *, #7338, .T. ) ;
#22225 = CARTESIAN_POINT ( 'NONE',  ( 19.99999662536857770, 86.60254037844397601, -9.999999999999998224 ) ) ;
#22226 = ADVANCED_FACE ( 'NONE', ( #8322 ), #5327, .F. ) ;
#22227 = DIRECTION ( 'NONE',  ( 0.000000000000000000, 0.000000000000000000, 1.000000000000000000 ) ) ;
#22228 = LINE ( 'NONE', #1605, #35326 ) ;
#22229 = EDGE_CURVE ( 'NONE', #15168, #16940, #13752, .T. ) ;
#22230 = VERTEX_POINT ( 'NONE', #31182 ) ;
#22231 = DIRECTION ( 'NONE',  ( -0.000000000000000000, -0.000000000000000000, -1.000000000000000000 ) ) ;
#22232 = EDGE_CURVE ( 'NONE', #1598, #27017, #16373, .T. ) ;
#22233 = CARTESIAN_POINT ( 'NONE',  ( 2.999996625368676728, -77.94228634059960825, -9.999999999999998224 ) ) ;
#22234 = CARTESIAN_POINT ( 'NONE',  ( -5.000003374631269537, -77.94228634059960825, -5.000000000000000000 ) ) ;
#22235 = VERTEX_POINT ( 'NONE', #27442 ) ;
#22236 = DIRECTION ( 'NONE',  ( 1.000000000000000000, 0.000000000000000000, 0.000000000000000000 ) ) ;
#22237 = CARTESIAN_POINT ( 'NONE',  ( -56.74224907228983739, 68.66839587347264739, 12.49999999999999645 ) ) ;
#22239 = VERTEX_POINT ( 'NONE', #4771 ) ;
#22238 = EDGE_CURVE ( 'NONE', #16919, #22507, #19016, .T. ) ;
#22240 = DIRECTION ( 'NONE',  ( 1.000000000000000000, 0.000000000000000000, 0.000000000000000000 ) ) ;
#22241 = EDGE_CURVE ( 'NONE', #31097, #17803, #34242, .T. ) ;
#22242 = AXIS2_PLACEMENT_3D ( 'NONE', #33380, #7694, #27923 ) ;
#22243 = DIRECTION ( 'NONE',  ( 0.000000000000000000, -0.000000000000000000, -1.000000000000000000 ) ) ;
#22244 = DIRECTION ( 'NONE',  ( 1.000000000000000000, 0.000000000000000000, 0.000000000000000000 ) ) ;
#22245 = DIRECTION ( 'NONE',  ( 0.000000000000000000, 0.000000000000000000, 1.000000000000000000 ) ) ;
#22246 = ORIENTED_EDGE ( 'NONE', *, *, #12132, .F. ) ;
#22247 = VERTEX_POINT ( 'NONE', #21805 ) ;
#22248 = CARTESIAN_POINT ( 'NONE',  ( 7.999996625368656744, -86.60254037844400443, -9.999999999999998224 ) ) ;
#22249 = CARTESIAN_POINT ( 'NONE',  ( 90.60231327712337190, 15.97563234535636134, -4.999999999999997335 ) ) ;
#22250 = EDGE_CURVE ( 'NONE', #1670, #22617, #10654, .T. ) ;
#22251 = ADVANCED_FACE ( 'NONE', ( #31344 ), #12015, .F. ) ;
#22252 = DIRECTION ( 'NONE',  ( -0.000000000000000000, -0.000000000000000000, 1.000000000000000000 ) ) ;
#22253 = ORIENTED_EDGE ( 'NONE', *, *, #33685, .F. ) ;
#22254 = EDGE_LOOP ( 'NONE', ( #6633, #21118, #96, #6020, #11010, #28363 ) ) ;
#22255 = EDGE_CURVE ( 'NONE', #34871, #30085, #28603, .T. ) ;
#22256 = LINE ( 'NONE', #13628, #7439 ) ;
#22257 = CARTESIAN_POINT ( 'NONE',  ( -0.7207917504152121513, 5.357353380764376283, -1.325189086772940117 ) ) ;
#22258 = DIRECTION ( 'NONE',  ( 0.000000000000000000, 0.000000000000000000, 1.000000000000000000 ) ) ;
#22259 = ORIENTED_EDGE ( 'NONE', *, *, #11263, .T. ) ;
#22260 = ORIENTED_EDGE ( 'NONE', *, *, #36629, .T. ) ;
#22261 = DIRECTION ( 'NONE',  ( -1.000000000000000000, 0.000000000000000000, 0.000000000000000000 ) ) ;
#22262 = CIRCLE ( 'NONE', #13873, 6.000000000000005329 ) ;
#22263 = DIRECTION ( 'NONE',  ( 1.000000000000000000, 0.000000000000000000, 0.000000000000000000 ) ) ;
#22264 = EDGE_LOOP ( 'NONE', ( #10486, #20229, #21750, #10847 ) ) ;
#22265 = CARTESIAN_POINT ( 'NONE',  ( -31.83425564451526668, -89.42901512340343118, -49.86348611802629449 ) ) ;
#22266 = ORIENTED_EDGE ( 'NONE', *, *, #28320, .T. ) ;
#22267 = TOROIDAL_SURFACE ( 'NONE', #15684, 6.532899837730827386, 0.5671001622691684840 ) ;
#22268 = FACE_BOUND ( 'NONE', #22664, .T. ) ;
#22269 = EDGE_CURVE ( 'NONE', #20675, #21723, #25038, .T. ) ;
#22270 = FACE_OUTER_BOUND ( 'NONE', #7297, .T. ) ;
#22271 = ADVANCED_FACE ( 'NONE', ( #28349 ), #2243, .T. ) ;
#22272 = CARTESIAN_POINT ( 'NONE',  ( 4.400655246573196955, 3.515428273944452453, -4.176900509772112358 ) ) ;
#22273 = EDGE_LOOP ( 'NONE', ( #1274, #36221, #34623, #16699 ) ) ;
#22274 = DIRECTION ( 'NONE',  ( 0.5718436470691531381, -0.8203626291504566570, 0.000000000000000000 ) ) ;
#22275 = CARTESIAN_POINT ( 'NONE',  ( 74.99999662536836809, 8.660254037844394404, -9.999999999999998224 ) ) ;
#22276 = CARTESIAN_POINT ( 'NONE',  ( 37.50000000000000000, -103.4105893997321743, 32.50000000000000000 ) ) ;
#22277 = FACE_OUTER_BOUND ( 'NONE', #3603, .T. ) ;
#22278 = VERTEX_POINT ( 'NONE', #34549 ) ;
#22279 = DIRECTION ( 'NONE',  ( 0.000000000000000000, 0.000000000000000000, 1.000000000000000000 ) ) ;
#22280 = EDGE_CURVE ( 'NONE', #36878, #18695, #3450, .T. ) ;
#22281 = FACE_OUTER_BOUND ( 'NONE', #12883, .T. ) ;
#22282 = CARTESIAN_POINT ( 'NONE',  ( 106.7731239591682026, -98.28784258493068648, 27.50000000000000000 ) ) ;
#22283 = EDGE_LOOP ( 'NONE', ( #22633, #29550, #25136, #27615 ) ) ;
#22284 = ORIENTED_EDGE ( 'NONE', *, *, #20746, .T. ) ;
#22285 = AXIS2_PLACEMENT_3D ( 'NONE', #35110, #24040, #9774 ) ;
#22286 = CARTESIAN_POINT ( 'NONE',  ( 42.99999662536850309, -60.62177826491080168, -5.000000000000000000 ) ) ;
#22287 = ORIENTED_EDGE ( 'NONE', *, *, #28480, .T. ) ;
#22288 = DIRECTION ( 'NONE',  ( 0.000000000000000000, 0.000000000000000000, 1.000000000000000000 ) ) ;
#22289 = DIRECTION ( 'NONE',  ( -0.000000000000000000, -0.000000000000000000, 1.000000000000000000 ) ) ;
#22290 = EDGE_CURVE ( 'NONE', #34086, #14414, #23819, .T. ) ;
#22291 = EDGE_CURVE ( 'NONE', #8626, #18158, #7034, .T. ) ;
#22292 = DIRECTION ( 'NONE',  ( 1.000000000000000000, 0.000000000000000000, 0.000000000000000000 ) ) ;
#22293 = ADVANCED_FACE ( 'NONE', ( #3416 ), #11838, .F. ) ;
#22294 = EDGE_CURVE ( 'NONE', #9342, #26254, #49, .T. ) ;
#22295 = DIRECTION ( 'NONE',  ( 1.000000000000000000, 0.000000000000000000, 0.000000000000000000 ) ) ;
#22296 = CARTESIAN_POINT ( 'NONE',  ( 102.6344492401623398, -62.23201224809161403, 32.50000000000000711 ) ) ;
#22297 = CARTESIAN_POINT ( 'NONE',  ( -86.97174780077182277, -72.12318266404240319, 32.49999999999999289 ) ) ;
#22298 = DIRECTION ( 'NONE',  ( -0.000000000000000000, -0.000000000000000000, 1.000000000000000000 ) ) ;
#22299 = DIRECTION ( 'NONE',  ( -1.000000000000000000, -0.000000000000000000, -0.000000000000000000 ) ) ;
#22300 = ORIENTED_EDGE ( 'NONE', *, *, #35780, .T. ) ;
#22301 = VERTEX_POINT ( 'NONE', #36999 ) ;
#22302 = VECTOR ( 'NONE', #29270, 1000.000000000000000 ) ;
#22303 = CIRCLE ( 'NONE', #27695, 3.500000000000003109 ) ;
#22304 = CARTESIAN_POINT ( 'NONE',  ( 67.99999662536838230, -3.224517592124143893E-15, -9.999999999999998224 ) ) ;
#22305 = FACE_OUTER_BOUND ( 'NONE', #33114, .T. ) ;
#22306 = CARTESIAN_POINT ( 'NONE',  ( -39.27785635698568711, -86.50000000000001421, 27.50000000000000000 ) ) ;
#22307 = LINE ( 'NONE', #33749, #6529 ) ;
#22308 = VERTEX_POINT ( 'NONE', #23098 ) ;
#22309 = PRODUCT_DEFINITION_CONTEXT ( 'detailed design', #4893, 'design' ) ;
#22310 = FACE_OUTER_BOUND ( 'NONE', #19344, .T. ) ;
#22311 = ORIENTED_EDGE ( 'NONE', *, *, #21249, .F. ) ;
#22312 = CIRCLE ( 'NONE', #6138, 0.5671001622691687061 ) ;
#22313 = ORIENTED_EDGE ( 'NONE', *, *, #33172, .T. ) ;
#22314 = DIRECTION ( 'NONE',  ( 0.000000000000000000, 0.000000000000000000, 1.000000000000000000 ) ) ;
#22315 = EDGE_LOOP ( 'NONE', ( #5866, #2250 ) ) ;
#22316 = EDGE_CURVE ( 'NONE', #11237, #29382, #9208, .T. ) ;
#22317 = LINE ( 'NONE', #13871, #34565 ) ;
#22318 = CARTESIAN_POINT ( 'NONE',  ( 32.99999662536855283, -77.94228634059960825, 12.50000000000000000 ) ) ;
#22319 = DIRECTION ( 'NONE',  ( 1.000000000000000000, 0.000000000000000000, 0.000000000000000000 ) ) ;
#22320 = ORIENTED_EDGE ( 'NONE', *, *, #34214, .F. ) ;
#22321 = ORIENTED_EDGE ( 'NONE', *, *, #3932, .T. ) ;
#22322 = EDGE_LOOP ( 'NONE', ( #14604, #6438 ) ) ;
#22323 = CIRCLE ( 'NONE', #6761, 33.00000000000002132 ) ;
#22324 = ORIENTED_EDGE ( 'NONE', *, *, #13487, .F. ) ;
#22325 = CARTESIAN_POINT ( 'NONE',  ( 74.99999662536836809, -8.660254037844401509, 12.50000000000000000 ) ) ;
#22326 = DIRECTION ( 'NONE',  ( 1.000000000000000000, 0.000000000000000000, 0.000000000000000000 ) ) ;
#22327 = DIRECTION ( 'NONE',  ( 0.000000000000000000, 0.000000000000000000, 1.000000000000000000 ) ) ;
#22328 = CYLINDRICAL_SURFACE ( 'NONE', #24107, 2.000000000000000000 ) ;
#22329 = DIRECTION ( 'NONE',  ( 0.000000000000000000, 0.000000000000000000, 1.000000000000000000 ) ) ;
#22330 = ORIENTED_EDGE ( 'NONE', *, *, #8848, .F. ) ;
#22331 = DIRECTION ( 'NONE',  ( 0.000000000000000000, 0.000000000000000000, 1.000000000000000000 ) ) ;
#22332 = DIRECTION ( 'NONE',  ( -1.000000000000000000, 0.000000000000000000, 0.000000000000000000 ) ) ;
#22333 = VECTOR ( 'NONE', #22666, 1000.000000000000000 ) ;
#22334 = ADVANCED_FACE ( 'NONE', ( #25756 ), #17306, .F. ) ;
#22335 = DIRECTION ( 'NONE',  ( 1.000000000000000000, 0.000000000000000000, 0.000000000000000000 ) ) ;
#22336 = EDGE_LOOP ( 'NONE', ( #21034, #35446, #30425, #3177 ) ) ;
#22337 = VECTOR ( 'NONE', #21089, 1000.000000000000000 ) ;
#22338 = CYLINDRICAL_SURFACE ( 'NONE', #20836, 2.000000000000001776 ) ;
#22339 = CYLINDRICAL_SURFACE ( 'NONE', #17163, 27.00000000000001421 ) ;
#22340 = ORIENTED_EDGE ( 'NONE', *, *, #36814, .F. ) ;
#22341 = VERTEX_POINT ( 'NONE', #16923 ) ;
#22342 = PLANE ( 'NONE',  #4445 ) ;
#22343 = CARTESIAN_POINT ( 'NONE',  ( 0.1702248550645280023, 5.871782057790544407, -4.289066185948687604 ) ) ;
#22344 = DIRECTION ( 'NONE',  ( 1.000000000000000000, 0.000000000000000000, 0.000000000000000000 ) ) ;
#22345 = CARTESIAN_POINT ( 'NONE',  ( 47.63139720814400846, -27.50000000000022737, -15.00000000000000000 ) ) ;
#22346 = ORIENTED_EDGE ( 'NONE', *, *, #8957, .T. ) ;
#22347 = ORIENTED_EDGE ( 'NONE', *, *, #486, .T. ) ;
#22348 = FACE_BOUND ( 'NONE', #21158, .T. ) ;
#22349 = CIRCLE ( 'NONE', #14574, 3.000000000000002665 ) ;
#22350 = VERTEX_POINT ( 'NONE', #14102 ) ;
#22351 = LINE ( 'NONE', #19907, #2823 ) ;
#22352 = VERTEX_POINT ( 'NONE', #9036 ) ;
#22353 = EDGE_CURVE ( 'NONE', #20996, #20810, #4665, .T. ) ;
#22354 = ORIENTED_EDGE ( 'NONE', *, *, #25844, .T. ) ;
#22355 = DIRECTION ( 'NONE',  ( -1.000000000000000000, 0.000000000000000000, 0.000000000000000000 ) ) ;
#22356 = CIRCLE ( 'NONE', #11554, 2.000000000000001776 ) ;
#22357 = DIRECTION ( 'NONE',  ( 1.000000000000000000, 0.000000000000000000, 0.000000000000000000 ) ) ;
#22358 = EDGE_LOOP ( 'NONE', ( #283, #15161, #13875, #22775, #21724 ) ) ;
#22359 = PRODUCT_DEFINITION ( 'UNKNOWN', '', #26759, #5055 ) ;
#22360 = ORIENTED_EDGE ( 'NONE', *, *, #15790, .F. ) ;
#22361 = CYLINDRICAL_SURFACE ( 'NONE', #35896, 2.000000000000001776 ) ;
#22362 = DIRECTION ( 'NONE',  ( 0.000000000000000000, 0.000000000000000000, 1.000000000000000000 ) ) ;
#22363 = FACE_OUTER_BOUND ( 'NONE', #13109, .T. ) ;
#22364 = CARTESIAN_POINT ( 'NONE',  ( -101.7384897088158766, -110.2237710830526112, 27.50000000000000000 ) ) ;
#22365 = EDGE_CURVE ( 'NONE', #31133, #15574, #11801, .T. ) ;
#22366 = VERTEX_POINT ( 'NONE', #8491 ) ;
#22367 = FACE_OUTER_BOUND ( 'NONE', #26312, .T. ) ;
#22368 = FACE_BOUND ( 'NONE', #9667, .T. ) ;
#22369 = DIRECTION ( 'NONE',  ( -1.000000000000000000, 0.000000000000000000, 0.000000000000000000 ) ) ;
#22370 = CIRCLE ( 'NONE', #28939, 2.000000000000001776 ) ;
#22371 = DIRECTION ( 'NONE',  ( 0.000000000000000000, 0.000000000000000000, 1.000000000000000000 ) ) ;
#22372 = CARTESIAN_POINT ( 'NONE',  ( -22.00000337463124112, -69.28203230275522628, -9.999999999999998224 ) ) ;
#22373 = DIRECTION ( 'NONE',  ( 1.000000000000000000, 0.000000000000000000, 0.000000000000000000 ) ) ;
#22374 = VECTOR ( 'NONE', #3534, 1000.000000000000000 ) ;
#22375 = CARTESIAN_POINT ( 'NONE',  ( 69.99999662536839651, -17.32050807568879947, -5.000000000000000000 ) ) ;
#22376 = EDGE_CURVE ( 'NONE', #14128, #575, #23201, .T. ) ;
#22377 = DIRECTION ( 'NONE',  ( 0.000000000000000000, 0.000000000000000000, 1.000000000000000000 ) ) ;
#22378 = ORIENTED_EDGE ( 'NONE', *, *, #31754, .F. ) ;
#22379 = CARTESIAN_POINT ( 'NONE',  ( -56.67878100130369035, 27.78182860042797131, -4.999999999999997335 ) ) ;
#22380 = DIRECTION ( 'NONE',  ( 1.000000000000000000, 0.000000000000000000, 0.000000000000000000 ) ) ;
#22381 = CARTESIAN_POINT ( 'NONE',  ( -55.00000337463110611, -43.30127018922202353, -9.999999999999998224 ) ) ;
#22382 = AXIS2_PLACEMENT_3D ( 'NONE', #29926, #4251, #13399 ) ;
#22383 = ORIENTED_EDGE ( 'NONE', *, *, #3892, .F. ) ;
#22384 = VERTEX_POINT ( 'NONE', #31881 ) ;
#22385 = ORIENTED_EDGE ( 'NONE', *, *, #36666, .F. ) ;
#22386 = AXIS2_PLACEMENT_3D ( 'NONE', #23870, #35318, #9615 ) ;
#22387 = DIRECTION ( 'NONE',  ( 0.000000000000000000, 0.4999999999999951150, -0.8660254037844414832 ) ) ;
#22388 = CARTESIAN_POINT ( 'NONE',  ( 30.89873427475420442, -67.49533964939347186, -5.000000000000000000 ) ) ;
#22389 = VERTEX_POINT ( 'NONE', #6215 ) ;
#22390 = EDGE_CURVE ( 'NONE', #15915, #25880, #16035, .T. ) ;
#22391 = CYLINDRICAL_SURFACE ( 'NONE', #35902, 3.500000000000003109 ) ;
#22392 = ORIENTED_EDGE ( 'NONE', *, *, #23310, .T. ) ;
#22393 = EDGE_CURVE ( 'NONE', #32118, #3085, #13022, .T. ) ;
#22394 = DIRECTION ( 'NONE',  ( -0.000000000000000000, -0.000000000000000000, 1.000000000000000000 ) ) ;
#22395 = EDGE_LOOP ( 'NONE', ( #5027, #12708 ) ) ;
#22396 = DIRECTION ( 'NONE',  ( 1.000000000000000000, 0.000000000000000000, 0.000000000000000000 ) ) ;
#22397 = AXIS2_PLACEMENT_3D ( 'NONE', #1232, #16536, #18095 ) ;
#22398 = CARTESIAN_POINT ( 'NONE',  ( 76.99999662536836809, 43.30127018922198801, -9.999999999999998224 ) ) ;
#22399 = CARTESIAN_POINT ( 'NONE',  ( 2.999996625368645198, 77.94228634059957983, 17.49999999999999645 ) ) ;
#22400 = EDGE_CURVE ( 'NONE', #10468, #4318, #32778, .T. ) ;
#22401 = ORIENTED_EDGE ( 'NONE', *, *, #27682, .F. ) ;
#22402 = DIRECTION ( 'NONE',  ( -1.000000000000000000, 0.000000000000000000, 0.000000000000000000 ) ) ;
#22403 = AXIS2_PLACEMENT_3D ( 'NONE', #36031, #21952, #10321 ) ;
#22404 = DIRECTION ( 'NONE',  ( -1.000000000000000000, 0.000000000000000000, 0.000000000000000000 ) ) ;
#22405 = CARTESIAN_POINT ( 'NONE',  ( -124.4080600076929954, 12.15049814296761888, 32.50002500000000083 ) ) ;
#22406 = EDGE_CURVE ( 'NONE', #12950, #36279, #30393, .T. ) ;
#22407 = VERTEX_POINT ( 'NONE', #18029 ) ;
#22408 = AXIS2_PLACEMENT_3D ( 'NONE', #34885, #24179, #15372 ) ;
#22409 = CARTESIAN_POINT ( 'NONE',  ( -35.00000337463116296, 77.94228634059957983, 12.50000000000000000 ) ) ;
#22410 = FACE_OUTER_BOUND ( 'NONE', #9490, .T. ) ;
#22411 = ORIENTED_EDGE ( 'NONE', *, *, #28274, .T. ) ;
#22412 = DIRECTION ( 'NONE',  ( 0.000000000000000000, 0.000000000000000000, -1.000000000000000000 ) ) ;
#22413 = DIRECTION ( 'NONE',  ( -1.000000000000000000, -0.000000000000000000, -0.000000000000000000 ) ) ;
#22414 = CARTESIAN_POINT ( 'NONE',  ( -69.61831313460106685, -36.60425647305652319, 12.50000000000000000 ) ) ;
#22415 = DIRECTION ( 'NONE',  ( 0.000000000000000000, 0.000000000000000000, 1.000000000000000000 ) ) ;
#22416 = ORIENTED_EDGE ( 'NONE', *, *, #17665, .F. ) ;
#22417 = VERTEX_POINT ( 'NONE', #24357 ) ;
#22418 = AXIS2_PLACEMENT_3D ( 'NONE', #35619, #22245, #21166 ) ;
#22419 = CYLINDRICAL_SURFACE ( 'NONE', #385, 3.500000000000003109 ) ;
#22420 = DIRECTION ( 'NONE',  ( 0.000000000000000000, 0.000000000000000000, 1.000000000000000000 ) ) ;
#22421 = CIRCLE ( 'NONE', #31408, 2.000000000000001776 ) ;
#22422 = ADVANCED_FACE ( 'NONE', ( #4477 ), #1465, .F. ) ;
#22423 = ORIENTED_EDGE ( 'NONE', *, *, #14558, .T. ) ;
#22424 = VERTEX_POINT ( 'NONE', #10666 ) ;
#22425 = CARTESIAN_POINT ( 'NONE',  ( 11.99999662536862566, 86.60254037844397601, -9.999999999999998224 ) ) ;
#22426 = DIRECTION ( 'NONE',  ( -1.000000000000000000, 0.000000000000000000, 0.000000000000000000 ) ) ;
#22427 = DIRECTION ( 'NONE',  ( 0.000000000000000000, 0.000000000000000000, 1.000000000000000000 ) ) ;
#22428 = ORIENTED_EDGE ( 'NONE', *, *, #19101, .T. ) ;
#22429 = CIRCLE ( 'NONE', #6261, 2.000000000000001776 ) ;
#22430 = EDGE_CURVE ( 'NONE', #30579, #29460, #27346, .T. ) ;
#22431 = AXIS2_PLACEMENT_3D ( 'NONE', #11424, #17785, #23593 ) ;
#22432 = ORIENTED_EDGE ( 'NONE', *, *, #36460, .F. ) ;
#22433 = DIRECTION ( 'NONE',  ( -1.000000000000000000, 0.000000000000000000, 0.000000000000000000 ) ) ;
#22434 = AXIS2_PLACEMENT_3D ( 'NONE', #22405, #27664, #1613 ) ;
#22435 = DIRECTION ( 'NONE',  ( 0.000000000000000000, 0.000000000000000000, 1.000000000000000000 ) ) ;
#22436 = ORIENTED_EDGE ( 'NONE', *, *, #32258, .F. ) ;
#22437 = EDGE_CURVE ( 'NONE', #16822, #17617, #33355, .T. ) ;
#22438 = DIRECTION ( 'NONE',  ( 1.000000000000000000, 0.000000000000000000, 0.000000000000000000 ) ) ;
#22439 = ORIENTED_EDGE ( 'NONE', *, *, #2511, .T. ) ;
#22440 = FACE_BOUND ( 'NONE', #17683, .T. ) ;
#22441 = DIRECTION ( 'NONE',  ( 1.000000000000000000, 0.000000000000000000, 0.000000000000000000 ) ) ;
#22442 = VECTOR ( 'NONE', #35400, 1000.000000000000000 ) ;
#22443 = CIRCLE ( 'NONE', #23055, 2.000000000000001776 ) ;
#22444 = ORIENTED_EDGE ( 'NONE', *, *, #27927, .F. ) ;
#22445 = DIRECTION ( 'NONE',  ( 1.000000000000000000, 0.000000000000000000, 0.000000000000000000 ) ) ;
#22446 = AXIS2_PLACEMENT_3D ( 'NONE', #8245, #14415, #5437 ) ;
#22447 = DIRECTION ( 'NONE',  ( 1.000000000000000000, 0.000000000000000000, 0.000000000000000000 ) ) ;
#22448 = EDGE_CURVE ( 'NONE', #19009, #11195, #19040, .T. ) ;
#22449 = DIRECTION ( 'NONE',  ( 0.000000000000000000, 0.000000000000000000, 1.000000000000000000 ) ) ;
#22450 = LINE ( 'NONE', #33901, #23898 ) ;
#22451 = ORIENTED_EDGE ( 'NONE', *, *, #25651, .T. ) ;
#22452 = DIRECTION ( 'NONE',  ( 1.000000000000000000, 0.000000000000000000, 0.000000000000000000 ) ) ;
#22453 = DIRECTION ( 'NONE',  ( 0.000000000000000000, 0.000000000000000000, 1.000000000000000000 ) ) ;
#22454 = CARTESIAN_POINT ( 'NONE',  ( 0.000000000000000000, 0.000000000000000000, 12.49999999999999822 ) ) ;
#22455 = AXIS2_PLACEMENT_3D ( 'NONE', #25833, #35001, #31437 ) ;
#22456 = CIRCLE ( 'NONE', #5710, 8.500000000000003553 ) ;
#22457 = ORIENTED_EDGE ( 'NONE', *, *, #21456, .T. ) ;
#22458 = ORIENTED_EDGE ( 'NONE', *, *, #15537, .T. ) ;
#22459 = PLANE ( 'NONE',  #1747 ) ;
#22460 = ORIENTED_EDGE ( 'NONE', *, *, #32946, .F. ) ;
#22461 = DIRECTION ( 'NONE',  ( 0.000000000000000000, 0.000000000000000000, 1.000000000000000000 ) ) ;
#22462 = CARTESIAN_POINT ( 'NONE',  ( -25.00000000000000000, 0.000000000000000000, -15.00000000000000000 ) ) ;
#22463 = DIRECTION ( 'NONE',  ( 0.000000000000000000, 0.000000000000000000, 1.000000000000000000 ) ) ;
#22464 = EDGE_CURVE ( 'NONE', #16555, #4566, #19620, .T. ) ;
#22465 = AXIS2_PLACEMENT_3D ( 'NONE', #26931, #30102, #21672 ) ;
#22466 = CARTESIAN_POINT ( 'NONE',  ( -4.597743007729434339, -3.118994528718985748, -0.4198507760575760361 ) ) ;
#22467 = CARTESIAN_POINT ( 'NONE',  ( -17.00000337463126243, 77.94228634059957983, -9.999999999999998224 ) ) ;
#22468 = CARTESIAN_POINT ( 'NONE',  ( -95.78732839747756600, -68.56887374850442995, 32.49999999999999289 ) ) ;
#22469 = EDGE_CURVE ( 'NONE', #16050, #29585, #13644, .T. ) ;
#22470 = AXIS2_PLACEMENT_3D ( 'NONE', #8128, #11485, #14112 ) ;
#22471 = CARTESIAN_POINT ( 'NONE',  ( 4.242640687119251020, -4.242640687119268783, 27.50000000000000000 ) ) ;
#22472 = CIRCLE ( 'NONE', #27879, 2.000000000000001776 ) ;
#22473 = FACE_OUTER_BOUND ( 'NONE', #26432, .T. ) ;
#22474 = CIRCLE ( 'NONE', #13475, 2.000000000000000000 ) ;
#22475 = ORIENTED_EDGE ( 'NONE', *, *, #16086, .F. ) ;
#22476 = EDGE_CURVE ( 'NONE', #14464, #27264, #30695, .T. ) ;
#22477 = AXIS2_PLACEMENT_3D ( 'NONE', #35422, #20569, #23413 ) ;
#22478 = ORIENTED_EDGE ( 'NONE', *, *, #9403, .T. ) ;
#22479 = CARTESIAN_POINT ( 'NONE',  ( 3.000000000000000000, -1.467624384280027172, 2.542000000000001592 ) ) ;
#22480 = CARTESIAN_POINT ( 'NONE',  ( -40.99999999999999289, 103.4105893997321743, 27.50000000000000000 ) ) ;
#22481 = DIRECTION ( 'NONE',  ( 0.000000000000000000, 0.000000000000000000, 1.000000000000000000 ) ) ;
#22482 = FACE_OUTER_BOUND ( 'NONE', #16200, .T. ) ;
#22483 = EDGE_CURVE ( 'NONE', #10350, #27052, #2866, .T. ) ;
#22484 = VERTEX_POINT ( 'NONE', #32275 ) ;
#22485 = EDGE_CURVE ( 'NONE', #14513, #7356, #32173, .T. ) ;
#22486 = AXIS2_PLACEMENT_3D ( 'NONE', #35568, #9859, #21300 ) ;
#22487 = VECTOR ( 'NONE', #5190, 1000.000000000000000 ) ;
#22488 = CARTESIAN_POINT ( 'NONE',  ( -45.00000000000000000, 0.000000000000000000, -5.000000000000000888 ) ) ;
#22489 = ORIENTED_EDGE ( 'NONE', *, *, #32824, .T. ) ;
#22490 = EDGE_LOOP ( 'NONE', ( #22909, #331, #18381, #25288 ) ) ;
#22491 = CARTESIAN_POINT ( 'NONE',  ( -63.00000337463104927, -25.98076211353322051, -5.000000000000000000 ) ) ;
#22492 = ORIENTED_EDGE ( 'NONE', *, *, #15362, .F. ) ;
#22493 = EDGE_CURVE ( 'NONE', #28322, #18808, #435, .T. ) ;
#22494 = CYLINDRICAL_SURFACE ( 'NONE', #21389, 2.000000000000001776 ) ;
#22495 = ADVANCED_FACE ( 'NONE', ( #10117 ), #7294, .T. ) ;
#22496 = CYLINDRICAL_SURFACE ( 'NONE', #3852, 2.000000000000001776 ) ;
#22497 = EDGE_CURVE ( 'NONE', #14414, #19227, #24730, .T. ) ;
#22498 = CARTESIAN_POINT ( 'NONE',  ( -73.00000337463100664, -43.30127018922202353, 17.49999999999999645 ) ) ;
#22499 = EDGE_CURVE ( 'NONE', #16356, #32680, #10466, .T. ) ;
#22500 = ORIENTED_EDGE ( 'NONE', *, *, #24373, .T. ) ;
#22501 = ORIENTED_EDGE ( 'NONE', *, *, #33924, .T. ) ;
#22502 = AXIS2_PLACEMENT_3D ( 'NONE', #26570, #1439, #9884 ) ;
#22503 = CIRCLE ( 'NONE', #11123, 2.000000000000001776 ) ;
#22504 = EDGE_LOOP ( 'NONE', ( #10786, #6900, #5436, #20358 ) ) ;
#22505 = AXIS2_PLACEMENT_3D ( 'NONE', #9675, #4415, #1595 ) ;
#22506 = CIRCLE ( 'NONE', #15899, 2.000000000000001776 ) ;
#22507 = VERTEX_POINT ( 'NONE', #2971 ) ;
#22508 = ORIENTED_EDGE ( 'NONE', *, *, #35808, .T. ) ;
#22509 = DIRECTION ( 'NONE',  ( 0.000000000000000000, 0.000000000000000000, 1.000000000000000000 ) ) ;
#22510 = CARTESIAN_POINT ( 'NONE',  ( 59.99999662536845335, 34.64101615137759893, 12.50000000000000000 ) ) ;
#22511 = CARTESIAN_POINT ( 'NONE',  ( 34.99999662536855283, -77.94228634059960825, -9.999999999999998224 ) ) ;
#22512 = AXIS2_PLACEMENT_3D ( 'NONE', #33118, #19260, #36517 ) ;
#22513 = DIRECTION ( 'NONE',  ( 0.000000000000000000, 0.000000000000000000, 1.000000000000000000 ) ) ;
#22514 = CARTESIAN_POINT ( 'NONE',  ( 64.99999662536839651, -43.30127018922199511, 12.50000000000000000 ) ) ;
#22515 = ORIENTED_EDGE ( 'NONE', *, *, #17942, .T. ) ;
#22516 = DIRECTION ( 'NONE',  ( -1.000000000000000000, 0.000000000000000000, 0.000000000000000000 ) ) ;
#22517 = CIRCLE ( 'NONE', #9934, 2.000000000000001776 ) ;
#22518 = DIRECTION ( 'NONE',  ( 1.000000000000000000, 0.000000000000000000, 0.000000000000000000 ) ) ;
#22519 = LINE ( 'NONE', #28864, #3830 ) ;
#22520 = ORIENTED_EDGE ( 'NONE', *, *, #29786, .F. ) ;
#22521 = LINE ( 'NONE', #11448, #5896 ) ;
#22522 = DIRECTION ( 'NONE',  ( 0.000000000000000000, 0.000000000000000000, 1.000000000000000000 ) ) ;
#22523 = EDGE_LOOP ( 'NONE', ( #29352, #1556, #26844, #33210, #11041 ) ) ;
#22524 = AXIS2_PLACEMENT_3D ( 'NONE', #29330, #26697, #6467 ) ;
#22525 = ORIENTED_EDGE ( 'NONE', *, *, #196, .F. ) ;
#22526 = CARTESIAN_POINT ( 'NONE',  ( 83.49774710563261237, -24.66044155380011915, 12.50000000000000000 ) ) ;
#22527 = CIRCLE ( 'NONE', #32084, 2.000000000000001776 ) ;
#22528 = CARTESIAN_POINT ( 'NONE',  ( -37.50000000000000000, 103.4105893997321743, 32.50000000000000000 ) ) ;
#22529 = CARTESIAN_POINT ( 'NONE',  ( -5.750000000000000000, 89.94802294027094547, 32.49999999999999289 ) ) ;
#22530 = CARTESIAN_POINT ( 'NONE',  ( -47.00000337463111322, 77.94228634059959404, -9.999999999999998224 ) ) ;
#22531 = ORIENTED_EDGE ( 'NONE', *, *, #29345, .F. ) ;
#22532 = ORIENTED_EDGE ( 'NONE', *, *, #246, .T. ) ;
#22533 = CIRCLE ( 'NONE', #6354, 2.000000000000001776 ) ;
#22534 = AXIS2_PLACEMENT_3D ( 'NONE', #35584, #9523, #15697 ) ;
#22535 = VECTOR ( 'NONE', #944, 1000.000000000000000 ) ;
#22536 = CIRCLE ( 'NONE', #13534, 2.000000000000001776 ) ;
#22537 = CARTESIAN_POINT ( 'NONE',  ( 0.000000000000000000, 0.000000000000000000, 12.49999999999999822 ) ) ;
#22538 = AXIS2_PLACEMENT_3D ( 'NONE', #2418, #25118, #10850 ) ;
#22539 = ORIENTED_EDGE ( 'NONE', *, *, #25740, .F. ) ;
#22540 = DIRECTION ( 'NONE',  ( 0.4999999999999919509, -0.8660254037844433705, 0.000000000000000000 ) ) ;
#22541 = ORIENTED_EDGE ( 'NONE', *, *, #27985, .F. ) ;
#22542 = DIRECTION ( 'NONE',  ( 1.000000000000000000, 0.000000000000000000, 0.000000000000000000 ) ) ;
#22543 = CIRCLE ( 'NONE', #3378, 2.445500000000000007 ) ;
#22544 = CARTESIAN_POINT ( 'NONE',  ( 42.99999662536850309, -60.62177826491080168, -9.999999999999998224 ) ) ;
#22545 = CARTESIAN_POINT ( 'NONE',  ( -32.49999999999947420, 56.29165124598880965, 12.49999999999999822 ) ) ;
#22546 = EDGE_CURVE ( 'NONE', #16338, #30229, #29182, .T. ) ;
#22547 = ORIENTED_EDGE ( 'NONE', *, *, #34354, .T. ) ;
#22548 = ORIENTED_EDGE ( 'NONE', *, *, #31325, .T. ) ;
#22549 = CARTESIAN_POINT ( 'NONE',  ( -3.000000000000000888, 3.673940397442060854E-16, -5.700000000000000178 ) ) ;
#22550 = CARTESIAN_POINT ( 'NONE',  ( -75.00000337463097821, 25.98076211353318854, -9.999999999999998224 ) ) ;
#22551 = CIRCLE ( 'NONE', #11171, 2.000000000000001776 ) ;
#22552 = DIRECTION ( 'NONE',  ( -1.000000000000000000, -0.000000000000000000, -0.000000000000000000 ) ) ;
#22553 = CARTESIAN_POINT ( 'NONE',  ( 74.99999662536836809, 8.660254037844394404, -9.999999999999998224 ) ) ;
#22554 = CIRCLE ( 'NONE', #10595, 2.000000000000001776 ) ;
#22555 = VERTEX_POINT ( 'NONE', #11205 ) ;
#22556 = FACE_OUTER_BOUND ( 'NONE', #2118, .T. ) ;
#22557 = FACE_BOUND ( 'NONE', #25991, .T. ) ;
#22558 = DIRECTION ( 'NONE',  ( -1.000000000000000000, 0.000000000000000000, 0.000000000000000000 ) ) ;
#22559 = FACE_OUTER_BOUND ( 'NONE', #32063, .T. ) ;
#22560 = VECTOR ( 'NONE', #5868, 1000.000000000000000 ) ;
#22561 = PLANE ( 'NONE',  #32049 ) ;
#22562 = DIRECTION ( 'NONE',  ( 0.000000000000000000, 0.000000000000000000, 1.000000000000000000 ) ) ;
#22563 = VECTOR ( 'NONE', #27415, 1000.000000000000000 ) ;
#22564 = AXIS2_PLACEMENT_3D ( 'NONE', #18121, #24310, #15511 ) ;
#22565 = CARTESIAN_POINT ( 'NONE',  ( 47.99999662536846756, -69.28203230275519786, -5.000000000000000000 ) ) ;
#22566 = CARTESIAN_POINT ( 'NONE',  ( 44.99999662536849598, 60.62177826491077326, -9.999999999999998224 ) ) ;
#22567 = ORIENTED_EDGE ( 'NONE', *, *, #26726, .F. ) ;
#22568 = FACE_OUTER_BOUND ( 'NONE', #36803, .T. ) ;
#22569 = CYLINDRICAL_SURFACE ( 'NONE', #6358, 2.000000000000001776 ) ;
#22570 = DIRECTION ( 'NONE',  ( 0.000000000000000000, 0.000000000000000000, 1.000000000000000000 ) ) ;
#22571 = EDGE_CURVE ( 'NONE', #5770, #23807, #13658, .T. ) ;
#22572 = EDGE_CURVE ( 'NONE', #11869, #7527, #21402, .T. ) ;
#22573 = ORIENTED_EDGE ( 'NONE', *, *, #5589, .T. ) ;
#22574 = AXIS2_PLACEMENT_3D ( 'NONE', #2489, #28526, #7923 ) ;
#22575 = EDGE_LOOP ( 'NONE', ( #10727, #31253, #1767, #2495 ) ) ;
#22576 = ORIENTED_EDGE ( 'NONE', *, *, #11240, .T. ) ;
#22577 = DIRECTION ( 'NONE',  ( 0.000000000000000000, 0.000000000000000000, 1.000000000000000000 ) ) ;
#22578 = CARTESIAN_POINT ( 'NONE',  ( -77.00000337463099243, -25.98076211353322051, 12.50000000000000000 ) ) ;
#22579 = ORIENTED_EDGE ( 'NONE', *, *, #3928, .F. ) ;
#22580 = AXIS2_PLACEMENT_3D ( 'NONE', #1830, #24888, #32958 ) ;
#22581 = CIRCLE ( 'NONE', #21375, 2.000000000000001776 ) ;
#22582 = DIRECTION ( 'NONE',  ( 0.000000000000000000, 0.000000000000000000, 1.000000000000000000 ) ) ;
#22583 = EDGE_CURVE ( 'NONE', #10982, #7521, #31091, .T. ) ;
#22584 = VECTOR ( 'NONE', #19033, 1000.000000000000000 ) ;
#22585 = ORIENTED_EDGE ( 'NONE', *, *, #27420, .T. ) ;
#22586 = DIRECTION ( 'NONE',  ( -0.7071067811865487940, -0.7071067811865463515, 0.000000000000000000 ) ) ;
#22587 = EDGE_LOOP ( 'NONE', ( #21005, #4036, #28928, #4412 ) ) ;
#22588 = CARTESIAN_POINT ( 'NONE',  ( 4.279621169095998212, -62.97617850287780072, -4.999999999999997335 ) ) ;
#22589 =( GEOMETRIC_REPRESENTATION_CONTEXT ( 3 ) GLOBAL_UNCERTAINTY_ASSIGNED_CONTEXT ( ( #7321 ) ) GLOBAL_UNIT_ASSIGNED_CONTEXT ( ( #5910, #14694, #31572 ) ) REPRESENTATION_CONTEXT ( 'NONE', 'WORKASPACE' ) );
#22590 = ORIENTED_EDGE ( 'NONE', *, *, #24538, .T. ) ;
#22591 = CIRCLE ( 'NONE', #34564, 5.750000000000002665 ) ;
#22592 = VECTOR ( 'NONE', #15089, 1000.000000000000000 ) ;
#22593 = FACE_OUTER_BOUND ( 'NONE', #35421, .T. ) ;
#22594 = DIRECTION ( 'NONE',  ( 1.000000000000000000, 0.000000000000000000, 0.000000000000000000 ) ) ;
#22595 = ADVANCED_FACE ( 'NONE', ( #33904 ), #28266, .F. ) ;
#22596 = EDGE_LOOP ( 'NONE', ( #16946, #32665, #32413, #31975 ) ) ;
#22597 = CARTESIAN_POINT ( 'NONE',  ( 14.99999662536859901, 77.94228634059957983, 17.49999999999999645 ) ) ;
#22598 = VECTOR ( 'NONE', #1983, 999.9999999999998863 ) ;
#22599 = ITEM_DEFINED_TRANSFORMATION ( 'NONE', 'NONE', #32726,  #21385 ) ;
#22600 = VECTOR ( 'NONE', #9947, 1000.000000000000000 ) ;
#22601 = FACE_OUTER_BOUND ( 'NONE', #30530, .T. ) ;
#22602 = FACE_OUTER_BOUND ( 'NONE', #33657, .T. ) ;
#22603 = ORIENTED_EDGE ( 'NONE', *, *, #22910, .T. ) ;
#22604 = CARTESIAN_POINT ( 'NONE',  ( -70.47608876694631874, -59.13646009116124702, 12.49999999999999822 ) ) ;
#22606 = DIRECTION ( 'NONE',  ( -0.000000000000000000, -0.000000000000000000, -1.000000000000000000 ) ) ;
#22605 = CIRCLE ( 'NONE', #10646, 2.000000000000000000 ) ;
#22607 = ORIENTED_EDGE ( 'NONE', *, *, #31767, .F. ) ;
#22608 = DIRECTION ( 'NONE',  ( -0.000000000000000000, -0.000000000000000000, 1.000000000000000000 ) ) ;
#22609 = AXIS2_PLACEMENT_3D ( 'NONE', #6653, #3825, #35710 ) ;
#22610 = CARTESIAN_POINT ( 'NONE',  ( 0.000000000000000000, 0.000000000000000000, -5.000000000000000000 ) ) ;
#22611 = FACE_OUTER_BOUND ( 'NONE', #8476, .T. ) ;
#22613 = AXIS2_PLACEMENT_3D ( 'NONE', #9405, #1855, #20840 ) ;
#22612 = DIRECTION ( 'NONE',  ( 1.000000000000000000, 0.000000000000000000, 0.000000000000000000 ) ) ;
#22614 = ORIENTED_EDGE ( 'NONE', *, *, #11684, .T. ) ;
#22615 = CIRCLE ( 'NONE', #34619, 8.500000000000000000 ) ;
#22616 = EDGE_CURVE ( 'NONE', #210, #1373, #36988, .T. ) ;
#22617 = VERTEX_POINT ( 'NONE', #5418 ) ;
#22618 = CARTESIAN_POINT ( 'NONE',  ( 0.000000000000000000, -1.467624384280027172, 2.542000000000001592 ) ) ;
#22619 = DIRECTION ( 'NONE',  ( -1.000000000000000000, 0.000000000000000000, 0.000000000000000000 ) ) ;
#22620 = ADVANCED_FACE ( 'NONE', ( #36715 ), #34277, .F. ) ;
#22621 = AXIS2_PLACEMENT_3D ( 'NONE', #324, #14411, #34675 ) ;
#22622 = AXIS2_PLACEMENT_3D ( 'NONE', #11512, #8528, #31573 ) ;
#22623 = ORIENTED_EDGE ( 'NONE', *, *, #36124, .T. ) ;
#22624 = EDGE_LOOP ( 'NONE', ( #26754, #19842, #33488 ) ) ;
#22625 = PRODUCT_RELATED_PRODUCT_CATEGORY ( 'part', '', ( #34021 ) ) ;
#22626 = CARTESIAN_POINT ( 'NONE',  ( 0.000000000000000000, 0.000000000000000000, 3.400000000000000355 ) ) ;
#22627 = LINE ( 'NONE', #31064, #29202 ) ;
#22628 =( REPRESENTATION_RELATIONSHIP ('NONE','NONE', #15268, #35440 ) REPRESENTATION_RELATIONSHIP_WITH_TRANSFORMATION ( #32736 )SHAPE_REPRESENTATION_RELATIONSHIP( ) );
#22629 = ADVANCED_FACE ( 'NONE', ( #22281 ), #34106, .F. ) ;
#22630 = DIRECTION ( 'NONE',  ( 0.000000000000000000, 0.000000000000000000, 1.000000000000000000 ) ) ;
#22631 = AXIS2_PLACEMENT_3D ( 'NONE', #32505, #1021, #27246 ) ;
#22632 = ORIENTED_EDGE ( 'NONE', *, *, #18830, .F. ) ;
#22633 = ORIENTED_EDGE ( 'NONE', *, *, #18978, .F. ) ;
#22634 = DIRECTION ( 'NONE',  ( -0.000000000000000000, -0.000000000000000000, 1.000000000000000000 ) ) ;
#22635 = ADVANCED_FACE ( 'NONE', ( #28639 ), #2220, .F. ) ;
#22636 = CIRCLE ( 'NONE', #13663, 2.000000000000001776 ) ;
#22637 = DIRECTION ( 'NONE',  ( 0.000000000000000000, 0.000000000000000000, 1.000000000000000000 ) ) ;
#22638 = ORIENTED_EDGE ( 'NONE', *, *, #7539, .F. ) ;
#22639 = DIRECTION ( 'NONE',  ( 0.000000000000000000, 0.000000000000000000, 1.000000000000000000 ) ) ;
#22640 = ORIENTED_EDGE ( 'NONE', *, *, #1632, .T. ) ;
#22641 = AXIS2_PLACEMENT_3D ( 'NONE', #17375, #28795, #2947 ) ;
#22642 = CIRCLE ( 'NONE', #1112, 2.000000000000001776 ) ;
#22643 = FACE_BOUND ( 'NONE', #1580, .T. ) ;
#22644 = VECTOR ( 'NONE', #4824, 1000.000000000000000 ) ;
#22645 = AXIS2_PLACEMENT_3D ( 'NONE', #7910, #15787, #24425 ) ;
#22646 = DIRECTION ( 'NONE',  ( 0.000000000000000000, 0.000000000000000000, 1.000000000000000000 ) ) ;
#22647 = ORIENTED_EDGE ( 'NONE', *, *, #21090, .T. ) ;
#22648 = DIRECTION ( 'NONE',  ( -0.9311380786261235221, -0.3646668048129015904, 0.000000000000000000 ) ) ;
#22649 = DIRECTION ( 'NONE',  ( -0.000000000000000000, -0.000000000000000000, 1.000000000000000000 ) ) ;
#22650 = CIRCLE ( 'NONE', #8285, 3.000000000000002665 ) ;
#22651 = EDGE_CURVE ( 'NONE', #25777, #27468, #25839, .T. ) ;
#22652 = DIRECTION ( 'NONE',  ( 1.000000000000000000, 0.000000000000000000, 0.000000000000000000 ) ) ;
#22653 = CYLINDRICAL_SURFACE ( 'NONE', #35283, 2.000000000000001776 ) ;
#22654 = ORIENTED_EDGE ( 'NONE', *, *, #33520, .T. ) ;
#22655 = CARTESIAN_POINT ( 'NONE',  ( 39.99999662536853151, 69.28203230275518365, -9.999999999999998224 ) ) ;
#22656 = DIRECTION ( 'NONE',  ( -1.000000000000000000, 0.000000000000000000, 0.000000000000000000 ) ) ;
#22657 = AXIS2_PLACEMENT_3D ( 'NONE', #8578, #20012, #31441 ) ;
#22658 = CARTESIAN_POINT ( 'NONE',  ( -2.925285743277526329, -4.084588180558410109, -5.989444439476605986 ) ) ;
#22659 = EDGE_CURVE ( 'NONE', #13352, #7812, #35233, .T. ) ;
#22660 = ORIENTED_EDGE ( 'NONE', *, *, #4630, .T. ) ;
#22661 = ORIENTED_EDGE ( 'NONE', *, *, #36011, .F. ) ;
#22662 = AXIS2_PLACEMENT_3D ( 'NONE', #33396, #25319, #30933 ) ;
#22663 = EDGE_CURVE ( 'NONE', #17059, #16108, #30888, .T. ) ;
#22664 = EDGE_LOOP ( 'NONE', ( #17440, #3832 ) ) ;
#22665 = AXIS2_PLACEMENT_3D ( 'NONE', #17437, #23254, #3021 ) ;
#22666 = DIRECTION ( 'NONE',  ( 0.000000000000000000, 0.000000000000000000, 1.000000000000000000 ) ) ;
#22667 = CARTESIAN_POINT ( 'NONE',  ( -52.39915983220772233, -35.19434990244957362, -4.999999999999997335 ) ) ;
#22668 = CIRCLE ( 'NONE', #10089, 2.000000000000001776 ) ;
#22669 = DIRECTION ( 'NONE',  ( 0.000000000000000000, 0.000000000000000000, -1.000000000000000000 ) ) ;
#22670 = AXIS2_PLACEMENT_3D ( 'NONE', #13125, #1483, #7488 ) ;
#22671 = CARTESIAN_POINT ( 'NONE',  ( -0.4022569922705816481, 5.541259509125439742, -0.4198507760575647119 ) ) ;
#22672 = CARTESIAN_POINT ( 'NONE',  ( 106.9297252919371175, -51.67691575806412629, 32.50000000000000000 ) ) ;
#22673 = CARTESIAN_POINT ( 'NONE',  ( -106.8619808665325337, -52.03941024792912629, 32.50000000000000000 ) ) ;
#22674 = DIRECTION ( 'NONE',  ( -0.000000000000000000, -0.000000000000000000, 1.000000000000000000 ) ) ;
#22676 = CIRCLE ( 'NONE', #28050, 2.000000000000001776 ) ;
#22675 = CYLINDRICAL_SURFACE ( 'NONE', #12429, 3.500000000000003109 ) ;
#22677 = VERTEX_POINT ( 'NONE', #30708 ) ;
#22678 = EDGE_LOOP ( 'NONE', ( #18664, #11908, #29265, #34290 ) ) ;
#22679 = AXIS2_PLACEMENT_3D ( 'NONE', #27241, #19371, #35703 ) ;
#22680 = FACE_BOUND ( 'NONE', #34979, .T. ) ;
#22681 = ADVANCED_FACE ( 'NONE', ( #19840 ), #11012, .F. ) ;
#22682 = DIRECTION ( 'NONE',  ( 0.000000000000000000, 0.000000000000000000, 1.000000000000000000 ) ) ;
#22683 = CARTESIAN_POINT ( 'NONE',  ( 84.99999662536832545, 8.660254037844394404, -5.000000000000000000 ) ) ;
#22684 = DIRECTION ( 'NONE',  ( 1.000000000000000000, 0.000000000000000000, 0.000000000000000000 ) ) ;
#22685 = VERTEX_POINT ( 'NONE', #14009 ) ;
#22686 = FACE_BOUND ( 'NONE', #9708, .T. ) ;
#22687 = CIRCLE ( 'NONE', #25668, 2.000000000000001776 ) ;
#22688 = ORIENTED_EDGE ( 'NONE', *, *, #12409, .F. ) ;
#22689 = ORIENTED_EDGE ( 'NONE', *, *, #30744, .T. ) ;
#22690 = AXIS2_PLACEMENT_3D ( 'NONE', #17897, #28938, #22963 ) ;
#22691 = CARTESIAN_POINT ( 'NONE',  ( -70.00000337463099243, 17.32050807568877460, -9.999999999999998224 ) ) ;
#22692 = VERTEX_POINT ( 'NONE', #8024 ) ;
#22693 = DIRECTION ( 'NONE',  ( -1.000000000000000000, 0.000000000000000000, 0.000000000000000000 ) ) ;
#22694 = FACE_OUTER_BOUND ( 'NONE', #835, .T. ) ;
#22695 = EDGE_CURVE ( 'NONE', #29460, #23785, #4092, .T. ) ;
#22696 = DIRECTION ( 'NONE',  ( 0.000000000000000000, 0.000000000000000000, 1.000000000000000000 ) ) ;
#22697 = AXIS2_PLACEMENT_3D ( 'NONE', #26879, #4366, #27224 ) ;
#22698 = EDGE_LOOP ( 'NONE', ( #10688, #12904, #25522, #36650 ) ) ;
#22699 = EDGE_CURVE ( 'NONE', #29605, #16351, #32808, .T. ) ;
#22700 = ORIENTED_EDGE ( 'NONE', *, *, #18987, .F. ) ;
#22701 = AXIS2_PLACEMENT_3D ( 'NONE', #28118, #25688, #19685 ) ;
#22702 = ORIENTED_EDGE ( 'NONE', *, *, #35574, .F. ) ;
#22703 = EDGE_CURVE ( 'NONE', #2655, #35919, #37097, .T. ) ;
#22704 = ORIENTED_EDGE ( 'NONE', *, *, #1729, .F. ) ;
#22705 = VECTOR ( 'NONE', #27333, 1000.000000000000000 ) ;
#22706 = EDGE_LOOP ( 'NONE', ( #1468, #6165, #24699, #12181, #28227 ) ) ;
#22707 = DIRECTION ( 'NONE',  ( 1.000000000000000000, 0.000000000000000000, 0.000000000000000000 ) ) ;
#22709 = DIRECTION ( 'NONE',  ( 1.000000000000000000, 0.000000000000000000, 0.000000000000000000 ) ) ;
#22708 = AXIS2_PLACEMENT_3D ( 'NONE', #28785, #25974, #274 ) ;
#22710 = EDGE_CURVE ( 'NONE', #12225, #7729, #6478, .T. ) ;
#22711 = DIRECTION ( 'NONE',  ( -1.000000000000000000, 0.000000000000000000, -0.000000000000000000 ) ) ;
#22712 = DIRECTION ( 'NONE',  ( 1.000000000000000000, 0.000000000000000000, 0.000000000000000000 ) ) ;
#22713 = CYLINDRICAL_SURFACE ( 'NONE', #18950, 3.000000000000002665 ) ;
#22714 = EDGE_CURVE ( 'NONE', #29420, #8519, #36435, .T. ) ;
#22715 = ORIENTED_EDGE ( 'NONE', *, *, #33888, .F. ) ;
#22716 = DIRECTION ( 'NONE',  ( 1.000000000000000000, 0.000000000000000000, 0.000000000000000000 ) ) ;
#22717 = DIRECTION ( 'NONE',  ( 0.000000000000000000, 0.000000000000000000, -1.000000000000000000 ) ) ;
#22718 = AXIS2_PLACEMENT_3D ( 'NONE', #7664, #36546, #19288 ) ;
#22719 = CARTESIAN_POINT ( 'NONE',  ( -60.00000337463104216, 34.64101615137757051, 17.49999999999999645 ) ) ;
#22720 = ORIENTED_EDGE ( 'NONE', *, *, #659, .F. ) ;
#22721 = CARTESIAN_POINT ( 'NONE',  ( 49.99999662536846756, 51.96152422706637708, -9.999999999999998224 ) ) ;
#22722 = AXIS2_PLACEMENT_3D ( 'NONE', #33630, #36797, #7933 ) ;
#22723 = DIRECTION ( 'NONE',  ( 1.000000000000000000, 0.000000000000000000, 0.000000000000000000 ) ) ;
#22724 = EDGE_CURVE ( 'NONE', #17922, #9816, #18472, .T. ) ;
#22725 = VERTEX_POINT ( 'NONE', #26751 ) ;
#22726 = EDGE_CURVE ( 'NONE', #16319, #2878, #26388, .T. ) ;
#22727 = ORIENTED_EDGE ( 'NONE', *, *, #20369, .T. ) ;
#22728 = LINE ( 'NONE', #11279, #29013 ) ;
#22729 = EDGE_CURVE ( 'NONE', #32307, #2310, #27427, .T. ) ;
#22730 = AXIS2_PLACEMENT_3D ( 'NONE', #29712, #35189, #35388 ) ;
#22731 = DIRECTION ( 'NONE',  ( 1.000000000000000000, 0.000000000000000000, 0.000000000000000000 ) ) ;
#22732 = CARTESIAN_POINT ( 'NONE',  ( -3.500000000000000888, 55.00000000000000000, -5.000000000000000888 ) ) ;
#22733 = ADVANCED_FACE ( 'NONE', ( #34829 ), #5970, .T. ) ;
#22734 = DIRECTION ( 'NONE',  ( 1.000000000000000000, 0.000000000000000000, 0.000000000000000000 ) ) ;
#22735 = ORIENTED_EDGE ( 'NONE', *, *, #13444, .T. ) ;
#22736 = VERTEX_POINT ( 'NONE', #23761 ) ;
#22737 = VECTOR ( 'NONE', #15290, 1000.000000000000000 ) ;
#22738 = SHAPE_REPRESENTATION ( 'socket head cap screw_iso_ISO 4762 M6 x 30 - 30N', ( #21385 ), #2159 ) ;
#22739 = DIRECTION ( 'NONE',  ( -0.000000000000000000, 0.000000000000000000, -1.000000000000000000 ) ) ;
#22740 = LINE ( 'NONE', #8475, #35684 ) ;
#22741 = CIRCLE ( 'NONE', #6560, 2.000000000000001776 ) ;
#22742 = ORIENTED_EDGE ( 'NONE', *, *, #5654, .F. ) ;
#22743 = DIRECTION ( 'NONE',  ( 0.000000000000000000, 0.000000000000000000, -1.000000000000000000 ) ) ;
#22744 = ORIENTED_EDGE ( 'NONE', *, *, #12289, .T. ) ;
#22745 = EDGE_LOOP ( 'NONE', ( #18157, #2178, #27116, #29846 ) ) ;
#22746 = CARTESIAN_POINT ( 'NONE',  ( 32.49999999999987210, -56.29165124598858938, 12.49999999999999822 ) ) ;
#22747 = LINE ( 'NONE', #16917, #4075 ) ;
#22748 = EDGE_CURVE ( 'NONE', #6874, #16532, #35007, .T. ) ;
#22749 = AXIS2_PLACEMENT_3D ( 'NONE', #1063, #29376, #9862 ) ;
#22750 = DIRECTION ( 'NONE',  ( 0.000000000000000000, 0.000000000000000000, 1.000000000000000000 ) ) ;
#22751 = ORIENTED_EDGE ( 'NONE', *, *, #8930, .T. ) ;
#22752 = VERTEX_POINT ( 'NONE', #35214 ) ;
#22753 = CARTESIAN_POINT ( 'NONE',  ( -72.00000337463102085, -51.96152422706641971, -9.999999999999998224 ) ) ;
#22754 = AXIS2_PLACEMENT_3D ( 'NONE', #6689, #35402, #6863 ) ;
#22755 = CARTESIAN_POINT ( 'NONE',  ( -33.00000337463116296, 77.94228634059957983, -9.999999999999998224 ) ) ;
#22756 = DIRECTION ( 'NONE',  ( -0.000000000000000000, -0.000000000000000000, 1.000000000000000000 ) ) ;
#22757 = DIRECTION ( 'NONE',  ( 1.000000000000000000, 0.000000000000000000, 0.000000000000000000 ) ) ;
#22758 = ORIENTED_EDGE ( 'NONE', *, *, #10884, .F. ) ;
#22759 = DIRECTION ( 'NONE',  ( 1.000000000000000000, 0.000000000000000000, 0.000000000000000000 ) ) ;
#22760 = FACE_BOUND ( 'NONE', #1986, .T. ) ;
#22761 = EDGE_CURVE ( 'NONE', #22972, #13489, #2895, .T. ) ;
#22762 = DIRECTION ( 'NONE',  ( 0.000000000000000000, 0.000000000000000000, 1.000000000000000000 ) ) ;
#22763 = CARTESIAN_POINT ( 'NONE',  ( 2.999999999999768630, -68.00000000000000000, 12.49999999999999822 ) ) ;
#22764 = LINE ( 'NONE', #34205, #15917 ) ;
#22765 = VECTOR ( 'NONE', #24285, 1000.000000000000000 ) ;
#22766 = DIRECTION ( 'NONE',  ( -1.000000000000000000, 0.000000000000000000, -0.000000000000000000 ) ) ;
#22767 = DIRECTION ( 'NONE',  ( 1.000000000000000000, 0.000000000000000000, 0.000000000000000000 ) ) ;
#22768 = AXIS2_PLACEMENT_3D ( 'NONE', #21414, #33033, #21774 ) ;
#22769 = DIRECTION ( 'NONE',  ( 0.000000000000000000, 0.000000000000000000, -1.000000000000000000 ) ) ;
#22770 = ORIENTED_EDGE ( 'NONE', *, *, #33830, .T. ) ;
#22771 = DIRECTION ( 'NONE',  ( -1.000000000000000000, 0.000000000000000000, 0.000000000000000000 ) ) ;
#22772 = CARTESIAN_POINT ( 'NONE',  ( 37.50000000000000000, 103.4105893997321743, 32.50000000000000000 ) ) ;
#22773 = VECTOR ( 'NONE', #4221, 1000.000000000000000 ) ;
#22774 = DIRECTION ( 'NONE',  ( -1.000000000000000000, 0.000000000000000000, 0.000000000000000000 ) ) ;
#22775 = ORIENTED_EDGE ( 'NONE', *, *, #29029, .T. ) ;
#22776 = EDGE_CURVE ( 'NONE', #28212, #19903, #26221, .T. ) ;
#22777 = ORIENTED_EDGE ( 'NONE', *, *, #29661, .T. ) ;
#22778 = ORIENTED_EDGE ( 'NONE', *, *, #29566, .T. ) ;
#22779 = EDGE_CURVE ( 'NONE', #17325, #12004, #32201, .T. ) ;
#22780 = EDGE_CURVE ( 'NONE', #27172, #34636, #4692, .T. ) ;
#22781 = DIRECTION ( 'NONE',  ( 0.000000000000000000, 0.000000000000000000, 1.000000000000000000 ) ) ;
#22782 = DIRECTION ( 'NONE',  ( 1.000000000000000000, 0.000000000000000000, 0.000000000000000000 ) ) ;
#22783 = DIRECTION ( 'NONE',  ( -1.000000000000000000, 0.000000000000000000, 0.000000000000000000 ) ) ;
#22784 = AXIS2_PLACEMENT_3D ( 'NONE', #24687, #27666, #13240 ) ;
#22785 = ORIENTED_EDGE ( 'NONE', *, *, #12113, .F. ) ;
#22786 = DIRECTION ( 'NONE',  ( 0.000000000000000000, -0.000000000000000000, -1.000000000000000000 ) ) ;
#22787 = VERTEX_POINT ( 'NONE', #31801 ) ;
#22788 = AXIS2_PLACEMENT_3D ( 'NONE', #36819, #20312, #6064 ) ;
#22789 = CYLINDRICAL_SURFACE ( 'NONE', #13761, 2.000000000000001776 ) ;
#22790 = ORIENTED_EDGE ( 'NONE', *, *, #9389, .T. ) ;
#22791 = DIRECTION ( 'NONE',  ( -1.000000000000000000, 0.000000000000000000, 0.000000000000000000 ) ) ;
#22792 = VERTEX_POINT ( 'NONE', #12101 ) ;
#22793 = ORIENTED_EDGE ( 'NONE', *, *, #26581, .F. ) ;
#22794 = LINE ( 'NONE', #27833, #24392 ) ;
#22795 = CYLINDRICAL_SURFACE ( 'NONE', #13625, 2.000000000000001776 ) ;
#22796 = AXIS2_PLACEMENT_3D ( 'NONE', #30952, #14066, #25520 ) ;
#22797 = ORIENTED_EDGE ( 'NONE', *, *, #11911, .T. ) ;
#22798 = DIRECTION ( 'NONE',  ( 0.000000000000000000, 0.000000000000000000, -1.000000000000000000 ) ) ;
#22799 = MECHANICAL_DESIGN_GEOMETRIC_PRESENTATION_REPRESENTATION (  '', ( #19798 ), #19191 ) ;
#22800 = CONTEXT_DEPENDENT_SHAPE_REPRESENTATION ( #12534, #36479 ) ;
#22801 = ADVANCED_FACE ( 'NONE', ( #34458 ), #309, .F. ) ;
#22802 = LINE ( 'NONE', #32124, #6682 ) ;
#22803 = DIRECTION ( 'NONE',  ( 0.000000000000000000, 0.000000000000000000, -1.000000000000000000 ) ) ;
#22804 = ORIENTED_EDGE ( 'NONE', *, *, #18685, .F. ) ;
#22805 = CARTESIAN_POINT ( 'NONE',  ( 44.99999662536849598, -77.94228634059960825, -9.999999999999998224 ) ) ;
#22806 = LINE ( 'NONE', #20345, #27561 ) ;
#22807 = ORIENTED_EDGE ( 'NONE', *, *, #37042, .T. ) ;
#22808 = CARTESIAN_POINT ( 'NONE',  ( 33.99999999999999289, 103.4105893997321743, -19.99999999999999645 ) ) ;
#22809 = DIRECTION ( 'NONE',  ( 0.000000000000000000, 0.000000000000000000, 1.000000000000000000 ) ) ;
#22810 = CARTESIAN_POINT ( 'NONE',  ( -20.00000337463122690, 86.60254037844397601, -5.000000000000000000 ) ) ;
#22811 = CARTESIAN_POINT ( 'NONE',  ( 0.000000000000000000, 0.000000000000000000, 32.50000000000000000 ) ) ;
#22812 = ORIENTED_EDGE ( 'NONE', *, *, #13, .T. ) ;
#22813 = ORIENTED_EDGE ( 'NONE', *, *, #15550, .T. ) ;
#22814 = LINE ( 'NONE', #22248, #32122 ) ;
#22815 = DIRECTION ( 'NONE',  ( 1.000000000000000000, 0.000000000000000000, 0.000000000000000000 ) ) ;
#22816 = EDGE_LOOP ( 'NONE', ( #22539, #2376, #35466, #21776, #29214 ) ) ;
#22817 = VERTEX_POINT ( 'NONE', #15124 ) ;
#22818 = AXIS2_PLACEMENT_3D ( 'NONE', #20020, #34668, #14964 ) ;
#22819 = ADVANCED_FACE ( 'NONE', ( #8764, #20205 ), #6133, .T. ) ;
#22820 = DIRECTION ( 'NONE',  ( 1.000000000000000000, 0.000000000000000000, 0.000000000000000000 ) ) ;
#22821 = LINE ( 'NONE', #14374, #27425 ) ;
#22822 = CARTESIAN_POINT ( 'NONE',  ( 0.000000000000000000, 89.94802294027088863, -24.99999999999999645 ) ) ;
#22823 = ORIENTED_EDGE ( 'NONE', *, *, #33084, .F. ) ;
#22824 = EDGE_LOOP ( 'NONE', ( #3967, #27418 ) ) ;
#22825 = CYLINDRICAL_SURFACE ( 'NONE', #9300, 3.500000000000003109 ) ;
#22826 = DIRECTION ( 'NONE',  ( 1.000000000000000000, 0.000000000000000000, 0.000000000000000000 ) ) ;
#22827 = VERTEX_POINT ( 'NONE', #14567 ) ;
#22828 = CARTESIAN_POINT ( 'NONE',  ( -43.00000337463112743, -60.62177826491080168, -5.000000000000000000 ) ) ;
#22829 = EDGE_LOOP ( 'NONE', ( #17264, #15902 ) ) ;
#22830 = CARTESIAN_POINT ( 'NONE',  ( -42.00000337463114164, -69.28203230275519786, -9.999999999999998224 ) ) ;
#22831 = DIRECTION ( 'NONE',  ( 0.000000000000000000, 0.000000000000000000, 1.000000000000000000 ) ) ;
#22832 = DIRECTION ( 'NONE',  ( 0.000000000000000000, -0.000000000000000000, -1.000000000000000000 ) ) ;
#22833 = VERTEX_POINT ( 'NONE', #29379 ) ;
#22834 = EDGE_CURVE ( 'NONE', #7482, #36258, #33433, .T. ) ;
#22835 = CARTESIAN_POINT ( 'NONE',  ( 70.80619744048946984, -84.18124734178287838, 38.50000000000000000 ) ) ;
#22836 = DIRECTION ( 'NONE',  ( 0.000000000000000000, 0.000000000000000000, 1.000000000000000000 ) ) ;
#22837 = CYLINDRICAL_SURFACE ( 'NONE', #34133, 2.000000000000001776 ) ;
#22838 = DIRECTION ( 'NONE',  ( -0.000000000000000000, -0.000000000000000000, -1.000000000000000000 ) ) ;
#22839 = ORIENTED_EDGE ( 'NONE', *, *, #35156, .T. ) ;
#22840 = DIRECTION ( 'NONE',  ( 1.000000000000000000, 0.000000000000000000, 0.000000000000000000 ) ) ;
#22841 = CARTESIAN_POINT ( 'NONE',  ( -65.00000337463102085, 60.62177826491077326, -5.000000000000000000 ) ) ;
#22842 = CARTESIAN_POINT ( 'NONE',  ( 64.99999662536842493, 43.30127018922200222, -9.999999999999998224 ) ) ;
#22843 = EDGE_LOOP ( 'NONE', ( #35669, #20539 ) ) ;
#22844 = EDGE_CURVE ( 'NONE', #30934, #26515, #2300, .T. ) ;
#22845 = EDGE_LOOP ( 'NONE', ( #12322, #31920, #11497, #12049 ) ) ;
#22846 =( REPRESENTATION_RELATIONSHIP ('NONE','NONE', #15268, #35880 ) REPRESENTATION_RELATIONSHIP_WITH_TRANSFORMATION ( #22058 )SHAPE_REPRESENTATION_RELATIONSHIP( ) );
#22847 = VERTEX_POINT ( 'NONE', #14957 ) ;
#22848 = DIRECTION ( 'NONE',  ( 4.625929269271481378E-15, 1.000000000000000000, 0.000000000000000000 ) ) ;
#22849 = VECTOR ( 'NONE', #34603, 1000.000000000000000 ) ;
#22850 = CARTESIAN_POINT ( 'NONE',  ( 90.60231327712337190, 15.97563234535636134, 12.49999999999999822 ) ) ;
#22851 = EDGE_CURVE ( 'NONE', #114, #12647, #26557, .T. ) ;
#22852 = LINE ( 'NONE', #30907, #20867 ) ;
#22853 = DIRECTION ( 'NONE',  ( -1.000000000000000000, 0.000000000000000000, 0.000000000000000000 ) ) ;
#22854 = CIRCLE ( 'NONE', #15660, 2.000000000000001776 ) ;
#22855 = FACE_OUTER_BOUND ( 'NONE', #28687, .T. ) ;
#22856 = DIRECTION ( 'NONE',  ( -1.047444401652940795E-14, -1.000000000000000000, 0.000000000000000000 ) ) ;
#22857 = ORIENTED_EDGE ( 'NONE', *, *, #3610, .F. ) ;
#22858 = VERTEX_POINT ( 'NONE', #35758 ) ;
#22859 = DIRECTION ( 'NONE',  ( 0.000000000000000000, 0.000000000000000000, -1.000000000000000000 ) ) ;
#22860 = CARTESIAN_POINT ( 'NONE',  ( -73.00000337463100664, -43.30127018922202353, 12.50000000000000000 ) ) ;
#22861 = CARTESIAN_POINT ( 'NONE',  ( -39.27785635698568711, -86.50000000000001421, 32.50000000000000000 ) ) ;
#22862 = DIRECTION ( 'NONE',  ( 0.000000000000000000, 0.5000000000000011102, 0.8660254037844379305 ) ) ;
#22863 = ORIENTED_EDGE ( 'NONE', *, *, #29247, .F. ) ;
#22864 = EDGE_CURVE ( 'NONE', #9742, #17546, #32744, .T. ) ;
#22865 = FACE_BOUND ( 'NONE', #21884, .T. ) ;
#22866 = ORIENTED_EDGE ( 'NONE', *, *, #7480, .F. ) ;
#22867 = VERTEX_POINT ( 'NONE', #12495 ) ;
#22868 = EDGE_CURVE ( 'NONE', #33, #34040, #18443, .T. ) ;
#22869 = DIRECTION ( 'NONE',  ( 0.000000000000000000, 0.000000000000000000, 1.000000000000000000 ) ) ;
#22870 = ORIENTED_EDGE ( 'NONE', *, *, #23921, .F. ) ;
#22871 = DIRECTION ( 'NONE',  ( 0.000000000000000000, 0.000000000000000000, -1.000000000000000000 ) ) ;
#22872 = EDGE_CURVE ( 'NONE', #16595, #14001, #16063, .T. ) ;
#22873 = CYLINDRICAL_SURFACE ( 'NONE', #12836, 2.000000000000001776 ) ;
#22874 = AXIS2_PLACEMENT_3D ( 'NONE', #30200, #4533, #18973 ) ;
#22875 = CARTESIAN_POINT ( 'NONE',  ( -53.00000337463106348, 60.62177826491078747, 12.50000000000000000 ) ) ;
#22876 = ORIENTED_EDGE ( 'NONE', *, *, #16935, .F. ) ;
#22877 = VERTEX_POINT ( 'NONE', #4071 ) ;
#22878 = ADVANCED_FACE ( 'NONE', ( #27112 ), #7071, .F. ) ;
#22879 = EDGE_LOOP ( 'NONE', ( #36994, #25981 ) ) ;
#22880 = VERTEX_POINT ( 'NONE', #21121 ) ;
#22881 = EDGE_CURVE ( 'NONE', #10971, #6989, #10251, .T. ) ;
#22882 = VERTEX_POINT ( 'NONE', #9696 ) ;
#22883 = DIRECTION ( 'NONE',  ( 0.000000000000000000, 0.000000000000000000, 1.000000000000000000 ) ) ;
#22884 = FACE_OUTER_BOUND ( 'NONE', #15830, .T. ) ;
#22885 = FACE_OUTER_BOUND ( 'NONE', #18543, .T. ) ;
#22886 = DIRECTION ( 'NONE',  ( 1.000000000000000000, 0.000000000000000000, 0.000000000000000000 ) ) ;
#22887 = CARTESIAN_POINT ( 'NONE',  ( -95.00000000000000000, 0.000000000000000000, 17.49999999999999645 ) ) ;
#22888 = ORIENTED_EDGE ( 'NONE', *, *, #16993, .T. ) ;
#22889 = CARTESIAN_POINT ( 'NONE',  ( 63.10544158860312081, 59.98094972882071829, -5.000000000000000000 ) ) ;
#22890 = CARTESIAN_POINT ( 'NONE',  ( -80.00000337463096400, -34.64101615137762025, 17.49999999999999645 ) ) ;
#22891 = DIRECTION ( 'NONE',  ( 1.000000000000000000, 0.000000000000000000, 0.000000000000000000 ) ) ;
#22892 = ORIENTED_EDGE ( 'NONE', *, *, #2433, .F. ) ;
#22893 = DIRECTION ( 'NONE',  ( 0.000000000000000000, 0.000000000000000000, 1.000000000000000000 ) ) ;
#22894 = DIRECTION ( 'NONE',  ( 1.000000000000000000, 0.000000000000000000, 0.000000000000000000 ) ) ;
#22895 = ORIENTED_EDGE ( 'NONE', *, *, #29531, .T. ) ;
#22896 = ORIENTED_EDGE ( 'NONE', *, *, #7680, .T. ) ;
#22897 = ADVANCED_FACE ( 'NONE', ( #4262 ), #10423, .F. ) ;
#22898 = CARTESIAN_POINT ( 'NONE',  ( 37.50000000000000000, 103.4105893997321743, 18.49999999999999645 ) ) ;
#22899 = AXIS2_PLACEMENT_3D ( 'NONE', #24003, #919, #29796 ) ;
#22900 = CARTESIAN_POINT ( 'NONE',  ( -0.7030283904599151645, 5.367609061416117378, -4.096693167836310323 ) ) ;
#22901 = DIRECTION ( 'NONE',  ( 1.000000000000000000, 0.000000000000000000, 0.000000000000000000 ) ) ;
#22902 = CARTESIAN_POINT ( 'NONE',  ( -5.000000000000000888, -2.886751345948162406, -4.069520038198750633 ) ) ;
#22903 = EDGE_LOOP ( 'NONE', ( #21244, #1736 ) ) ;
#22904 = ORIENTED_EDGE ( 'NONE', *, *, #3325, .T. ) ;
#22905 = CARTESIAN_POINT ( 'NONE',  ( 31.99999662536856704, 69.28203230275518365, 17.49999999999999645 ) ) ;
#22906 = EDGE_CURVE ( 'NONE', #18966, #13116, #15691, .T. ) ;
#22907 = DIRECTION ( 'NONE',  ( 1.000000000000000000, 0.000000000000000000, 0.000000000000000000 ) ) ;
#22908 = DIRECTION ( 'NONE',  ( -1.000000000000000000, 0.000000000000000000, 0.000000000000000000 ) ) ;
#22909 = ORIENTED_EDGE ( 'NONE', *, *, #33529, .F. ) ;
#22910 = EDGE_CURVE ( 'NONE', #20554, #111, #13050, .T. ) ;
#22911 = EDGE_CURVE ( 'NONE', #14541, #20832, #21863, .T. ) ;
#22912 = CARTESIAN_POINT ( 'NONE',  ( 21.99999662536859191, 69.28203230275516944, -9.999999999999998224 ) ) ;
#22913 = ORIENTED_EDGE ( 'NONE', *, *, #10226, .F. ) ;
#22914 = ORIENTED_EDGE ( 'NONE', *, *, #639, .F. ) ;
#22915 = AXIS2_PLACEMENT_3D ( 'NONE', #30216, #35871, #18797 ) ;
#22916 = DIRECTION ( 'NONE',  ( 1.000000000000000000, 0.000000000000000000, 0.000000000000000000 ) ) ;
#22917 = DIRECTION ( 'NONE',  ( 0.000000000000000000, 0.000000000000000000, -1.000000000000000000 ) ) ;
#22918 = ORIENTED_EDGE ( 'NONE', *, *, #16304, .F. ) ;
#22919 = VERTEX_POINT ( 'NONE', #30110 ) ;
#22920 = CARTESIAN_POINT ( 'NONE',  ( 67.99999662536838230, -17.32050807568879947, -9.999999999999998224 ) ) ;
#22921 = DIRECTION ( 'NONE',  ( 0.000000000000000000, 0.000000000000000000, 1.000000000000000000 ) ) ;
#22922 = CARTESIAN_POINT ( 'NONE',  ( -70.00000337463099243, 51.96152422706637708, 12.50000000000000000 ) ) ;
#22923 = EDGE_CURVE ( 'NONE', #29025, #34519, #9477, .T. ) ;
#22924 = EDGE_LOOP ( 'NONE', ( #14381, #31611, #26718 ) ) ;
#22925 = FACE_OUTER_BOUND ( 'NONE', #2867, .T. ) ;
#22926 = AXIS2_PLACEMENT_3D ( 'NONE', #25468, #34798, #3484 ) ;
#22927 = FACE_BOUND ( 'NONE', #12192, .T. ) ;
#22928 = AXIS2_PLACEMENT_3D ( 'NONE', #21827, #36468, #19387 ) ;
#22929 = DIRECTION ( 'NONE',  ( -1.000000000000000000, 0.000000000000000000, 0.000000000000000000 ) ) ;
#22930 = DIRECTION ( 'NONE',  ( -0.4999999999999979461, 0.8660254037844397068, 0.000000000000000000 ) ) ;
#22931 = LINE ( 'NONE', #22372, #4547 ) ;
#22932 = DIRECTION ( 'NONE',  ( 1.000000000000000000, 0.000000000000000000, 0.000000000000000000 ) ) ;
#22933 = DIRECTION ( 'NONE',  ( 1.000000000000000000, 0.000000000000000000, 0.000000000000000000 ) ) ;
#22934 = DIRECTION ( 'NONE',  ( 1.000000000000000000, 0.000000000000000000, 0.000000000000000000 ) ) ;
#22935 = ORIENTED_EDGE ( 'NONE', *, *, #12852, .T. ) ;
#22936 = FACE_OUTER_BOUND ( 'NONE', #14803, .T. ) ;
#22937 = DIRECTION ( 'NONE',  ( 1.000000000000000000, 0.000000000000000000, -0.000000000000000000 ) ) ;
#22938 = CARTESIAN_POINT ( 'NONE',  ( 9.999996625368655856, -69.28203230275519786, -9.999999999999998224 ) ) ;
#22939 = ORIENTED_EDGE ( 'NONE', *, *, #33724, .T. ) ;
#22940 = VECTOR ( 'NONE', #9580, 1000.000000000000000 ) ;
#22941 = ORIENTED_EDGE ( 'NONE', *, *, #33520, .F. ) ;
#22942 = EDGE_CURVE ( 'NONE', #12253, #14986, #23845, .T. ) ;
#22943 = ORIENTED_EDGE ( 'NONE', *, *, #7349, .T. ) ;
#22944 = DIRECTION ( 'NONE',  ( 0.000000000000000000, 0.000000000000000000, -1.000000000000000000 ) ) ;
#22945 = DIRECTION ( 'NONE',  ( 1.000000000000000000, 0.000000000000000000, 0.000000000000000000 ) ) ;
#22946 = ADVANCED_FACE ( 'NONE', ( #21681 ), #27499, .T. ) ;
#22947 = DIRECTION ( 'NONE',  ( -0.000000000000000000, -0.000000000000000000, 1.000000000000000000 ) ) ;
#22948 = ORIENTED_EDGE ( 'NONE', *, *, #89, .T. ) ;
#22949 = EDGE_CURVE ( 'NONE', #4610, #21860, #7624, .T. ) ;
#22950 = DIRECTION ( 'NONE',  ( -0.000000000000000000, -0.000000000000000000, -1.000000000000000000 ) ) ;
#22951 = AXIS2_PLACEMENT_3D ( 'NONE', #14916, #30899, #5236 ) ;
#22952 = ORIENTED_EDGE ( 'NONE', *, *, #7390, .T. ) ;
#22953 = DIRECTION ( 'NONE',  ( 0.000000000000000000, 0.000000000000000000, 1.000000000000000000 ) ) ;
#22955 = ADVANCED_FACE ( 'NONE', ( #16256 ), #1067, .F. ) ;
#22954 = VERTEX_POINT ( 'NONE', #18874 ) ;
#22956 = DIRECTION ( 'NONE',  ( 0.000000000000000000, 0.000000000000000000, 1.000000000000000000 ) ) ;
#22957 = ORIENTED_EDGE ( 'NONE', *, *, #16218, .F. ) ;
#22958 = EDGE_CURVE ( 'NONE', #34330, #6458, #16675, .T. ) ;
#22959 = ORIENTED_EDGE ( 'NONE', *, *, #35614, .T. ) ;
#22960 = CARTESIAN_POINT ( 'NONE',  ( -38.00000337463113453, -69.28203230275519786, -9.999999999999998224 ) ) ;
#22961 = FACE_OUTER_BOUND ( 'NONE', #4271, .T. ) ;
#22962 = ORIENTED_EDGE ( 'NONE', *, *, #21758, .T. ) ;
#22963 = DIRECTION ( 'NONE',  ( 1.000000000000000000, 0.000000000000000000, 0.000000000000000000 ) ) ;
#22964 = AXIS2_PLACEMENT_3D ( 'NONE', #33832, #30642, #25393 ) ;
#22965 = ITEM_DEFINED_TRANSFORMATION ( 'NONE', 'NONE', #2784,  #21385 ) ;
#22966 = EDGE_CURVE ( 'NONE', #20246, #25464, #8307, .T. ) ;
#22967 = DIRECTION ( 'NONE',  ( -0.000000000000000000, 1.000000000000000000, 1.224646799147353207E-16 ) ) ;
#22968 = EDGE_CURVE ( 'NONE', #32425, #25770, #4718, .T. ) ;
#22969 = CARTESIAN_POINT ( 'NONE',  ( -68.00000337463099243, -2.428612866367529932E-14, -9.999999999999998224 ) ) ;
#22970 = VECTOR ( 'NONE', #8978, 1000.000000000000000 ) ;
#22971 = EDGE_CURVE ( 'NONE', #17289, #2363, #13075, .T. ) ;
#22972 = VERTEX_POINT ( 'NONE', #5729 ) ;
#22973 = DIRECTION ( 'NONE',  ( 1.000000000000000000, 0.000000000000000000, 0.000000000000000000 ) ) ;
#22974 = FACE_OUTER_BOUND ( 'NONE', #12172, .T. ) ;
#22975 = EDGE_CURVE ( 'NONE', #167, #21629, #34053, .T. ) ;
#22976 = ORIENTED_EDGE ( 'NONE', *, *, #1514, .F. ) ;
#22977 = DIRECTION ( 'NONE',  ( 0.5000000000000038858, 0.8660254037844362651, 0.000000000000000000 ) ) ;
#22978 = CARTESIAN_POINT ( 'NONE',  ( -58.00000337463104216, 34.64101615137757051, -9.999999999999998224 ) ) ;
#22979 = DIRECTION ( 'NONE',  ( -0.000000000000000000, -0.000000000000000000, -1.000000000000000000 ) ) ;
#22980 = DIRECTION ( 'NONE',  ( 0.000000000000000000, 0.000000000000000000, 1.000000000000000000 ) ) ;
#22981 = VECTOR ( 'NONE', #14093, 1000.000000000000114 ) ;
#22982 = AXIS2_PLACEMENT_3D ( 'NONE', #6615, #3976, #30031 ) ;
#22983 = VERTEX_POINT ( 'NONE', #8373 ) ;
#22984 = PLANE ( 'NONE',  #7603 ) ;
#22985 = DIRECTION ( 'NONE',  ( 0.000000000000000000, 0.000000000000000000, 1.000000000000000000 ) ) ;
#22986 = AXIS2_PLACEMENT_3D ( 'NONE', #7227, #1394, #14921 ) ;
#22987 = VERTEX_POINT ( 'NONE', #22068 ) ;
#22988 = ORIENTED_EDGE ( 'NONE', *, *, #33329, .T. ) ;
#22989 = VERTEX_POINT ( 'NONE', #19254 ) ;
#22990 = CARTESIAN_POINT ( 'NONE',  ( -106.7731239591675205, 98.28784258493143966, 32.55002500000000509 ) ) ;
#22991 = DIRECTION ( 'NONE',  ( 0.000000000000000000, 0.000000000000000000, 1.000000000000000000 ) ) ;
#22992 = LINE ( 'NONE', #34432, #36227 ) ;
#22993 = ORIENTED_EDGE ( 'NONE', *, *, #6361, .T. ) ;
#22994 = AXIS2_PLACEMENT_3D ( 'NONE', #31063, #34078, #19437 ) ;
#22995 = CARTESIAN_POINT ( 'NONE',  ( -55.00000337463107059, 43.30127018922197379, -9.999999999999998224 ) ) ;
#22996 = ORIENTED_EDGE ( 'NONE', *, *, #5235, .F. ) ;
#22997 = CYLINDRICAL_SURFACE ( 'NONE', #25126, 2.000000000000001776 ) ;
#22998 = ORIENTED_EDGE ( 'NONE', *, *, #4111, .T. ) ;
#22999 = FACE_OUTER_BOUND ( 'NONE', #16704, .T. ) ;
#23000 = AXIS2_PLACEMENT_3D ( 'NONE', #3958, #32061, #6398 ) ;
#23001 = CARTESIAN_POINT ( 'NONE',  ( 6.999996625368676284, -77.94228634059960825, 12.50000000000000000 ) ) ;
#23002 = CYLINDRICAL_SURFACE ( 'NONE', #23904, 3.750000000000001776 ) ;
#23003 = CARTESIAN_POINT ( 'NONE',  ( 0.000000000000000000, 0.000000000000000000, 0.000000000000000000 ) ) ;
#23004 = EDGE_CURVE ( 'NONE', #31031, #36783, #30668, .T. ) ;
#23005 = DIRECTION ( 'NONE',  ( 1.000000000000000000, 0.000000000000000000, 0.000000000000000000 ) ) ;
#23006 = DIRECTION ( 'NONE',  ( 0.000000000000000000, 0.000000000000000000, 1.000000000000000000 ) ) ;
#23007 = FACE_OUTER_BOUND ( 'NONE', #20424, .T. ) ;
#23008 = EDGE_CURVE ( 'NONE', #34191, #26481, #5379, .T. ) ;
#23009 = VERTEX_POINT ( 'NONE', #2725 ) ;
#23010 = DIRECTION ( 'NONE',  ( 0.000000000000000000, 0.000000000000000000, -1.000000000000000000 ) ) ;
#23011 = CARTESIAN_POINT ( 'NONE',  ( -35.00000337463116296, 77.94228634059957983, 12.50000000000000000 ) ) ;
#23012 = CARTESIAN_POINT ( 'NONE',  ( -50.00000337463109190, 51.96152422706637708, -5.000000000000000000 ) ) ;
#23013 = ORIENTED_EDGE ( 'NONE', *, *, #19551, .T. ) ;
#23014 = CIRCLE ( 'NONE', #8055, 2.000000000000001776 ) ;
#23015 = ORIENTED_EDGE ( 'NONE', *, *, #30558, .F. ) ;
#23016 = VERTEX_POINT ( 'NONE', #27670 ) ;
#23017 = VECTOR ( 'NONE', #17982, 1000.000000000000000 ) ;
#23018 = CARTESIAN_POINT ( 'NONE',  ( 9.999996625368618552, 69.28203230275516944, 17.49999999999999645 ) ) ;
#23019 = CIRCLE ( 'NONE', #6853, 2.000000000000001776 ) ;
#23020 = DIRECTION ( 'NONE',  ( 0.000000000000000000, 0.000000000000000000, 1.000000000000000000 ) ) ;
#23021 = DIRECTION ( 'NONE',  ( 0.000000000000000000, 0.000000000000000000, 1.000000000000000000 ) ) ;
#23022 = DIRECTION ( 'NONE',  ( 0.000000000000000000, 0.000000000000000000, 1.000000000000000000 ) ) ;
#23023 = CARTESIAN_POINT ( 'NONE',  ( -27.78182860042817026, -56.67878100130359087, 12.49999999999999822 ) ) ;
#23024 = EDGE_CURVE ( 'NONE', #27066, #17904, #27455, .T. ) ;
#23025 = DIRECTION ( 'NONE',  ( 0.000000000000000000, 0.000000000000000000, -1.000000000000000000 ) ) ;
#23026 = ADVANCED_FACE ( 'NONE', ( #5546 ), #36311, .F. ) ;
#23027 = VERTEX_POINT ( 'NONE', #19616 ) ;
#23028 = EDGE_LOOP ( 'NONE', ( #24555, #31763, #21489, #11190 ) ) ;
#23029 = CARTESIAN_POINT ( 'NONE',  ( -75.00000337463097821, -8.660254037844422825, -9.999999999999998224 ) ) ;
#23030 = AXIS2_PLACEMENT_3D ( 'NONE', #34510, #8817, #364 ) ;
#23031 = DIRECTION ( 'NONE',  ( 0.000000000000000000, 0.000000000000000000, 1.000000000000000000 ) ) ;
#23032 = CIRCLE ( 'NONE', #13441, 2.000000000000001776 ) ;
#23033 = CARTESIAN_POINT ( 'NONE',  ( 0.000000000000000000, -55.00000000000000000, 5.000000000000000888 ) ) ;
#23034 = ORIENTED_EDGE ( 'NONE', *, *, #14907, .F. ) ;
#23035 = EDGE_CURVE ( 'NONE', #8981, #8132, #21463, .T. ) ;
#23036 = FACE_BOUND ( 'NONE', #20343, .T. ) ;
#23037 = EDGE_LOOP ( 'NONE', ( #2082, #23048 ) ) ;
#23038 = ORIENTED_EDGE ( 'NONE', *, *, #18865, .F. ) ;
#23039 = DIRECTION ( 'NONE',  ( 0.000000000000000000, 0.000000000000000000, 1.000000000000000000 ) ) ;
#23040 = EDGE_LOOP ( 'NONE', ( #22346, #33953, #21137, #33727 ) ) ;
#23041 =( NAMED_UNIT ( * ) PLANE_ANGLE_UNIT ( ) SI_UNIT ( $, .RADIAN. ) );
#23042 = CIRCLE ( 'NONE', #22455, 150.0000000000000284 ) ;
#23043 = AXIS2_PLACEMENT_3D ( 'NONE', #33239, #30233, #7560 ) ;
#23044 = AXIS2_PLACEMENT_3D ( 'NONE', #20180, #16992, #287 ) ;
#23045 = DIRECTION ( 'NONE',  ( 1.000000000000000000, 0.000000000000000000, 0.000000000000000000 ) ) ;
#23046 = CARTESIAN_POINT ( 'NONE',  ( -68.00000337463102085, -51.96152422706641971, -9.999999999999998224 ) ) ;
#23047 = EDGE_CURVE ( 'NONE', #16018, #6451, #7706, .T. ) ;
#23048 = ORIENTED_EDGE ( 'NONE', *, *, #9994, .T. ) ;
#23049 = ORIENTED_EDGE ( 'NONE', *, *, #14653, .T. ) ;
#23050 = VERTEX_POINT ( 'NONE', #25619 ) ;
#23051 = ORIENTED_EDGE ( 'NONE', *, *, #36666, .T. ) ;
#23052 = ORIENTED_EDGE ( 'NONE', *, *, #14400, .F. ) ;
#23054 = DIRECTION ( 'NONE',  ( 0.000000000000000000, 0.000000000000000000, 1.000000000000000000 ) ) ;
#23053 = VECTOR ( 'NONE', #20997, 1000.000000000000000 ) ;
#23055 = AXIS2_PLACEMENT_3D ( 'NONE', #29694, #1218, #26158 ) ;
#23056 = DIRECTION ( 'NONE',  ( 1.000000000000000000, 0.000000000000000000, 0.000000000000000000 ) ) ;
#23057 = DIRECTION ( 'NONE',  ( 1.000000000000000000, 0.000000000000000000, 0.000000000000000000 ) ) ;
#23058 = DIRECTION ( 'NONE',  ( -0.000000000000000000, -0.000000000000000000, 1.000000000000000000 ) ) ;
#23059 = ORIENTED_EDGE ( 'NONE', *, *, #1825, .T. ) ;
#23060 = AXIS2_PLACEMENT_3D ( 'NONE', #28249, #21883, #17379 ) ;
#23061 = DIRECTION ( 'NONE',  ( 0.000000000000000000, 0.000000000000000000, 1.000000000000000000 ) ) ;
#23062 = CIRCLE ( 'NONE', #11071, 2.000000000000001776 ) ;
#23063 = DIRECTION ( 'NONE',  ( -0.000000000000000000, -0.000000000000000000, -1.000000000000000000 ) ) ;
#23064 = ADVANCED_FACE ( 'NONE', ( #7820 ), #37054, .F. ) ;
#23065 = DIRECTION ( 'NONE',  ( 0.000000000000000000, 0.000000000000000000, 1.000000000000000000 ) ) ;
#23066 = VERTEX_POINT ( 'NONE', #4987 ) ;
#23067 = LINE ( 'NONE', #2285, #35236 ) ;
#23068 = CARTESIAN_POINT ( 'NONE',  ( 23.49154088336464952, 103.5526315789473699, 32.50000000000000000 ) ) ;
#23069 = CIRCLE ( 'NONE', #9902, 2.000000000000001776 ) ;
#23070 = ORIENTED_EDGE ( 'NONE', *, *, #35469, .F. ) ;
#23071 = EDGE_LOOP ( 'NONE', ( #10104, #24542, #19197 ) ) ;
#23072 = FACE_OUTER_BOUND ( 'NONE', #20156, .T. ) ;
#23073 = PRODUCT_RELATED_PRODUCT_CATEGORY ( 'part', '', ( #37010 ) ) ;
#23074 = DIRECTION ( 'NONE',  ( 1.000000000000000000, 0.000000000000000000, 0.000000000000000000 ) ) ;
#23075 = DIRECTION ( 'NONE',  ( 1.000000000000000000, 0.000000000000000000, 0.000000000000000000 ) ) ;
#23076 = DIRECTION ( 'NONE',  ( 1.000000000000000000, 0.000000000000000000, 0.000000000000000000 ) ) ;
#23077 = EDGE_CURVE ( 'NONE', #30062, #8407, #11163, .T. ) ;
#23078 = ORIENTED_EDGE ( 'NONE', *, *, #6512, .T. ) ;
#23079 = CARTESIAN_POINT ( 'NONE',  ( -33.00000337463116296, 77.94228634059957983, -9.999999999999998224 ) ) ;
#23080 = DIRECTION ( 'NONE',  ( -0.000000000000000000, -0.000000000000000000, 1.000000000000000000 ) ) ;
#23081 = CARTESIAN_POINT ( 'NONE',  ( 17.99999662536861678, -86.60254037844400443, 17.49999999999999645 ) ) ;
#23082 = EDGE_CURVE ( 'NONE', #36051, #5822, #5307, .T. ) ;
#23083 = AXIS2_PLACEMENT_3D ( 'NONE', #24121, #10609, #16245 ) ;
#23084 = ORIENTED_EDGE ( 'NONE', *, *, #29292, .F. ) ;
#23085 = AXIS2_PLACEMENT_3D ( 'NONE', #16934, #31353, #22766 ) ;
#23086 = DIRECTION ( 'NONE',  ( 1.000000000000000000, 0.000000000000000000, 0.000000000000000000 ) ) ;
#23087 = ORIENTED_EDGE ( 'NONE', *, *, #32007, .F. ) ;
#23088 = AXIS2_PLACEMENT_3D ( 'NONE', #31813, #31451, #6144 ) ;
#23089 = AXIS2_PLACEMENT_3D ( 'NONE', #23684, #3799, #24440 ) ;
#23090 = CIRCLE ( 'NONE', #32057, 2.000000000000001776 ) ;
#23091 = VERTEX_POINT ( 'NONE', #8175 ) ;
#23092 = AXIS2_PLACEMENT_3D ( 'NONE', #8390, #31245, #5008 ) ;
#23093 = DIRECTION ( 'NONE',  ( 0.000000000000000000, 0.000000000000000000, 1.000000000000000000 ) ) ;
#23094 = CARTESIAN_POINT ( 'NONE',  ( -124.4080600076929954, 12.15049814296761888, 32.50000000000000000 ) ) ;
#23095 = ORIENTED_EDGE ( 'NONE', *, *, #4341, .T. ) ;
#23096 = ORIENTED_EDGE ( 'NONE', *, *, #19482, .T. ) ;
#23097 = DIRECTION ( 'NONE',  ( -1.000000000000000000, -0.000000000000000000, -0.000000000000000000 ) ) ;
#23098 = CARTESIAN_POINT ( 'NONE',  ( -84.88770934388888634, 10.65709906204123492, 12.50000000000000000 ) ) ;
#23099 = AXIS2_PLACEMENT_3D ( 'NONE', #28381, #33842, #36660 ) ;
#23100 = DIRECTION ( 'NONE',  ( 1.000000000000000000, 0.000000000000000000, 0.000000000000000000 ) ) ;
#23101 = ADVANCED_FACE ( 'NONE', ( #25417 ), #1984, .T. ) ;
#23102 = VERTEX_POINT ( 'NONE', #5179 ) ;
#23103 = DIRECTION ( 'NONE',  ( 1.000000000000000000, 0.000000000000000000, 0.000000000000000000 ) ) ;
#23104 = FACE_BOUND ( 'NONE', #9566, .T. ) ;
#23105 = CARTESIAN_POINT ( 'NONE',  ( 47.99999662536846756, 69.28203230275516944, -9.999999999999998224 ) ) ;
#23106 = CARTESIAN_POINT ( 'NONE',  ( 82.27241335952147949, -47.50000000000039790, 32.50002500000000083 ) ) ;
#23107 = DIRECTION ( 'NONE',  ( 0.000000000000000000, 0.000000000000000000, 1.000000000000000000 ) ) ;
#23108 = CARTESIAN_POINT ( 'NONE',  ( -75.00000337463097821, 25.98076211353318854, -9.999999999999998224 ) ) ;
#23109 = AXIS2_PLACEMENT_3D ( 'NONE', #12236, #35362, #31764 ) ;
#23110 = ADVANCED_FACE ( 'NONE', ( #10810 ), #7986, .F. ) ;
#23111 = LINE ( 'NONE', #29290, #7802 ) ;
#23112 = AXIS2_PLACEMENT_3D ( 'NONE', #2885, #14111, #19761 ) ;
#23113 = EDGE_CURVE ( 'NONE', #15730, #2540, #12477, .T. ) ;
#23114 = CARTESIAN_POINT ( 'NONE',  ( 84.99999662536831124, -8.660254037844397956, -9.999999999999998224 ) ) ;
#23115 = ORIENTED_EDGE ( 'NONE', *, *, #31258, .F. ) ;
#23117 = AXIS2_PLACEMENT_3D ( 'NONE', #8085, #22162, #13715 ) ;
#23116 = CARTESIAN_POINT ( 'NONE',  ( 101.4252628994511980, 31.43180897937319784, 32.50001250000000397 ) ) ;
#23118 =( GEOMETRIC_REPRESENTATION_CONTEXT ( 3 ) GLOBAL_UNCERTAINTY_ASSIGNED_CONTEXT ( ( #17039 ) ) GLOBAL_UNIT_ASSIGNED_CONTEXT ( ( #10504, #15247, #1005 ) ) REPRESENTATION_CONTEXT ( 'NONE', 'WORKASPACE' ) );
#23119 = CARTESIAN_POINT ( 'NONE',  ( 2.500000000000005773, 4.330127018922191873, -6.000000000000000000 ) ) ;
#23120 = DIRECTION ( 'NONE',  ( 0.000000000000000000, 0.000000000000000000, 1.000000000000000000 ) ) ;
#23121 = AXIS2_PLACEMENT_3D ( 'NONE', #21312, #21512, #12296 ) ;
#23122 = AXIS2_PLACEMENT_3D ( 'NONE', #24591, #13137, #7146 ) ;
#23123 = ORIENTED_EDGE ( 'NONE', *, *, #9681, .T. ) ;
#23124 = AXIS2_PLACEMENT_3D ( 'NONE', #13771, #64, #17128 ) ;
#23125 = ORIENTED_EDGE ( 'NONE', *, *, #55, .F. ) ;
#23126 = AXIS2_PLACEMENT_3D ( 'NONE', #8765, #28816, #3141 ) ;
#23127 = ORIENTED_EDGE ( 'NONE', *, *, #36133, .T. ) ;
#23128 = DIRECTION ( 'NONE',  ( 0.000000000000000000, 0.000000000000000000, 1.000000000000000000 ) ) ;
#23129 = CARTESIAN_POINT ( 'NONE',  ( 84.99999662536832545, 8.660254037844394404, 12.50000000000000000 ) ) ;
#23130 = DIRECTION ( 'NONE',  ( -1.000000000000000000, 0.000000000000000000, 0.000000000000000000 ) ) ;
#23131 = ORIENTED_EDGE ( 'NONE', *, *, #32909, .T. ) ;
#23132 = AXIS2_PLACEMENT_3D ( 'NONE', #22225, #5362, #16599 ) ;
#23133 = CARTESIAN_POINT ( 'NONE',  ( 29.99999662536856349, 69.28203230275518365, -9.999999999999998224 ) ) ;
#23134 = EDGE_CURVE ( 'NONE', #1955, #16077, #24470, .T. ) ;
#23135 = EDGE_LOOP ( 'NONE', ( #3633, #34694, #10664 ) ) ;
#23136 = CARTESIAN_POINT ( 'NONE',  ( 8.109924056054151009, -118.6579847640609131, 32.49999999999999289 ) ) ;
#23137 = ORIENTED_EDGE ( 'NONE', *, *, #36866, .T. ) ;
#23138 = DIRECTION ( 'NONE',  ( 0.000000000000000000, 0.000000000000000000, 1.000000000000000000 ) ) ;
#23139 = ORIENTED_EDGE ( 'NONE', *, *, #31979, .T. ) ;
#23140 = CIRCLE ( 'NONE', #13553, 2.000000000000001776 ) ;
#23141 = EDGE_LOOP ( 'NONE', ( #33132, #17584, #4482 ) ) ;
#23142 = DIRECTION ( 'NONE',  ( 0.000000000000000000, 0.000000000000000000, 1.000000000000000000 ) ) ;
#23143 = VECTOR ( 'NONE', #23058, 1000.000000000000000 ) ;
#23144 = CARTESIAN_POINT ( 'NONE',  ( -11.64413683707582337, -85.46375806488710225, -5.000000000000000000 ) ) ;
#23145 = ORIENTED_EDGE ( 'NONE', *, *, #18624, .F. ) ;
#23146 = PRODUCT_DEFINITION_FORMATION_WITH_SPECIFIED_SOURCE ( 'ANY', '', #160, .NOT_KNOWN. ) ;
#23147 = DIRECTION ( 'NONE',  ( 0.000000000000000000, -1.000000000000000000, 0.000000000000000000 ) ) ;
#23148 = VECTOR ( 'NONE', #13551, 1000.000000000000000 ) ;
#23149 = VECTOR ( 'NONE', #28056, 1000.000000000000000 ) ;
#23150 = AXIS2_PLACEMENT_3D ( 'NONE', #29098, #228, #8875 ) ;
#23151 = CYLINDRICAL_SURFACE ( 'NONE', #1294, 6.000000000000005329 ) ;
#23152 = DIRECTION ( 'NONE',  ( 1.000000000000000000, 0.000000000000000000, 0.000000000000000000 ) ) ;
#23153 = VECTOR ( 'NONE', #27671, 1000.000000000000000 ) ;
#23154 = EDGE_CURVE ( 'NONE', #31157, #8144, #2832, .T. ) ;
#23155 = ORIENTED_EDGE ( 'NONE', *, *, #20907, .F. ) ;
#23156 = CARTESIAN_POINT ( 'NONE',  ( -25.00000337463121980, -77.94228634059963667, -9.999999999999998224 ) ) ;
#23157 = CARTESIAN_POINT ( 'NONE',  ( -68.00000337463099243, 34.64101615137758472, 12.50000000000000000 ) ) ;
#23158 = EDGE_LOOP ( 'NONE', ( #1886, #21399 ) ) ;
#23159 = EDGE_CURVE ( 'NONE', #29874, #4566, #17906, .T. ) ;
#23160 = LINE ( 'NONE', #32333, #16637 ) ;
#23161 = DIRECTION ( 'NONE',  ( -0.000000000000000000, -0.000000000000000000, 1.000000000000000000 ) ) ;
#23162 = CARTESIAN_POINT ( 'NONE',  ( -8.000003374631281972, 86.60254037844397601, -9.999999999999998224 ) ) ;
#23163 = DIRECTION ( 'NONE',  ( 0.000000000000000000, 0.000000000000000000, 1.000000000000000000 ) ) ;
#23164 = AXIS2_PLACEMENT_3D ( 'NONE', #636, #28765, #32109 ) ;
#23165 = EDGE_CURVE ( 'NONE', #11237, #27568, #32228, .T. ) ;
#23166 = CARTESIAN_POINT ( 'NONE',  ( -83.67710216016716629, 27.48073957228723430, -5.000000000000000000 ) ) ;
#23167 = ORIENTED_EDGE ( 'NONE', *, *, #22726, .T. ) ;
#23168 = EDGE_CURVE ( 'NONE', #22827, #1125, #22668, .T. ) ;
#23169 = DIRECTION ( 'NONE',  ( -0.000000000000000000, -0.000000000000000000, 1.000000000000000000 ) ) ;
#23170 = CARTESIAN_POINT ( 'NONE',  ( -20.00000337463122690, 86.60254037844397601, 12.50000000000000000 ) ) ;
#23171 = ADVANCED_FACE ( 'NONE', ( #23711 ), #26348, .F. ) ;
#23172 = AXIS2_PLACEMENT_3D ( 'NONE', #18204, #9961, #29636 ) ;
#23173 = ORIENTED_EDGE ( 'NONE', *, *, #25257, .F. ) ;
#23174 = EDGE_LOOP ( 'NONE', ( #17995, #16566 ) ) ;
#23175 = ORIENTED_EDGE ( 'NONE', *, *, #9420, .F. ) ;
#23176 = AXIS2_PLACEMENT_3D ( 'NONE', #32601, #27360, #30352 ) ;
#23177 = AXIS2_PLACEMENT_3D ( 'NONE', #19909, #17097, #592 ) ;
#23178 = CARTESIAN_POINT ( 'NONE',  ( 24.99999662536857059, 77.94228634059957983, 17.49999999999999645 ) ) ;
#23179 = CARTESIAN_POINT ( 'NONE',  ( 12.99999662536863632, -77.94228634059960825, -5.000000000000000000 ) ) ;
#23180 = EDGE_CURVE ( 'NONE', #9210, #18862, #29336, .T. ) ;
#23181 = AXIS2_PLACEMENT_3D ( 'NONE', #15071, #17890, #17691 ) ;
#23182 = VECTOR ( 'NONE', #20070, 1000.000000000000000 ) ;
#23183 = EDGE_CURVE ( 'NONE', #6394, #10047, #1114, .T. ) ;
#23184 = VECTOR ( 'NONE', #25317, 1000.000000000000000 ) ;
#23185 = AXIS2_PLACEMENT_3D ( 'NONE', #23359, #34795, #8719 ) ;
#23186 = ADVANCED_FACE ( 'NONE', ( #17172 ), #23526, .T. ) ;
#23187 = CYLINDRICAL_SURFACE ( 'NONE', #14679, 2.000000000000001776 ) ;
#23189 = EDGE_CURVE ( 'NONE', #17979, #15624, #25671, .T. ) ;
#23188 = ORIENTED_EDGE ( 'NONE', *, *, #16075, .T. ) ;
#23190 = ADVANCED_FACE ( 'NONE', ( #6475 ), #31931, .F. ) ;
#23191 = CARTESIAN_POINT ( 'NONE',  ( -30.00000337463119848, -69.28203230275522628, -5.000000000000000000 ) ) ;
#23192 = VERTEX_POINT ( 'NONE', #34415 ) ;
#23193 = FACE_BOUND ( 'NONE', #23318, .T. ) ;
#23194 = AXIS2_PLACEMENT_3D ( 'NONE', #17951, #8763, #15307 ) ;
#23195 = VECTOR ( 'NONE', #9801, 1000.000000000000000 ) ;
#23196 = DIRECTION ( 'NONE',  ( 0.000000000000000000, 0.000000000000000000, 1.000000000000000000 ) ) ;
#23197 = CARTESIAN_POINT ( 'NONE',  ( 46.99999662536849598, -77.94228634059960825, 12.50000000000000000 ) ) ;
#23198 = DIRECTION ( 'NONE',  ( 0.000000000000000000, 0.000000000000000000, 1.000000000000000000 ) ) ;
#23199 = VECTOR ( 'NONE', #5502, 1000.000000000000114 ) ;
#23200 = DIRECTION ( 'NONE',  ( 0.000000000000000000, 0.000000000000000000, 1.000000000000000000 ) ) ;
#23201 = CIRCLE ( 'NONE', #36406, 2.000000000000001776 ) ;
#23202 = DIRECTION ( 'NONE',  ( 1.000000000000000000, 0.000000000000000000, 0.000000000000000000 ) ) ;
#23203 = DIRECTION ( 'NONE',  ( 0.000000000000000000, 0.000000000000000000, 1.000000000000000000 ) ) ;
#23204 = DIRECTION ( 'NONE',  ( 0.000000000000000000, 0.000000000000000000, 1.000000000000000000 ) ) ;
#23205 = EDGE_LOOP ( 'NONE', ( #16396, #29050, #25137, #15100 ) ) ;
#23206 = LINE ( 'NONE', #513, #19606 ) ;
#23207 = DIRECTION ( 'NONE',  ( 1.000000000000000000, 0.000000000000000000, 0.000000000000000000 ) ) ;
#23208 = CARTESIAN_POINT ( 'NONE',  ( 74.99999662536835388, -43.30127018922199511, -5.000000000000000000 ) ) ;
#23209 = EDGE_LOOP ( 'NONE', ( #17477, #18807, #21985, #9238 ) ) ;
#23210 = AXIS2_PLACEMENT_3D ( 'NONE', #10959, #2712, #30827 ) ;
#23211 = EDGE_LOOP ( 'NONE', ( #26579, #7845, #2601, #23434, #15838 ) ) ;
#23212 = EDGE_LOOP ( 'NONE', ( #19553, #27944, #11945, #6109 ) ) ;
#23213 = DIRECTION ( 'NONE',  ( 0.000000000000000000, 0.000000000000000000, 1.000000000000000000 ) ) ;
#23214 = AXIS2_PLACEMENT_3D ( 'NONE', #6270, #3475, #31586 ) ;
#23215 = FACE_BOUND ( 'NONE', #18064, .T. ) ;
#23216 = CIRCLE ( 'NONE', #14218, 2.000000000000001776 ) ;
#23217 = DIRECTION ( 'NONE',  ( -0.000000000000000000, -0.000000000000000000, 1.000000000000000000 ) ) ;
#23218 = CARTESIAN_POINT ( 'NONE',  ( 72.99999662536836809, -8.660254037844401509, -9.999999999999998224 ) ) ;
#23219 = FACE_OUTER_BOUND ( 'NONE', #22490, .T. ) ;
#23220 = VECTOR ( 'NONE', #17725, 1000.000000000000227 ) ;
#23221 = AXIS2_PLACEMENT_3D ( 'NONE', #36041, #1723, #30757 ) ;
#23222 = DIRECTION ( 'NONE',  ( 1.000000000000000000, 0.000000000000000000, 0.000000000000000000 ) ) ;
#23223 = EDGE_LOOP ( 'NONE', ( #23038, #10900, #27285, #12751 ) ) ;
#23224 = AXIS2_PLACEMENT_3D ( 'NONE', #26006, #34656, #693 ) ;
#23226 = ORIENTED_EDGE ( 'NONE', *, *, #11952, .T. ) ;
#23225 = ADVANCED_FACE ( 'NONE', ( #99 ), #34966, .F. ) ;
#23227 = CARTESIAN_POINT ( 'NONE',  ( -72.00000337463100664, 17.32050807568877460, 17.49999999999999645 ) ) ;
#23228 = LINE ( 'NONE', #31459, #22970 ) ;
#23229 = EDGE_CURVE ( 'NONE', #1926, #17193, #828, .T. ) ;
#23230 = DIRECTION ( 'NONE',  ( 0.000000000000000000, 0.000000000000000000, -1.000000000000000000 ) ) ;
#23231 = EDGE_LOOP ( 'NONE', ( #13865, #29942, #19269, #24306 ) ) ;
#23232 = VECTOR ( 'NONE', #27567, 1000.000000000000000 ) ;
#23233 = DIRECTION ( 'NONE',  ( 0.000000000000000000, 0.000000000000000000, 1.000000000000000000 ) ) ;
#23234 = EDGE_LOOP ( 'NONE', ( #1643, #24482, #22993, #3525 ) ) ;
#23235 = ORIENTED_EDGE ( 'NONE', *, *, #8918, .T. ) ;
#23236 = CARTESIAN_POINT ( 'NONE',  ( -4.279621169095561228, 62.97617850287782915, 12.49999999999999822 ) ) ;
#23237 = ORIENTED_EDGE ( 'NONE', *, *, #5015, .F. ) ;
#23238 = AXIS2_PLACEMENT_3D ( 'NONE', #5580, #8409, #34104 ) ;
#23239 = CARTESIAN_POINT ( 'NONE',  ( 59.99999662536842493, -51.96152422706639840, -5.000000000000000000 ) ) ;
#23240 = AXIS2_PLACEMENT_3D ( 'NONE', #12993, #1555, #10200 ) ;
#23241 = FACE_OUTER_BOUND ( 'NONE', #31446, .T. ) ;
#23242 = ORIENTED_EDGE ( 'NONE', *, *, #16983, .T. ) ;
#23243 = B_SPLINE_CURVE_WITH_KNOTS ( 'NONE', 3,
 ( #24499, #10606, #22048, #36491, #1970, #18677, #24858, #27658, #4974, #4423 ),
 .UNSPECIFIED., .F., .F.,
 ( 4, 2, 2, 2, 4 ),
 ( 0.000000000000000000, 0.001528561485809837349, 0.003057122971619674699, 0.004585684457429512265, 0.006114245943239349397 ),
 .UNSPECIFIED. ) ;
#23244 = VERTEX_POINT ( 'NONE', #20163 ) ;
#23245 = CIRCLE ( 'NONE', #33430, 5.000000000000000888 ) ;
#23246 = AXIS2_PLACEMENT_3D ( 'NONE', #35058, #9364, #32235 ) ;
#23247 = ORIENTED_EDGE ( 'NONE', *, *, #30072, .T. ) ;
#23248 = EDGE_CURVE ( 'NONE', #3582, #36402, #20771, .T. ) ;
#23249 = AXIS2_PLACEMENT_3D ( 'NONE', #4633, #16073, #19975 ) ;
#23250 = ORIENTED_EDGE ( 'NONE', *, *, #455, .T. ) ;
#23251 = EDGE_LOOP ( 'NONE', ( #2110, #8210, #29350, #33620 ) ) ;
#23252 = DIRECTION ( 'NONE',  ( -1.000000000000000000, 0.000000000000000000, 0.000000000000000000 ) ) ;
#23253 = DIRECTION ( 'NONE',  ( 0.4999999999999919509, -0.8660254037844432595, 0.000000000000000000 ) ) ;
#23254 = DIRECTION ( 'NONE',  ( 0.000000000000000000, 0.000000000000000000, 1.000000000000000000 ) ) ;
#23255 = CYLINDRICAL_SURFACE ( 'NONE', #1962, 150.0000000000000284 ) ;
#23256 = DIRECTION ( 'NONE',  ( 0.000000000000000000, 0.000000000000000000, 1.000000000000000000 ) ) ;
#23257 = AXIS2_PLACEMENT_3D ( 'NONE', #2095, #13529, #30973 ) ;
#23258 = ORIENTED_EDGE ( 'NONE', *, *, #23610, .F. ) ;
#23259 = CARTESIAN_POINT ( 'NONE',  ( 4.999996625368645198, 77.94228634059957983, -5.000000000000000000 ) ) ;
#23260 = ADVANCED_FACE ( 'NONE', ( #17360 ), #28782, .F. ) ;
#23261 = AXIS2_PLACEMENT_3D ( 'NONE', #36257, #24252, #30061 ) ;
#23262 = DIRECTION ( 'NONE',  ( 0.000000000000000000, 0.000000000000000000, 1.000000000000000000 ) ) ;
#23263 = CARTESIAN_POINT ( 'NONE',  ( 145.0000000000000284, -6.000000000000504485, 32.50000000000000000 ) ) ;
#23264 = VERTEX_POINT ( 'NONE', #31769 ) ;
#23265 = FACE_OUTER_BOUND ( 'NONE', #31178, .T. ) ;
#23266 = LINE ( 'NONE', #20267, #35157 ) ;
#23267 = CIRCLE ( 'NONE', #515, 2.000000000000001776 ) ;
#23268 = ORIENTED_EDGE ( 'NONE', *, *, #15104, .F. ) ;
#23269 = ORIENTED_EDGE ( 'NONE', *, *, #35933, .F. ) ;
#23270 = DIRECTION ( 'NONE',  ( -0.7650473262243671080, -0.6439740589782688707, -0.000000000000000000 ) ) ;
#23271 = VECTOR ( 'NONE', #27748, 1000.000000000000114 ) ;
#23272 = CARTESIAN_POINT ( 'NONE',  ( 74.99999662536836809, 25.98076211353319565, -9.999999999999998224 ) ) ;
#23273 = EDGE_CURVE ( 'NONE', #538, #22077, #30360, .T. ) ;
#23274 = CARTESIAN_POINT ( 'NONE',  ( -75.00000337463100664, -43.30127018922202353, 12.50000000000000000 ) ) ;
#23275 = CARTESIAN_POINT ( 'NONE',  ( 84.99999662536831124, -8.660254037844397956, -9.999999999999998224 ) ) ;
#23276 = ORIENTED_EDGE ( 'NONE', *, *, #16243, .T. ) ;
#23277 = VECTOR ( 'NONE', #11516, 1000.000000000000000 ) ;
#23278 = CYLINDRICAL_SURFACE ( 'NONE', #18341, 33.00000000000001421 ) ;
#23279 = CARTESIAN_POINT ( 'NONE',  ( -77.00000337463097821, -8.660254037844422825, -9.999999999999998224 ) ) ;
#23280 = LINE ( 'NONE', #36982, #11093 ) ;
#23281 = CIRCLE ( 'NONE', #3509, 2.000000000000001776 ) ;
#23282 = VERTEX_POINT ( 'NONE', #3275 ) ;
#23283 = AXIS2_PLACEMENT_3D ( 'NONE', #7961, #22786, #242 ) ;
#23284 = DIRECTION ( 'NONE',  ( -3.846960960290410782E-15, -1.000000000000000000, 0.000000000000000000 ) ) ;
#23285 = ORIENTED_EDGE ( 'NONE', *, *, #14217, .T. ) ;
#23286 = AXIS2_PLACEMENT_3D ( 'NONE', #34481, #26028, #17243 ) ;
#23287 = DIRECTION ( 'NONE',  ( 1.000000000000000000, 0.000000000000000000, 0.000000000000000000 ) ) ;
#23288 = AXIS2_PLACEMENT_3D ( 'NONE', #20462, #3607, #28895 ) ;
#23289 = CARTESIAN_POINT ( 'NONE',  ( 71.99999662536839651, -3.469446951953614189E-15, -9.999999999999998224 ) ) ;
#23290 = EDGE_CURVE ( 'NONE', #25177, #20566, #14712, .T. ) ;
#23291 = CARTESIAN_POINT ( 'NONE',  ( -95.00000000000001421, 1.163414459189985801E-14, -5.000000000000000000 ) ) ;
#23292 = VERTEX_POINT ( 'NONE', #29506 ) ;
#23293 = ORIENTED_EDGE ( 'NONE', *, *, #27980, .T. ) ;
#23294 = CARTESIAN_POINT ( 'NONE',  ( 86.99999662536832545, 25.98076211353319565, 12.50000000000000000 ) ) ;
#23295 = EDGE_CURVE ( 'NONE', #31156, #25326, #10017, .T. ) ;
#23296 = DIRECTION ( 'NONE',  ( -1.047444401652940007E-14, -1.000000000000000000, 0.000000000000000000 ) ) ;
#23297 = CARTESIAN_POINT ( 'NONE',  ( -3.000000000000000000, 0.000000000000000000, -5.974599999999999689 ) ) ;
#23298 = EDGE_LOOP ( 'NONE', ( #23332, #26601 ) ) ;
#23299 = CARTESIAN_POINT ( 'NONE',  ( 27.78182860042856461, 56.67878100130339902, -4.999999999999997335 ) ) ;
#23300 = AXIS2_PLACEMENT_3D ( 'NONE', #29780, #6724, #35435 ) ;
#23301 = FACE_BOUND ( 'NONE', #80, .T. ) ;
#23302 = ADVANCED_BREP_SHAPE_REPRESENTATION ( '', ( #31591, #21385 ), #11148 ) ;
#23303 = ADVANCED_FACE ( 'NONE', ( #30246 ), #9653, .T. ) ;
#23304 = AXIS2_PLACEMENT_3D ( 'NONE', #4293, #16113, #27702 ) ;
#23305 = DIRECTION ( 'NONE',  ( 0.000000000000000000, 0.000000000000000000, 1.000000000000000000 ) ) ;
#23306 = DIRECTION ( 'NONE',  ( 0.000000000000000000, 0.4999999999999941713, -0.8660254037844420383 ) ) ;
#23307 = DIRECTION ( 'NONE',  ( 1.000000000000000000, 0.000000000000000000, 0.000000000000000000 ) ) ;
#23308 = CARTESIAN_POINT ( 'NONE',  ( 72.99999662536836809, 8.660254037844394404, -9.999999999999998224 ) ) ;
#23309 = DIRECTION ( 'NONE',  ( 0.000000000000000000, 0.000000000000000000, 1.000000000000000000 ) ) ;
#23310 = EDGE_CURVE ( 'NONE', #28932, #32680, #17203, .T. ) ;
#23311 = CIRCLE ( 'NONE', #16736, 2.000000000000001776 ) ;
#23312 = DIRECTION ( 'NONE',  ( 0.8660254037844382635, -0.5000000000000006661, 0.000000000000000000 ) ) ;
#23313 = ORIENTED_EDGE ( 'NONE', *, *, #15713, .F. ) ;
#23314 = CARTESIAN_POINT ( 'NONE',  ( 11.64412580323855018, 85.46375187899521109, -5.000000000000000000 ) ) ;
#23315 = PLANE ( 'NONE',  #17738 ) ;
#23316 = DIRECTION ( 'NONE',  ( 1.000000000000000000, 0.000000000000000000, 0.000000000000000000 ) ) ;
#23317 = AXIS2_PLACEMENT_3D ( 'NONE', #36340, #13264, #25100 ) ;
#23318 = EDGE_LOOP ( 'NONE', ( #2534, #34872 ) ) ;
#23319 = EDGE_LOOP ( 'NONE', ( #25598, #9678, #13381, #2744 ) ) ;
#23320 = CIRCLE ( 'NONE', #18537, 2.000000000000001776 ) ;
#23321 = VERTEX_POINT ( 'NONE', #18469 ) ;
#23322 = FACE_OUTER_BOUND ( 'NONE', #9233, .T. ) ;
#23323 = ADVANCED_FACE ( 'NONE', ( #33070 ), #27073, .F. ) ;
#23324 = CARTESIAN_POINT ( 'NONE',  ( 93.36492675454790913, 17.14523346298246409, 12.49999999999999822 ) ) ;
#23325 = AXIS2_PLACEMENT_3D ( 'NONE', #6657, #14719, #26709 ) ;
#23326 = DIRECTION ( 'NONE',  ( -0.000000000000000000, -0.000000000000000000, -1.000000000000000000 ) ) ;
#23327 = ORIENTED_EDGE ( 'NONE', *, *, #15587, .T. ) ;
#23328 = CYLINDRICAL_SURFACE ( 'NONE', #11892, 2.000000000000001776 ) ;
#23329 = EDGE_CURVE ( 'NONE', #31662, #19701, #4663, .T. ) ;
#23330 = CIRCLE ( 'NONE', #15538, 2.000000000000001776 ) ;
#23331 = AXIS2_PLACEMENT_3D ( 'NONE', #31044, #27842, #13807 ) ;
#23332 = ORIENTED_EDGE ( 'NONE', *, *, #30114, .F. ) ;
#23333 = CARTESIAN_POINT ( 'NONE',  ( -23.49188638668713480, -103.5527587461262442, 32.50001250000000397 ) ) ;
#23334 = ORIENTED_EDGE ( 'NONE', *, *, #20963, .F. ) ;
#23335 = AXIS2_PLACEMENT_3D ( 'NONE', #28437, #28262, #31085 ) ;
#23336 = FACE_OUTER_BOUND ( 'NONE', #633, .T. ) ;
#23337 = ORIENTED_EDGE ( 'NONE', *, *, #9423, .T. ) ;
#23338 = ORIENTED_EDGE ( 'NONE', *, *, #13569, .F. ) ;
#23339 = ADVANCED_FACE ( 'NONE', ( #4222 ), #27451, .T. ) ;
#23340 = CARTESIAN_POINT ( 'NONE',  ( 39.99999662536853151, 69.28203230275518365, 17.49999999999999645 ) ) ;
#23341 = DIRECTION ( 'NONE',  ( -1.000000000000000000, 0.000000000000000000, -0.000000000000000000 ) ) ;
#23342 = ADVANCED_FACE ( 'NONE', ( #21078 ), #1382, .F. ) ;
#23343 = DIRECTION ( 'NONE',  ( -1.000000000000000000, 0.000000000000000000, 0.000000000000000000 ) ) ;
#23344 =( REPRESENTATION_RELATIONSHIP ('NONE','NONE', #15268, #33015 ) REPRESENTATION_RELATIONSHIP_WITH_TRANSFORMATION ( #22599 )SHAPE_REPRESENTATION_RELATIONSHIP( ) );
#23345 = VERTEX_POINT ( 'NONE', #18831 ) ;
#23346 = CARTESIAN_POINT ( 'NONE',  ( 104.8061974404898820, 19.22934205794938478, 32.50000000000000000 ) ) ;
#23347 = AXIS2_PLACEMENT_3D ( 'NONE', #24673, #10403, #33283 ) ;
#23348 = DIRECTION ( 'NONE',  ( 0.000000000000000000, 0.000000000000000000, 1.000000000000000000 ) ) ;
#23349 = CARTESIAN_POINT ( 'NONE',  ( 81.99999662536832545, -17.32050807568879591, -9.999999999999998224 ) ) ;
#23350 = ORIENTED_EDGE ( 'NONE', *, *, #6074, .T. ) ;
#23351 = CARTESIAN_POINT ( 'NONE',  ( 0.000000000000000000, 0.000000000000000000, 12.49999999999999822 ) ) ;
#23352 = CYLINDRICAL_SURFACE ( 'NONE', #2993, 2.000000000000001776 ) ;
#23353 = EDGE_LOOP ( 'NONE', ( #7409, #25689, #20444 ) ) ;
#23354 = AXIS2_PLACEMENT_3D ( 'NONE', #9613, #24045, #30206 ) ;
#23355 = DIRECTION ( 'NONE',  ( 0.000000000000000000, 0.000000000000000000, 1.000000000000000000 ) ) ;
#23356 = ADVANCED_FACE ( 'NONE', ( #15821 ), #21459, .F. ) ;
#23357 = CARTESIAN_POINT ( 'NONE',  ( -50.00000337463112032, -51.96152422706641971, -9.999999999999998224 ) ) ;
#23358 = CIRCLE ( 'NONE', #4788, 2.000000000000000000 ) ;
#23359 = CARTESIAN_POINT ( 'NONE',  ( -35.00000337463116296, -60.62177826491080168, -9.999999999999998224 ) ) ;
#23360 = DIRECTION ( 'NONE',  ( 1.000000000000000000, 0.000000000000000000, 0.000000000000000000 ) ) ;
#23361 = CARTESIAN_POINT ( 'NONE',  ( -5.000003374631269537, -77.94228634059960825, 12.50000000000000000 ) ) ;
#23362 = EDGE_CURVE ( 'NONE', #32711, #33803, #20801, .T. ) ;
#23363 = AXIS2_PLACEMENT_3D ( 'NONE', #9137, #4090, #20962 ) ;
#23364 = DIRECTION ( 'NONE',  ( 0.000000000000000000, 0.000000000000000000, 1.000000000000000000 ) ) ;
#23365 = ORIENTED_EDGE ( 'NONE', *, *, #16117, .T. ) ;
#23366 = DIRECTION ( 'NONE',  ( 0.000000000000000000, 0.000000000000000000, 1.000000000000000000 ) ) ;
#23367 = AXIS2_PLACEMENT_3D ( 'NONE', #17355, #19802, #11350 ) ;
#23368 = FACE_OUTER_BOUND ( 'NONE', #17450, .T. ) ;
#23369 = DIRECTION ( 'NONE',  ( -1.000000000000000000, 0.000000000000000000, 0.000000000000000000 ) ) ;
#23370 = ORIENTED_EDGE ( 'NONE', *, *, #28161, .F. ) ;
#23371 = EDGE_LOOP ( 'NONE', ( #23901, #20588, #23188, #22614 ) ) ;
#23372 = ORIENTED_EDGE ( 'NONE', *, *, #21758, .F. ) ;
#23373 = DIRECTION ( 'NONE',  ( 1.000000000000000000, 0.000000000000000000, 0.000000000000000000 ) ) ;
#23374 = DIRECTION ( 'NONE',  ( 1.000000000000000000, 0.000000000000000000, 0.000000000000000000 ) ) ;
#23375 = CARTESIAN_POINT ( 'NONE',  ( 47.63139720814418610, 27.49999999999988987, -10.00000000000000178 ) ) ;
#23376 = AXIS2_PLACEMENT_3D ( 'NONE', #36743, #10314, #2052 ) ;
#23377 = EDGE_CURVE ( 'NONE', #20832, #13259, #21401, .T. ) ;
#23378 = CARTESIAN_POINT ( 'NONE',  ( -38.00000337463113453, 69.28203230275516944, -9.999999999999998224 ) ) ;
#23379 = ORIENTED_EDGE ( 'NONE', *, *, #4087, .F. ) ;
#23380 = CIRCLE ( 'NONE', #616, 2.000000000000001776 ) ;
#23381 = LINE ( 'NONE', #850, #24529 ) ;
#23382 = ORIENTED_EDGE ( 'NONE', *, *, #31954, .F. ) ;
#23384 = AXIS2_PLACEMENT_3D ( 'NONE', #24737, #35999, #16669 ) ;
#23383 = FACE_BOUND ( 'NONE', #25107, .T. ) ;
#23385 = EDGE_CURVE ( 'NONE', #33080, #36512, #1652, .T. ) ;
#23386 = CARTESIAN_POINT ( 'NONE',  ( 41.99999662536853151, 69.28203230275518365, -9.999999999999998224 ) ) ;
#23387 = EDGE_CURVE ( 'NONE', #2049, #20372, #10378, .T. ) ;
#23388 = DIRECTION ( 'NONE',  ( 0.000000000000000000, 0.000000000000000000, 1.000000000000000000 ) ) ;
#23389 = EDGE_CURVE ( 'NONE', #12717, #13311, #434, .T. ) ;
#23390 = VERTEX_POINT ( 'NONE', #12636 ) ;
#23391 = DIRECTION ( 'NONE',  ( 0.000000000000000000, 0.000000000000000000, 1.000000000000000000 ) ) ;
#23392 = CARTESIAN_POINT ( 'NONE',  ( -47.63139720814419320, 27.49999999999989697, -16.00000000000000000 ) ) ;
#23393 = DIRECTION ( 'NONE',  ( 0.000000000000000000, 0.000000000000000000, -1.000000000000000000 ) ) ;
#23394 = FACE_OUTER_BOUND ( 'NONE', #7102, .T. ) ;
#23395 = CARTESIAN_POINT ( 'NONE',  ( 0.000000000000000000, 1.467624384280029615, 2.541999999999997151 ) ) ;
#23396 = ORIENTED_EDGE ( 'NONE', *, *, #32863, .T. ) ;
#23397 = CARTESIAN_POINT ( 'NONE',  ( 76.99999662536835388, -25.98076211353319565, 12.50000000000000000 ) ) ;
#23398 = CARTESIAN_POINT ( 'NONE',  ( 20.00000000000001066, 89.94802294027088863, 27.49999999999999645 ) ) ;
#23399 = DIRECTION ( 'NONE',  ( 1.000000000000000000, 0.000000000000000000, 0.000000000000000000 ) ) ;
#23400 = ORIENTED_EDGE ( 'NONE', *, *, #33414, .T. ) ;
#23401 = VERTEX_POINT ( 'NONE', #24084 ) ;
#23402 = EDGE_CURVE ( 'NONE', #8483, #32886, #35528, .T. ) ;
#23403 = AXIS2_PLACEMENT_3D ( 'NONE', #6320, #22669, #28452 ) ;
#23404 = ORIENTED_EDGE ( 'NONE', *, *, #8740, .F. ) ;
#23405 = DIRECTION ( 'NONE',  ( -1.000000000000000000, 0.000000000000000000, 0.000000000000000000 ) ) ;
#23406 = DIRECTION ( 'NONE',  ( 1.000000000000000000, 0.000000000000000000, 0.000000000000000000 ) ) ;
#23407 = CARTESIAN_POINT ( 'NONE',  ( 62.97617850287784336, 4.279621169095339184, -4.999999999999997335 ) ) ;
#23408 = CARTESIAN_POINT ( 'NONE',  ( 68.66839587347284635, 56.74224907228958870, -4.999999999999997335 ) ) ;
#23409 = DIRECTION ( 'NONE',  ( 0.000000000000000000, 0.000000000000000000, -1.000000000000000000 ) ) ;
#23410 = CARTESIAN_POINT ( 'NONE',  ( 87.99999662536828282, 2.449293598294703949E-16, 17.49999999999999645 ) ) ;
#23411 = ORIENTED_EDGE ( 'NONE', *, *, #23552, .T. ) ;
#23412 = ORIENTED_EDGE ( 'NONE', *, *, #33856, .T. ) ;
#23413 = DIRECTION ( 'NONE',  ( 1.000000000000000000, 0.000000000000000000, 0.000000000000000000 ) ) ;
#23414 = EDGE_CURVE ( 'NONE', #27264, #23728, #32694, .T. ) ;
#23415 = CARTESIAN_POINT ( 'NONE',  ( -2.778182860042071933, 69.13212189986968781, -4.999999999999997335 ) ) ;
#23416 = EDGE_CURVE ( 'NONE', #28072, #15480, #12418, .T. ) ;
#23417 = FACE_OUTER_BOUND ( 'NONE', #2257, .T. ) ;
#23418 = ORIENTED_EDGE ( 'NONE', *, *, #33529, .T. ) ;
#23419 = FACE_BOUND ( 'NONE', #17222, .T. ) ;
#23420 = ORIENTED_EDGE ( 'NONE', *, *, #8641, .F. ) ;
#23421 = EDGE_LOOP ( 'NONE', ( #14329, #13879, #19178, #33743 ) ) ;
#23422 = AXIS2_PLACEMENT_3D ( 'NONE', #29948, #35586, #32953 ) ;
#23423 = EDGE_CURVE ( 'NONE', #9029, #21384, #5245, .T. ) ;
#23424 = DIRECTION ( 'NONE',  ( -0.000000000000000000, -0.000000000000000000, 1.000000000000000000 ) ) ;
#23425 = ORIENTED_EDGE ( 'NONE', *, *, #19716, .T. ) ;
#23426 = DIRECTION ( 'NONE',  ( 1.000000000000000000, 0.000000000000000000, 0.000000000000000000 ) ) ;
#23427 = CARTESIAN_POINT ( 'NONE',  ( 44.99999662536849598, 60.62177826491077326, -9.999999999999998224 ) ) ;
#23428 = DIRECTION ( 'NONE',  ( 1.000000000000000000, 0.000000000000000000, 0.000000000000000000 ) ) ;
#23429 = VERTEX_POINT ( 'NONE', #36261 ) ;
#23430 = ORIENTED_EDGE ( 'NONE', *, *, #24225, .T. ) ;
#23431 = EDGE_CURVE ( 'NONE', #36358, #15508, #8241, .T. ) ;
#23432 = ORIENTED_EDGE ( 'NONE', *, *, #16584, .T. ) ;
#23433 = EDGE_CURVE ( 'NONE', #33197, #33432, #2240, .T. ) ;
#23434 = ORIENTED_EDGE ( 'NONE', *, *, #25069, .F. ) ;
#23435 = ORIENTED_EDGE ( 'NONE', *, *, #14783, .F. ) ;
#23436 = EDGE_CURVE ( 'NONE', #16067, #22858, #5130, .T. ) ;
#23437 = CARTESIAN_POINT ( 'NONE',  ( 67.99999662536838230, -3.224517592124143893E-15, -9.999999999999998224 ) ) ;
#23438 = ADVANCED_FACE ( 'NONE', ( #33640 ), #7770, .F. ) ;
#23439 = EDGE_LOOP ( 'NONE', ( #14619, #14799, #25682, #18410 ) ) ;
#23440 = CIRCLE ( 'NONE', #21025, 2.000000000000000000 ) ;
#23441 = CARTESIAN_POINT ( 'NONE',  ( 1.999996625368696490, -86.60254037844400443, -9.999999999999998224 ) ) ;
#23442 = DIRECTION ( 'NONE',  ( 1.000000000000000000, 0.000000000000000000, 0.000000000000000000 ) ) ;
#23443 = DIRECTION ( 'NONE',  ( 1.000000000000000000, 0.000000000000000000, 0.000000000000000000 ) ) ;
#23444 = VERTEX_POINT ( 'NONE', #27629 ) ;
#23445 = DIRECTION ( 'NONE',  ( 0.000000000000000000, 0.000000000000000000, -1.000000000000000000 ) ) ;
#23446 = LINE ( 'NONE', #34884, #2422 ) ;
#23447 = CARTESIAN_POINT ( 'NONE',  ( -65.00000337463102085, 25.98076211353317433, 12.50000000000000000 ) ) ;
#23448 = ORIENTED_EDGE ( 'NONE', *, *, #12393, .F. ) ;
#23449 = CARTESIAN_POINT ( 'NONE',  ( -30.00000337463119848, -69.28203230275522628, -9.999999999999998224 ) ) ;
#23450 = CARTESIAN_POINT ( 'NONE',  ( -63.00000337463104927, -25.98076211353322051, -9.999999999999998224 ) ) ;
#23451 = EDGE_LOOP ( 'NONE', ( #5363, #18063 ) ) ;
#23452 = ORIENTED_EDGE ( 'NONE', *, *, #15836, .F. ) ;
#23453 = DIRECTION ( 'NONE',  ( 0.000000000000000000, 0.000000000000000000, -1.000000000000000000 ) ) ;
#23454 = DIRECTION ( 'NONE',  ( 0.000000000000000000, 0.000000000000000000, -1.000000000000000000 ) ) ;
#23455 = DIRECTION ( 'NONE',  ( 0.000000000000000000, 0.000000000000000000, -1.000000000000000000 ) ) ;
#23456 = CARTESIAN_POINT ( 'NONE',  ( -4.999999999999999112, 2.059541880721995177, -1.329159518034682685 ) ) ;
#23457 = ORIENTED_EDGE ( 'NONE', *, *, #15967, .T. ) ;
#23458 = EDGE_CURVE ( 'NONE', #29705, #22787, #24825, .T. ) ;
#23459 = CARTESIAN_POINT ( 'NONE',  ( -68.00000337463099243, 34.64101615137758472, -9.999999999999998224 ) ) ;
#23460 = CARTESIAN_POINT ( 'NONE',  ( -78.00000337463094979, 17.32050807568878525, 17.49999999999999645 ) ) ;
#23461 = FACE_OUTER_BOUND ( 'NONE', #5012, .T. ) ;
#23462 = ORIENTED_EDGE ( 'NONE', *, *, #36536, .T. ) ;
#23463 = VECTOR ( 'NONE', #30443, 1000.000000000000000 ) ;
#23464 = CIRCLE ( 'NONE', #12665, 2.000000000000001776 ) ;
#23465 = DIRECTION ( 'NONE',  ( 1.000000000000000000, 0.000000000000000000, 0.000000000000000000 ) ) ;
#23466 = EDGE_LOOP ( 'NONE', ( #21308, #35137, #12364, #12115 ) ) ;
#23467 = LINE ( 'NONE', #15401, #5736 ) ;
#23468 = CARTESIAN_POINT ( 'NONE',  ( 44.99999662536849598, 60.62177826491077326, 17.49999999999999645 ) ) ;
#23469 = CARTESIAN_POINT ( 'NONE',  ( -101.7384897088135887, 110.2237710830547286, 32.55002500000000509 ) ) ;
#23470 = ORIENTED_EDGE ( 'NONE', *, *, #30741, .T. ) ;
#23471 = VERTEX_POINT ( 'NONE', #11313 ) ;
#23472 = CARTESIAN_POINT ( 'NONE',  ( 74.99999662536835388, -25.98076211353319565, 17.49999999999999645 ) ) ;
#23473 = DIRECTION ( 'NONE',  ( 1.000000000000000000, 0.000000000000000000, 0.000000000000000000 ) ) ;
#23474 = DIRECTION ( 'NONE',  ( -1.000000000000000000, 0.000000000000000000, 0.000000000000000000 ) ) ;
#23475 = ORIENTED_EDGE ( 'NONE', *, *, #15491, .T. ) ;
#23476 = DIRECTION ( 'NONE',  ( 0.000000000000000000, 0.000000000000000000, 1.000000000000000000 ) ) ;
#23477 = EDGE_CURVE ( 'NONE', #33271, #20440, #7031, .T. ) ;
#23478 = FACE_BOUND ( 'NONE', #19955, .T. ) ;
#23479 = DIRECTION ( 'NONE',  ( 0.000000000000000000, 0.000000000000000000, 1.000000000000000000 ) ) ;
#23480 = CARTESIAN_POINT ( 'NONE',  ( 27.99999662536855993, 69.28203230275518365, 12.50000000000000000 ) ) ;
#23481 = DIRECTION ( 'NONE',  ( -1.000000000000000000, 0.000000000000000000, 0.000000000000000000 ) ) ;
#23482 = ORIENTED_EDGE ( 'NONE', *, *, #10957, .T. ) ;
#23483 = DIRECTION ( 'NONE',  ( -1.000000000000000000, 0.000000000000000000, -0.000000000000000000 ) ) ;
#23484 = CARTESIAN_POINT ( 'NONE',  ( 49.99999662536846756, 69.28203230275516944, -9.999999999999998224 ) ) ;
#23485 = AXIS2_PLACEMENT_3D ( 'NONE', #411, #5877, #2505 ) ;
#23486 = DIRECTION ( 'NONE',  ( 1.000000000000000000, 0.000000000000000000, 0.000000000000000000 ) ) ;
#23487 = EDGE_LOOP ( 'NONE', ( #4197, #19866, #25190, #26668, #36243, #25669 ) ) ;
#23488 = CYLINDRICAL_SURFACE ( 'NONE', #25624, 2.000000000000001776 ) ;
#23489 = CARTESIAN_POINT ( 'NONE',  ( 81.99999662536833966, 17.32050807568879236, -9.999999999999998224 ) ) ;
#23490 = CARTESIAN_POINT ( 'NONE',  ( 3.000000000000000000, -1.467624384280027172, 2.542000000000001592 ) ) ;
#23491 = ORIENTED_EDGE ( 'NONE', *, *, #31226, .F. ) ;
#23492 = EDGE_LOOP ( 'NONE', ( #16225, #8204, #7823, #5457 ) ) ;
#23493 = ORIENTED_EDGE ( 'NONE', *, *, #2444, .T. ) ;
#23494 = DIRECTION ( 'NONE',  ( 0.000000000000000000, 0.000000000000000000, 1.000000000000000000 ) ) ;
#23495 = FACE_OUTER_BOUND ( 'NONE', #28813, .T. ) ;
#23496 = DIRECTION ( 'NONE',  ( 0.000000000000000000, 0.000000000000000000, -1.000000000000000000 ) ) ;
#23497 = ORIENTED_EDGE ( 'NONE', *, *, #681, .F. ) ;
#23498 = ORIENTED_EDGE ( 'NONE', *, *, #19497, .T. ) ;
#23499 = EDGE_CURVE ( 'NONE', #7111, #36249, #9441, .T. ) ;
#23500 = CIRCLE ( 'NONE', #7339, 2.000000000000001776 ) ;
#23501 = DIRECTION ( 'NONE',  ( -1.000000000000000000, 0.000000000000000000, 0.000000000000000000 ) ) ;
#23502 = AXIS2_PLACEMENT_3D ( 'NONE', #29861, #24798, #35500 ) ;
#23503 = ORIENTED_EDGE ( 'NONE', *, *, #12726, .T. ) ;
#23504 = DIRECTION ( 'NONE',  ( 1.000000000000000000, 0.000000000000000000, 0.000000000000000000 ) ) ;
#23505 = EDGE_CURVE ( 'NONE', #4760, #105, #35202, .T. ) ;
#23506 = VERTEX_POINT ( 'NONE', #19214 ) ;
#23507 = CARTESIAN_POINT ( 'NONE',  ( -75.00000337463097821, 43.30127018922197379, -9.999999999999998224 ) ) ;
#23508 = ORIENTED_EDGE ( 'NONE', *, *, #35810, .F. ) ;
#23509 = ORIENTED_EDGE ( 'NONE', *, *, #30648, .F. ) ;
#23510 = EDGE_CURVE ( 'NONE', #8606, #16595, #8125, .T. ) ;
#23511 = DIRECTION ( 'NONE',  ( -0.000000000000000000, -0.000000000000000000, 1.000000000000000000 ) ) ;
#23512 = DIRECTION ( 'NONE',  ( 0.000000000000000000, 0.000000000000000000, 1.000000000000000000 ) ) ;
#23513 = FACE_OUTER_BOUND ( 'NONE', #35302, .T. ) ;
#23514 = ORIENTED_EDGE ( 'NONE', *, *, #31535, .T. ) ;
#23515 = VERTEX_POINT ( 'NONE', #37005 ) ;
#23516 = LINE ( 'NONE', #14698, #4116 ) ;
#23517 = ITEM_DEFINED_TRANSFORMATION ( 'NONE', 'NONE', #14762,  #21385 ) ;
#23518 = DIRECTION ( 'NONE',  ( 0.000000000000000000, 0.000000000000000000, 1.000000000000000000 ) ) ;
#23519 = CARTESIAN_POINT ( 'NONE',  ( -5.236971957347722473, 1.063004708247950125, -4.059261105226032562 ) ) ;
#23520 = ORIENTED_EDGE ( 'NONE', *, *, #11211, .F. ) ;
#23521 = DIRECTION ( 'NONE',  ( 1.000000000000000000, 0.000000000000000000, 0.000000000000000000 ) ) ;
#23522 = CARTESIAN_POINT ( 'NONE',  ( -20.00000337463123756, -69.28203230275522628, 12.50000000000000000 ) ) ;
#23523 = EDGE_LOOP ( 'NONE', ( #15805, #18871, #26669, #1183 ) ) ;
#23524 = EDGE_CURVE ( 'NONE', #19449, #5559, #31558, .T. ) ;
#23525 = CARTESIAN_POINT ( 'NONE',  ( 31.99999662536857770, -69.28203230275519786, 12.50000000000000000 ) ) ;
#23526 = CYLINDRICAL_SURFACE ( 'NONE', #14872, 3.000000000000002665 ) ;
#23527 = DIRECTION ( 'NONE',  ( 0.000000000000000000, 0.000000000000000000, 1.000000000000000000 ) ) ;
#23528 = CARTESIAN_POINT ( 'NONE',  ( -43.00000337463111322, -77.94228634059960825, -9.999999999999998224 ) ) ;
#23529 = AXIS2_PLACEMENT_3D ( 'NONE', #14460, #12164, #17621 ) ;
#23530 = CARTESIAN_POINT ( 'NONE',  ( 52.39915983220795681, 35.19434990244919703, 12.49999999999999822 ) ) ;
#23531 = CARTESIAN_POINT ( 'NONE',  ( 84.99999662536831124, -25.98076211353319565, 12.50000000000000000 ) ) ;
#23532 = ORIENTED_EDGE ( 'NONE', *, *, #5205, .F. ) ;
#23533 = DIRECTION ( 'NONE',  ( -1.000000000000000000, 0.000000000000000000, 0.000000000000000000 ) ) ;
#23534 = DIRECTION ( 'NONE',  ( 0.000000000000000000, 0.000000000000000000, 1.000000000000000000 ) ) ;
#23535 = CARTESIAN_POINT ( 'NONE',  ( 1.999996625368672287, 86.60254037844397601, -9.999999999999998224 ) ) ;
#23536 = ORIENTED_EDGE ( 'NONE', *, *, #36156, .T. ) ;
#23537 = VERTEX_POINT ( 'NONE', #10765 ) ;
#23538 = ORIENTED_EDGE ( 'NONE', *, *, #4175, .F. ) ;
#23539 = EDGE_CURVE ( 'NONE', #22150, #3127, #16032, .T. ) ;
#23540 = SURFACE_SIDE_STYLE ('',( #3291 ) ) ;
#23541 = DIRECTION ( 'NONE',  ( 0.000000000000000000, 0.000000000000000000, -1.000000000000000000 ) ) ;
#23542 = DIRECTION ( 'NONE',  ( -1.000000000000000000, 0.000000000000000000, 0.000000000000000000 ) ) ;
#23543 = CARTESIAN_POINT ( 'NONE',  ( -51.13139720814380951, 27.50000000000055422, -15.00000000000000000 ) ) ;
#23544 = DIRECTION ( 'NONE',  ( 1.000000000000000000, 0.000000000000000000, 0.000000000000000000 ) ) ;
#23545 = EDGE_LOOP ( 'NONE', ( #15435, #23127, #21841, #22823 ) ) ;
#23546 = DIRECTION ( 'NONE',  ( 0.000000000000000000, 0.000000000000000000, 1.000000000000000000 ) ) ;
#23547 = EDGE_CURVE ( 'NONE', #26995, #28371, #36985, .T. ) ;
#23548 = EDGE_LOOP ( 'NONE', ( #36379, #12292, #29011, #18357 ) ) ;
#23549 = FACE_BOUND ( 'NONE', #3795, .T. ) ;
#23550 = VECTOR ( 'NONE', #1355, 1000.000000000000000 ) ;
#23551 = CIRCLE ( 'NONE', #7393, 1.999999999999998224 ) ;
#23552 = EDGE_CURVE ( 'NONE', #18905, #5915, #7652, .T. ) ;
#23553 = DIRECTION ( 'NONE',  ( -1.000000000000000000, 0.000000000000000000, 0.000000000000000000 ) ) ;
#23554 = CARTESIAN_POINT ( 'NONE',  ( -77.00000337463097821, 25.98076211353318854, -5.000000000000000000 ) ) ;
#23555 = ORIENTED_EDGE ( 'NONE', *, *, #4630, .F. ) ;
#23556 = CARTESIAN_POINT ( 'NONE',  ( 5.244800587397357106, 2.026986389275619249, -4.190560292650617136 ) ) ;
#23557 = CARTESIAN_POINT ( 'NONE',  ( 0.000000000000000000, 55.00000000000000000, -16.00000000000000000 ) ) ;
#23558 = CARTESIAN_POINT ( 'NONE',  ( 2.778182860042562208, -69.13212189986967360, 12.49999999999999645 ) ) ;
#23559 = AXIS2_PLACEMENT_3D ( 'NONE', #5684, #22769, #2686 ) ;
#23560 = DIRECTION ( 'NONE',  ( 0.000000000000000000, 0.000000000000000000, 1.000000000000000000 ) ) ;
#23561 = DIRECTION ( 'NONE',  ( 0.000000000000000000, 0.000000000000000000, 1.000000000000000000 ) ) ;
#23562 = VERTEX_POINT ( 'NONE', #36456 ) ;
#23563 = CARTESIAN_POINT ( 'NONE',  ( 61.25926521283101067, -32.16008401677932227, -49.22241343995298024 ) ) ;
#23564 = DIRECTION ( 'NONE',  ( 0.000000000000000000, 0.000000000000000000, 1.000000000000000000 ) ) ;
#23565 = DIRECTION ( 'NONE',  ( 0.000000000000000000, 0.000000000000000000, 1.000000000000000000 ) ) ;
#23566 = EDGE_LOOP ( 'NONE', ( #32488, #24976, #23247, #31773 ) ) ;
#23567 = EDGE_CURVE ( 'NONE', #14423, #17871, #1031, .T. ) ;
#23568 = ORIENTED_EDGE ( 'NONE', *, *, #11293, .T. ) ;
#23569 = VERTEX_POINT ( 'NONE', #2504 ) ;
#23570 = VECTOR ( 'NONE', #36430, 1000.000000000000000 ) ;
#23571 = CARTESIAN_POINT ( 'NONE',  ( -78.00000337463094979, -2.428612866367529932E-14, -9.999999999999998224 ) ) ;
#23572 = ADVANCED_FACE ( 'NONE', ( #2329 ), #13758, .F. ) ;
#23573 = CIRCLE ( 'NONE', #3234, 3.000000000000001332 ) ;
#23574 = DIRECTION ( 'NONE',  ( -0.8660254037844449249, -0.4999999999999888423, 0.000000000000000000 ) ) ;
#23575 = ORIENTED_EDGE ( 'NONE', *, *, #1709, .F. ) ;
#23576 = EDGE_CURVE ( 'NONE', #16224, #16338, #14809, .T. ) ;
#23577 = LINE ( 'NONE', #138, #17569 ) ;
#23578 = DIRECTION ( 'NONE',  ( 0.7071067811865536790, 0.7071067811865414665, 0.000000000000000000 ) ) ;
#23579 = CARTESIAN_POINT ( 'NONE',  ( 69.99999662536839651, 17.32050807568879236, 17.49999999999999645 ) ) ;
#23580 = ORIENTED_EDGE ( 'NONE', *, *, #14347, .F. ) ;
#23581 = AXIS2_PLACEMENT_3D ( 'NONE', #7801, #10409, #34188 ) ;
#23582 = ORIENTED_EDGE ( 'NONE', *, *, #34537, .F. ) ;
#23583 = CARTESIAN_POINT ( 'NONE',  ( 0.000000000000000000, 55.00000000000000000, -5.000000000000000888 ) ) ;
#23584 = AXIS2_PLACEMENT_3D ( 'NONE', #24787, #36418, #10342 ) ;
#23585 = DIRECTION ( 'NONE',  ( 0.000000000000000000, 0.000000000000000000, 1.000000000000000000 ) ) ;
#23586 = EDGE_LOOP ( 'NONE', ( #30524, #10088, #21427, #31495 ) ) ;
#23587 = DIRECTION ( 'NONE',  ( -1.047444401652940007E-14, -1.000000000000000000, 0.000000000000000000 ) ) ;
#23588 = VERTEX_POINT ( 'NONE', #17313 ) ;
#23589 = ADVANCED_FACE ( 'NONE', ( #31536 ), #5674, .F. ) ;
#23590 = FACE_BOUND ( 'NONE', #15888, .T. ) ;
#23591 = ORIENTED_EDGE ( 'NONE', *, *, #6461, .F. ) ;
#23592 = EDGE_LOOP ( 'NONE', ( #13421, #29004, #24147, #32430 ) ) ;
#23593 = DIRECTION ( 'NONE',  ( -1.000000000000000000, 0.000000000000000000, 0.000000000000000000 ) ) ;
#23594 = ORIENTED_EDGE ( 'NONE', *, *, #3188, .T. ) ;
#23595 =( LENGTH_UNIT ( ) NAMED_UNIT ( * ) SI_UNIT ( .MILLI., .METRE. ) );
#23596 = AXIS2_PLACEMENT_3D ( 'NONE', #17724, #20176, #26532 ) ;
#23597 = DIRECTION ( 'NONE',  ( -1.000000000000000000, 0.000000000000000000, 0.000000000000000000 ) ) ;
#23598 = DIRECTION ( 'NONE',  ( 0.000000000000000000, 0.000000000000000000, 1.000000000000000000 ) ) ;
#23599 = CARTESIAN_POINT ( 'NONE',  ( -77.00000337463100664, -43.30127018922202353, -9.999999999999998224 ) ) ;
#23600 = EDGE_LOOP ( 'NONE', ( #3474, #31883 ) ) ;
#23601 = ORIENTED_EDGE ( 'NONE', *, *, #13392, .T. ) ;
#23602 = VERTEX_POINT ( 'NONE', #31723 ) ;
#23603 = CIRCLE ( 'NONE', #27780, 27.00000000000001421 ) ;
#23604 = ORIENTED_EDGE ( 'NONE', *, *, #11003, .F. ) ;
#23605 = ADVANCED_FACE ( 'NONE', ( #3612 ), #28547, .F. ) ;
#23606 = ORIENTED_EDGE ( 'NONE', *, *, #17382, .F. ) ;
#23607 = DIRECTION ( 'NONE',  ( 1.000000000000000000, 0.000000000000000000, 0.000000000000000000 ) ) ;
#23608 = CIRCLE ( 'NONE', #8036, 4.700000000000000178 ) ;
#23609 = DIRECTION ( 'NONE',  ( -0.000000000000000000, -0.000000000000000000, 1.000000000000000000 ) ) ;
#23610 = EDGE_CURVE ( 'NONE', #35409, #18894, #25761, .T. ) ;
#23611 = ORIENTED_EDGE ( 'NONE', *, *, #15294, .F. ) ;
#23612 = DIRECTION ( 'NONE',  ( 1.000000000000000000, 0.000000000000000000, -0.000000000000000000 ) ) ;
#23613 = DIRECTION ( 'NONE',  ( 0.000000000000000000, 0.000000000000000000, 1.000000000000000000 ) ) ;
#23614 = CYLINDRICAL_SURFACE ( 'NONE', #5779, 30.00000000000000000 ) ;
#23615 = ORIENTED_EDGE ( 'NONE', *, *, #27206, .F. ) ;
#23616 = CARTESIAN_POINT ( 'NONE',  ( 39.99999662536853151, -69.28203230275519786, -9.999999999999998224 ) ) ;
#23617 = EDGE_CURVE ( 'NONE', #6269, #6911, #8668, .T. ) ;
#23618 = CARTESIAN_POINT ( 'NONE',  ( -2.000003374631303732, -86.60254037844400443, -9.999999999999998224 ) ) ;
#23619 = DIRECTION ( 'NONE',  ( -1.000000000000000000, -0.000000000000000000, -0.000000000000000000 ) ) ;
#23620 = ORIENTED_EDGE ( 'NONE', *, *, #7602, .F. ) ;
#23621 = DIRECTION ( 'NONE',  ( 1.000000000000000000, 0.000000000000000000, 0.000000000000000000 ) ) ;
#23622 = AXIS2_PLACEMENT_3D ( 'NONE', #4483, #24565, #7988 ) ;
#23623 = EDGE_CURVE ( 'NONE', #21452, #23390, #37017, .T. ) ;
#23624 = CYLINDRICAL_SURFACE ( 'NONE', #25568, 2.000000000000001776 ) ;
#23625 = EDGE_CURVE ( 'NONE', #35979, #16326, #15041, .T. ) ;
#23626 = ORIENTED_EDGE ( 'NONE', *, *, #27611, .F. ) ;
#23627 = AXIS2_PLACEMENT_3D ( 'NONE', #30172, #10490, #19314 ) ;
#23628 = ORIENTED_EDGE ( 'NONE', *, *, #18981, .T. ) ;
#23629 = CARTESIAN_POINT ( 'NONE',  ( 45.00000000000000000, 5.510910596163089556E-15, 15.00000000000000000 ) ) ;
#23630 = CARTESIAN_POINT ( 'NONE',  ( 19.53925848833874213, 89.94802294027088863, -23.27834620192013304 ) ) ;
#23631 = DIRECTION ( 'NONE',  ( 0.000000000000000000, 0.000000000000000000, -1.000000000000000000 ) ) ;
#23632 = DIRECTION ( 'NONE',  ( 1.000000000000000000, 0.000000000000000000, 0.000000000000000000 ) ) ;
#23633 = EDGE_LOOP ( 'NONE', ( #383, #22939, #14787, #22579 ) ) ;
#23634 = EDGE_CURVE ( 'NONE', #4217, #30962, #30424, .T. ) ;
#23635 = AXIS2_PLACEMENT_3D ( 'NONE', #15907, #10280, #24350 ) ;
#23636 = FACE_BOUND ( 'NONE', #7459, .T. ) ;
#23637 = CIRCLE ( 'NONE', #9848, 2.000000000000001776 ) ;
#23638 = EDGE_CURVE ( 'NONE', #12313, #19362, #17233, .T. ) ;
#23639 = DIRECTION ( 'NONE',  ( 1.000000000000000000, 0.000000000000000000, 0.000000000000000000 ) ) ;
#23640 = EDGE_CURVE ( 'NONE', #10635, #9991, #19926, .T. ) ;
#23641 = CIRCLE ( 'NONE', #7479, 2.000000000000000000 ) ;
#23642 = ORIENTED_EDGE ( 'NONE', *, *, #31911, .F. ) ;
#23643 = EDGE_CURVE ( 'NONE', #12555, #25896, #33431, .T. ) ;
#23644 = CARTESIAN_POINT ( 'NONE',  ( 40.99999999999999289, 103.4105893997321743, 27.50000000000000000 ) ) ;
#23645 = VERTEX_POINT ( 'NONE', #26467 ) ;
#23646 = CARTESIAN_POINT ( 'NONE',  ( -85.00000337463092137, 25.98076211353317433, -9.999999999999998224 ) ) ;
#23647 = CARTESIAN_POINT ( 'NONE',  ( -3.500000000000000888, 55.00000000000000000, -15.00000000000000000 ) ) ;
#23648 = DIRECTION ( 'NONE',  ( 0.000000000000000000, 0.000000000000000000, -1.000000000000000000 ) ) ;
#23649 = VERTEX_POINT ( 'NONE', #3067 ) ;
#23650 = CIRCLE ( 'NONE', #29009, 27.00000000000001776 ) ;
#23651 = VERTEX_POINT ( 'NONE', #20301 ) ;
#23652 = CARTESIAN_POINT ( 'NONE',  ( -80.00000337463094979, 17.32050807568878525, -5.000000000000000000 ) ) ;
#23653 = DIRECTION ( 'NONE',  ( 1.000000000000000000, 0.000000000000000000, 0.000000000000000000 ) ) ;
#23654 = DIRECTION ( 'NONE',  ( -1.000000000000000000, 0.000000000000000000, 0.000000000000000000 ) ) ;
#23655 = VECTOR ( 'NONE', #14974, 1000.000000000000000 ) ;
#23656 = ORIENTED_EDGE ( 'NONE', *, *, #3861, .T. ) ;
#23657 = CARTESIAN_POINT ( 'NONE',  ( 16.99999662536863454, -77.94228634059960825, 17.49999999999999645 ) ) ;
#23658 = FACE_BOUND ( 'NONE', #24672, .T. ) ;
#23659 = DIRECTION ( 'NONE',  ( 0.000000000000000000, 0.000000000000000000, 1.000000000000000000 ) ) ;
#23660 = DIRECTION ( 'NONE',  ( 0.000000000000000000, 0.000000000000000000, -1.000000000000000000 ) ) ;
#23661 = FACE_OUTER_BOUND ( 'NONE', #34037, .T. ) ;
#23662 = VERTEX_POINT ( 'NONE', #23105 ) ;
#23663 = PLANE ( 'NONE',  #35678 ) ;
#23664 = FILL_AREA_STYLE_COLOUR ( '', #16183 ) ;
#23665 = DIRECTION ( 'NONE',  ( -1.000000000000000000, -0.000000000000000000, -0.000000000000000000 ) ) ;
#23666 = ORIENTED_EDGE ( 'NONE', *, *, #67, .T. ) ;
#23667 = DIRECTION ( 'NONE',  ( 0.000000000000000000, 0.000000000000000000, 1.000000000000000000 ) ) ;
#23668 = DIRECTION ( 'NONE',  ( -1.000000000000000000, 0.000000000000000000, 0.000000000000000000 ) ) ;
#23669 = DIRECTION ( 'NONE',  ( 0.000000000000000000, 0.000000000000000000, 1.000000000000000000 ) ) ;
#23670 = ORIENTED_EDGE ( 'NONE', *, *, #34466, .T. ) ;
#23671 = VERTEX_POINT ( 'NONE', #25922 ) ;
#23672 = ORIENTED_EDGE ( 'NONE', *, *, #7367, .T. ) ;
#23673 = AXIS2_PLACEMENT_3D ( 'NONE', #7389, #27075, #24468 ) ;
#23674 = CARTESIAN_POINT ( 'NONE',  ( 2.931639317407913392, -4.080919942823937774, -0.01465562841809941313 ) ) ;
#23675 = CYLINDRICAL_SURFACE ( 'NONE', #7975, 2.000000000000000000 ) ;
#23676 = AXIS2_PLACEMENT_3D ( 'NONE', #4587, #19218, #35530 ) ;
#23677 = CARTESIAN_POINT ( 'NONE',  ( -0.1709976663249050954, -5.674777143212785369, -1.879366290983713217 ) ) ;
#23678 = ORIENTED_EDGE ( 'NONE', *, *, #4124, .F. ) ;
#23679 = ORIENTED_EDGE ( 'NONE', *, *, #22316, .F. ) ;
#23680 = ORIENTED_EDGE ( 'NONE', *, *, #21355, .T. ) ;
#23681 = AXIS2_PLACEMENT_3D ( 'NONE', #4925, #1922, #21789 ) ;
#23682 = CIRCLE ( 'NONE', #20062, 1.999999999999998224 ) ;
#23683 = AXIS2_PLACEMENT_3D ( 'NONE', #13634, #28247, #22433 ) ;
#23684 = CARTESIAN_POINT ( 'NONE',  ( 27.78182860042856461, 56.67878100130339902, -49.86348611802629449 ) ) ;
#23685 = CIRCLE ( 'NONE', #2733, 2.000000000000000000 ) ;
#23686 = VERTEX_POINT ( 'NONE', #34558 ) ;
#23687 = ADVANCED_FACE ( 'NONE', ( #17117 ), #14313, .F. ) ;
#23688 = DIRECTION ( 'NONE',  ( 1.000000000000000000, 0.000000000000000000, 0.000000000000000000 ) ) ;
#23689 = ORIENTED_EDGE ( 'NONE', *, *, #18480, .F. ) ;
#23690 = DIRECTION ( 'NONE',  ( -1.000000000000000000, -0.000000000000000000, -0.000000000000000000 ) ) ;
#23691 = EDGE_LOOP ( 'NONE', ( #20389, #20368, #11958 ) ) ;
#23692 = AXIS2_PLACEMENT_3D ( 'NONE', #11517, #90, #8534 ) ;
#23693 = VERTEX_POINT ( 'NONE', #34366 ) ;
#23694 = AXIS2_PLACEMENT_3D ( 'NONE', #23966, #18318, #4083 ) ;
#23695 = CARTESIAN_POINT ( 'NONE',  ( 17.99999662536861678, -69.28203230275519786, 12.50000000000000000 ) ) ;
#23696 = FACE_BOUND ( 'NONE', #27892, .T. ) ;
#23697 = FACE_OUTER_BOUND ( 'NONE', #1546, .T. ) ;
#23698 = ORIENTED_EDGE ( 'NONE', *, *, #19334, .F. ) ;
#23699 = ORIENTED_EDGE ( 'NONE', *, *, #6122, .T. ) ;
#23700 = DIRECTION ( 'NONE',  ( 0.000000000000000000, 0.000000000000000000, 1.000000000000000000 ) ) ;
#23701 = DIRECTION ( 'NONE',  ( -0.000000000000000000, 1.000000000000000000, 0.000000000000000000 ) ) ;
#23702 = CARTESIAN_POINT ( 'NONE',  ( -28.00000337463119493, -69.28203230275522628, -5.000000000000000000 ) ) ;
#23703 = CARTESIAN_POINT ( 'NONE',  ( 89.99999662536828282, 0.000000000000000000, 17.49999999999999645 ) ) ;
#23704 = AXIS2_PLACEMENT_3D ( 'NONE', #35908, #27249, #33459 ) ;
#23705 = EDGE_LOOP ( 'NONE', ( #26371, #17000, #15348, #13280 ) ) ;
#23706 = CARTESIAN_POINT ( 'NONE',  ( -85.00000337463092137, -8.660254037844422825, -9.999999999999998224 ) ) ;
#23707 = CARTESIAN_POINT ( 'NONE',  ( 54.99999662536844625, -60.62177826491080168, -9.999999999999998224 ) ) ;
#23708 = ORIENTED_EDGE ( 'NONE', *, *, #4871, .T. ) ;
#23709 = DIRECTION ( 'NONE',  ( 0.000000000000000000, 0.000000000000000000, -1.000000000000000000 ) ) ;
#23710 = CIRCLE ( 'NONE', #30288, 0.2999999999999999334 ) ;
#23711 = FACE_OUTER_BOUND ( 'NONE', #18917, .T. ) ;
#23712 = DIRECTION ( 'NONE',  ( 1.000000000000000000, 0.000000000000000000, 0.000000000000000000 ) ) ;
#23713 = AXIS2_PLACEMENT_3D ( 'NONE', #34674, #32195, #34287 ) ;
#23714 = EDGE_CURVE ( 'NONE', #11964, #11432, #219, .T. ) ;
#23715 = AXIS2_PLACEMENT_3D ( 'NONE', #1882, #27738, #13138 ) ;
#23716 = AXIS2_PLACEMENT_3D ( 'NONE', #2353, #2148, #25049 ) ;
#23717 = EDGE_CURVE ( 'NONE', #26378, #27735, #17834, .T. ) ;
#23718 = CARTESIAN_POINT ( 'NONE',  ( -57.00000337463107059, 43.30127018922197379, -5.000000000000000000 ) ) ;
#23719 = CIRCLE ( 'NONE', #7549, 33.00000000000001421 ) ;
#23720 = AXIS2_PLACEMENT_3D ( 'NONE', #23855, #15913, #35305 ) ;
#23721 = CYLINDRICAL_SURFACE ( 'NONE', #28107, 6.000000000000005329 ) ;
#23722 = DIRECTION ( 'NONE',  ( 1.000000000000000000, 0.000000000000000000, 0.000000000000000000 ) ) ;
#23723 = VERTEX_POINT ( 'NONE', #20108 ) ;
#23724 = LINE ( 'NONE', #32143, #19007 ) ;
#23725 = CIRCLE ( 'NONE', #11133, 100.0000000000000142 ) ;
#23726 = CARTESIAN_POINT ( 'NONE',  ( -68.00000337463099243, 51.96152422706637708, 17.49999999999999645 ) ) ;
#23727 = CYLINDRICAL_SURFACE ( 'NONE', #15186, 2.000000000000001776 ) ;
#23728 = VERTEX_POINT ( 'NONE', #5876 ) ;
#23730 = VERTEX_POINT ( 'NONE', #20466 ) ;
#23729 = ADVANCED_FACE ( 'NONE', ( #8861 ), #11649, .F. ) ;
#23731 = EDGE_LOOP ( 'NONE', ( #28230, #10232, #23856 ) ) ;
#23732 = CARTESIAN_POINT ( 'NONE',  ( -3.368272016354732390, 78.44802294027070388, -24.99999999999999645 ) ) ;
#23733 = CARTESIAN_POINT ( 'NONE',  ( 64.99999662536842493, 43.30127018922200222, 12.50000000000000000 ) ) ;
#23734 = DIRECTION ( 'NONE',  ( 0.000000000000000000, 0.000000000000000000, -1.000000000000000000 ) ) ;
#23735 = CIRCLE ( 'NONE', #12931, 65.00000000000000000 ) ;
#23736 = LINE ( 'NONE', #1593, #2362 ) ;
#23737 = AXIS2_PLACEMENT_3D ( 'NONE', #14614, #362, #31843 ) ;
#23738 = DIRECTION ( 'NONE',  ( 0.000000000000000000, 0.000000000000000000, 1.000000000000000000 ) ) ;
#23739 = ORIENTED_EDGE ( 'NONE', *, *, #107, .T. ) ;
#23740 = ADVANCED_FACE ( 'NONE', ( #14657 ), #3424, .F. ) ;
#23741 = DIRECTION ( 'NONE',  ( 1.000000000000000000, 0.000000000000000000, 0.000000000000000000 ) ) ;
#23742 = ORIENTED_EDGE ( 'NONE', *, *, #3430, .F. ) ;
#23743 = AXIS2_PLACEMENT_3D ( 'NONE', #8571, #22648, #10842 ) ;
#23744 = FACE_BOUND ( 'NONE', #6779, .T. ) ;
#23745 = CIRCLE ( 'NONE', #12939, 2.000000000000001776 ) ;
#23746 = AXIS2_PLACEMENT_3D ( 'NONE', #21190, #30179, #21746 ) ;
#23747 = CIRCLE ( 'NONE', #5785, 3.000000000000002665 ) ;
#23748 = CIRCLE ( 'NONE', #17166, 33.00000000000001421 ) ;
#23749 = DIRECTION ( 'NONE',  ( 0.000000000000000000, 0.000000000000000000, 1.000000000000000000 ) ) ;
#23750 = CARTESIAN_POINT ( 'NONE',  ( 5.000000000000000000, 25.00000000000000000, -15.00000000000000000 ) ) ;
#23751 = ORIENTED_EDGE ( 'NONE', *, *, #35330, .T. ) ;
#23752 = CARTESIAN_POINT ( 'NONE',  ( 5.238704763094642836, 1.015773027556920338, -4.085839086323460378 ) ) ;
#23753 = APPLICATION_PROTOCOL_DEFINITION ( 'draft international standard', 'automotive_design', 1998, #11542 ) ;
#23754 = AXIS2_PLACEMENT_3D ( 'NONE', #17887, #23138, #3639 ) ;
#23755 = LINE ( 'NONE', #29183, #7500 ) ;
#23756 = DIRECTION ( 'NONE',  ( -0.000000000000000000, -0.000000000000000000, -1.000000000000000000 ) ) ;
#23757 = DIRECTION ( 'NONE',  ( 1.000000000000000000, 0.000000000000000000, 0.000000000000000000 ) ) ;
#23758 = EDGE_CURVE ( 'NONE', #20354, #36154, #34613, .T. ) ;
#23759 = ORIENTED_EDGE ( 'NONE', *, *, #26338, .F. ) ;
#23760 = CARTESIAN_POINT ( 'NONE',  ( -20.00000337463122690, 86.60254037844397601, 12.50000000000000000 ) ) ;
#23761 = CARTESIAN_POINT ( 'NONE',  ( 94.40806000769313755, 12.15049814296589226, 27.50000000000000000 ) ) ;
#23762 = DIRECTION ( 'NONE',  ( 1.000000000000000000, 0.000000000000000000, 0.000000000000000000 ) ) ;
#23763 = EDGE_CURVE ( 'NONE', #8255, #2201, #15437, .T. ) ;
#23764 = AXIS2_PLACEMENT_3D ( 'NONE', #34749, #26465, #6604 ) ;
#23765 = ORIENTED_EDGE ( 'NONE', *, *, #26140, .T. ) ;
#23766 = ORIENTED_EDGE ( 'NONE', *, *, #2142, .T. ) ;
#23767 = VECTOR ( 'NONE', #16128, 1000.000000000000000 ) ;
#23768 = EDGE_LOOP ( 'NONE', ( #36613, #26981, #18595, #19814 ) ) ;
#23769 = EDGE_CURVE ( 'NONE', #1092, #13427, #22024, .T. ) ;
#23770 = CARTESIAN_POINT ( 'NONE',  ( 2.143131898507887033E-16, 84.74289592134881843, -25.98445554337711627 ) ) ;
#23771 = FACE_OUTER_BOUND ( 'NONE', #5703, .T. ) ;
#23772 = AXIS2_PLACEMENT_3D ( 'NONE', #7056, #27657, #7419 ) ;
#23773 = DIRECTION ( 'NONE',  ( 1.000000000000000000, 0.000000000000000000, 0.000000000000000000 ) ) ;
#23774 = EDGE_CURVE ( 'NONE', #36432, #22247, #3970, .T. ) ;
#23775 = CARTESIAN_POINT ( 'NONE',  ( -18.00000337463123756, -86.60254037844400443, 17.49999999999999645 ) ) ;
#23776 = LINE ( 'NONE', #32956, #13503 ) ;
#23777 = FACE_OUTER_BOUND ( 'NONE', #24967, .T. ) ;
#23778 = ORIENTED_EDGE ( 'NONE', *, *, #11367, .T. ) ;
#23779 = AXIS2_PLACEMENT_3D ( 'NONE', #33438, #2656, #27787 ) ;
#23780 = VERTEX_POINT ( 'NONE', #24415 ) ;
#23781 = CARTESIAN_POINT ( 'NONE',  ( 0.000000000000000000, 55.00000000000000000, 5.000000000000000888 ) ) ;
#23782 = DIRECTION ( 'NONE',  ( -1.000000000000000000, 0.000000000000000000, 0.000000000000000000 ) ) ;
#23783 = ORIENTED_EDGE ( 'NONE', *, *, #13111, .T. ) ;
#23784 = DIRECTION ( 'NONE',  ( 0.000000000000000000, 0.000000000000000000, -1.000000000000000000 ) ) ;
#23785 = VERTEX_POINT ( 'NONE', #7343 ) ;
#23786 = AXIS2_PLACEMENT_3D ( 'NONE', #1254, #27299, #30304 ) ;
#23787 = AXIS2_PLACEMENT_3D ( 'NONE', #18886, #22258, #16437 ) ;
#23788 = CIRCLE ( 'NONE', #16003, 2.000000000000001776 ) ;
#23789 = EDGE_CURVE ( 'NONE', #25631, #24583, #35109, .T. ) ;
#23790 = CIRCLE ( 'NONE', #5833, 3.500000000000003109 ) ;
#23791 = FACE_BOUND ( 'NONE', #29518, .T. ) ;
#23792 = ORIENTED_EDGE ( 'NONE', *, *, #36236, .T. ) ;
#23793 = VERTEX_POINT ( 'NONE', #3775 ) ;
#23794 = LINE ( 'NONE', #35246, #27214 ) ;
#23795 = ORIENTED_EDGE ( 'NONE', *, *, #32688, .T. ) ;
#23796 = CIRCLE ( 'NONE', #4012, 2.000000000000001776 ) ;
#23797 = ADVANCED_FACE ( 'NONE', ( #30199 ), #15213, .F. ) ;
#23798 = CIRCLE ( 'NONE', #11238, 2.000000000000001776 ) ;
#23799 = DIRECTION ( 'NONE',  ( 0.000000000000000000, 0.000000000000000000, 1.000000000000000000 ) ) ;
#23800 = CARTESIAN_POINT ( 'NONE',  ( -67.00000337463104927, -43.30127018922202353, 17.49999999999999645 ) ) ;
#23801 = CARTESIAN_POINT ( 'NONE',  ( 4.390739357591696154E-15, -5.773502691896305272, -3.984345921091785758 ) ) ;
#23802 = EDGE_CURVE ( 'NONE', #19362, #12313, #25648, .T. ) ;
#23803 = VERTEX_POINT ( 'NONE', #18608 ) ;
#23804 = VERTEX_POINT ( 'NONE', #970 ) ;
#23805 = CIRCLE ( 'NONE', #34574, 2.000000000000000000 ) ;
#23806 = EDGE_LOOP ( 'NONE', ( #9588, #15462 ) ) ;
#23807 = VERTEX_POINT ( 'NONE', #30024 ) ;
#23808 = ORIENTED_EDGE ( 'NONE', *, *, #8363, .F. ) ;
#23809 = DIRECTION ( 'NONE',  ( 0.000000000000000000, 0.000000000000000000, 1.000000000000000000 ) ) ;
#23810 = CARTESIAN_POINT ( 'NONE',  ( -52.00000337463109190, 51.96152422706637708, -9.999999999999998224 ) ) ;
#23811 = ORIENTED_EDGE ( 'NONE', *, *, #29136, .F. ) ;
#23812 = AXIS2_PLACEMENT_3D ( 'NONE', #15322, #21318, #26767 ) ;
#23814 = AXIS2_PLACEMENT_3D ( 'NONE', #36081, #1570, #13204 ) ;
#23813 = DIRECTION ( 'NONE',  ( 1.000000000000000000, 0.000000000000000000, 0.000000000000000000 ) ) ;
#23815 = CARTESIAN_POINT ( 'NONE',  ( 98.70586713948475222, 66.35239263737575754, 32.49999999999999289 ) ) ;
#23816 = DIRECTION ( 'NONE',  ( 1.000000000000000000, 0.000000000000000000, 0.000000000000000000 ) ) ;
#23817 = ORIENTED_EDGE ( 'NONE', *, *, #20903, .F. ) ;
#23818 = DIRECTION ( 'NONE',  ( 0.000000000000000000, 0.000000000000000000, -1.000000000000000000 ) ) ;
#23819 = CIRCLE ( 'NONE', #24409, 2.000000000000001776 ) ;
#23820 = FACE_OUTER_BOUND ( 'NONE', #13951, .T. ) ;
#23821 = EDGE_CURVE ( 'NONE', #30697, #11450, #34027, .T. ) ;
#23822 = AXIS2_PLACEMENT_3D ( 'NONE', #27601, #21777, #24982 ) ;
#23823 = CARTESIAN_POINT ( 'NONE',  ( 3.368272016354729725, 78.44802294027070388, -24.99999999999999289 ) ) ;
#23824 = VERTEX_POINT ( 'NONE', #15777 ) ;
#23825 = DIRECTION ( 'NONE',  ( 1.000000000000000000, 0.000000000000000000, 0.000000000000000000 ) ) ;
#23826 = DIRECTION ( 'NONE',  ( 0.000000000000000000, 0.000000000000000000, 1.000000000000000000 ) ) ;
#23827 = ORIENTED_EDGE ( 'NONE', *, *, #18702, .T. ) ;
#23828 = ORIENTED_EDGE ( 'NONE', *, *, #469, .F. ) ;
#23829 = CIRCLE ( 'NONE', #2850, 2.000000000000001776 ) ;
#23830 = DIRECTION ( 'NONE',  ( 0.000000000000000000, 0.000000000000000000, 1.000000000000000000 ) ) ;
#23831 = DIRECTION ( 'NONE',  ( -0.000000000000000000, -0.000000000000000000, 1.000000000000000000 ) ) ;
#23832 = FACE_OUTER_BOUND ( 'NONE', #36348, .T. ) ;
#23833 = CARTESIAN_POINT ( 'NONE',  ( 64.99999662536841072, -25.98076211353320275, -9.999999999999998224 ) ) ;
#23834 = ORIENTED_EDGE ( 'NONE', *, *, #21976, .F. ) ;
#23835 = AXIS2_PLACEMENT_3D ( 'NONE', #3824, #7022, #26900 ) ;
#23836 = CARTESIAN_POINT ( 'NONE',  ( -5.000000000000000000, 2.424500739214314304, -0.4207179063848073275 ) ) ;
#23837 = PLANE ( 'NONE',  #24330 ) ;
#23838 = EDGE_CURVE ( 'NONE', #24005, #200, #6474, .T. ) ;
#23839 = VECTOR ( 'NONE', #30987, 1000.000000000000000 ) ;
#23840 = EDGE_LOOP ( 'NONE', ( #31776, #35853, #14789, #7254, #12633 ) ) ;
#23841 = ADVANCED_FACE ( 'NONE', ( #10171 ), #32282, .T. ) ;
#23842 = VECTOR ( 'NONE', #36284, 1000.000000000000000 ) ;
#23843 = CARTESIAN_POINT ( 'NONE',  ( -53.72397537678465085, -62.16182779291699489, 12.50000000000000000 ) ) ;
#23844 = ORIENTED_EDGE ( 'NONE', *, *, #19124, .T. ) ;
#23845 = CIRCLE ( 'NONE', #7681, 2.000000000000000000 ) ;
#23846 = DIRECTION ( 'NONE',  ( 0.000000000000000000, 0.000000000000000000, 1.000000000000000000 ) ) ;
#23847 = ADVANCED_FACE ( 'NONE', ( #1516 ), #33028, .F. ) ;
#23848 = DIRECTION ( 'NONE',  ( -1.000000000000000000, 0.000000000000000000, 0.000000000000000000 ) ) ;
#23849 = AXIS2_PLACEMENT_3D ( 'NONE', #18790, #30766, #33211 ) ;
#23850 = CYLINDRICAL_SURFACE ( 'NONE', #20826, 1.999999999999998224 ) ;
#23851 = ORIENTED_EDGE ( 'NONE', *, *, #25666, .T. ) ;
#23852 = ORIENTED_EDGE ( 'NONE', *, *, #19716, .F. ) ;
#23853 = ADVANCED_FACE ( 'NONE', ( #9773 ), #4172, .F. ) ;
#23854 = EDGE_CURVE ( 'NONE', #22239, #13283, #8269, .T. ) ;
#23855 = CARTESIAN_POINT ( 'NONE',  ( 64.99999662536841072, -25.98076211353320275, -5.000000000000000000 ) ) ;
#23856 = ORIENTED_EDGE ( 'NONE', *, *, #36645, .F. ) ;
#23857 = CARTESIAN_POINT ( 'NONE',  ( 83.47442710120355969, -31.09745072740822991, 12.49999999999999645 ) ) ;
#23858 = FACE_BOUND ( 'NONE', #33822, .T. ) ;
#23859 = DIRECTION ( 'NONE',  ( 1.000000000000000000, 0.000000000000000000, 0.000000000000000000 ) ) ;
#23860 = DIRECTION ( 'NONE',  ( -1.000000000000000000, 0.000000000000000000, 0.000000000000000000 ) ) ;
#23861 = CIRCLE ( 'NONE', #7698, 2.000000000000001776 ) ;
#23862 = CARTESIAN_POINT ( 'NONE',  ( 83.67878100130370456, -27.78182860042797131, -49.86348611802629449 ) ) ;
#23863 = EDGE_CURVE ( 'NONE', #35244, #16038, #24437, .T. ) ;
#23864 = ORIENTED_EDGE ( 'NONE', *, *, #11293, .F. ) ;
#23865 = DIRECTION ( 'NONE',  ( 1.000000000000000000, 0.000000000000000000, 0.000000000000000000 ) ) ;
#23866 = EDGE_CURVE ( 'NONE', #21698, #26530, #21429, .T. ) ;
#23867 = CARTESIAN_POINT ( 'NONE',  ( 69.99999662536838230, -51.96152422706639840, -5.000000000000000000 ) ) ;
#23868 = ADVANCED_FACE ( 'NONE', ( #29842 ), #4731, .T. ) ;
#23869 = CIRCLE ( 'NONE', #14894, 2.000000000000001776 ) ;
#23870 = CARTESIAN_POINT ( 'NONE',  ( -31.46585318596190106, -86.45172111230344569, -49.86348611802629449 ) ) ;
#23871 = EDGE_LOOP ( 'NONE', ( #35096, #33128, #28329, #12535 ) ) ;
#23872 = EDGE_CURVE ( 'NONE', #29309, #17608, #10652, .T. ) ;
#23873 = DIRECTION ( 'NONE',  ( 0.000000000000000000, 0.000000000000000000, 1.000000000000000000 ) ) ;
#23874 = AXIS2_PLACEMENT_3D ( 'NONE', #3373, #31841, #14060 ) ;
#23875 = FACE_OUTER_BOUND ( 'NONE', #10989, .T. ) ;
#23876 = CARTESIAN_POINT ( 'NONE',  ( 49.99999662536846756, 69.28203230275516944, 17.49999999999999645 ) ) ;
#23877 = AXIS2_PLACEMENT_3D ( 'NONE', #2546, #34246, #31230 ) ;
#23878 = EDGE_LOOP ( 'NONE', ( #14641, #36566 ) ) ;
#23879 = ORIENTED_EDGE ( 'NONE', *, *, #11143, .F. ) ;
#23880 = DIRECTION ( 'NONE',  ( -1.000000000000000000, 0.000000000000000000, 0.000000000000000000 ) ) ;
#23881 = CARTESIAN_POINT ( 'NONE',  ( 2.999996625368645198, 77.94228634059957983, -9.999999999999998224 ) ) ;
#23882 = CARTESIAN_POINT ( 'NONE',  ( 34.00000000000000000, -103.4105893997321743, 32.50000000000000000 ) ) ;
#23883 = ORIENTED_EDGE ( 'NONE', *, *, #14543, .F. ) ;
#23884 = ORIENTED_EDGE ( 'NONE', *, *, #20595, .F. ) ;
#23885 = VERTEX_POINT ( 'NONE', #10717 ) ;
#23886 = CIRCLE ( 'NONE', #507, 2.000000000000001776 ) ;
#23887 = AXIS2_PLACEMENT_3D ( 'NONE', #13362, #32890, #22196 ) ;
#23888 = DIRECTION ( 'NONE',  ( 1.000000000000000000, 0.000000000000000000, 0.000000000000000000 ) ) ;
#23889 = EDGE_CURVE ( 'NONE', #1670, #725, #16889, .T. ) ;
#23890 = ORIENTED_EDGE ( 'NONE', *, *, #34845, .F. ) ;
#23891 = FACE_OUTER_BOUND ( 'NONE', #10754, .T. ) ;
#23892 = ORIENTED_EDGE ( 'NONE', *, *, #1413, .F. ) ;
#23893 = DIRECTION ( 'NONE',  ( 0.000000000000000000, 0.000000000000000000, 1.000000000000000000 ) ) ;
#23894 = ORIENTED_EDGE ( 'NONE', *, *, #25361, .T. ) ;
#23895 = VERTEX_POINT ( 'NONE', #33771 ) ;
#23896 = SURFACE_STYLE_USAGE ( .BOTH. , #10705 ) ;
#23897 = CARTESIAN_POINT ( 'NONE',  ( 4.282125186551308360, -3.301216562737187221, -1.327869168827487290 ) ) ;
#23898 = VECTOR ( 'NONE', #8218, 1000.000000000000000 ) ;
#23899 = DIRECTION ( 'NONE',  ( 0.000000000000000000, 0.000000000000000000, -1.000000000000000000 ) ) ;
#23900 = ORIENTED_EDGE ( 'NONE', *, *, #22971, .T. ) ;
#23901 = ORIENTED_EDGE ( 'NONE', *, *, #16072, .F. ) ;
#23902 = EDGE_CURVE ( 'NONE', #30974, #5388, #19710, .T. ) ;
#23903 = LINE ( 'NONE', #35518, #12502 ) ;
#23904 = AXIS2_PLACEMENT_3D ( 'NONE', #31961, #8569, #11387 ) ;
#23905 = CARTESIAN_POINT ( 'NONE',  ( 71.99999662536838230, -34.64101615137759183, -5.000000000000000000 ) ) ;
#23906 = DIRECTION ( 'NONE',  ( -0.000000000000000000, -0.000000000000000000, -1.000000000000000000 ) ) ;
#23907 = CARTESIAN_POINT ( 'NONE',  ( 0.000000000000000000, 0.000000000000000000, 1.716666666667001406 ) ) ;
#23908 = ORIENTED_EDGE ( 'NONE', *, *, #11553, .T. ) ;
#23909 = CARTESIAN_POINT ( 'NONE',  ( 51.13139720814419320, 27.49999999999988987, 5.000000000000000888 ) ) ;
#23910 = CARTESIAN_POINT ( 'NONE',  ( 27.99999662536855993, 69.28203230275518365, -9.999999999999998224 ) ) ;
#23911 = CIRCLE ( 'NONE', #34087, 2.000000000000001776 ) ;
#23912 = EDGE_LOOP ( 'NONE', ( #31962, #8173 ) ) ;
#23913 = DIRECTION ( 'NONE',  ( 1.000000000000000000, 0.000000000000000000, 0.000000000000000000 ) ) ;
#23914 = CARTESIAN_POINT ( 'NONE',  ( -68.00000000000000000, 0.000000000000000000, -4.999999999999997335 ) ) ;
#23915 = CYLINDRICAL_SURFACE ( 'NONE', #10604, 2.000000000000001776 ) ;
#23916 = AXIS2_PLACEMENT_3D ( 'NONE', #13304, #27176, #30571 ) ;
#23917 = DIRECTION ( 'NONE',  ( 0.000000000000000000, 0.000000000000000000, 1.000000000000000000 ) ) ;
#23918 = EDGE_CURVE ( 'NONE', #35505, #14063, #25035, .T. ) ;
#23919 = CIRCLE ( 'NONE', #7746, 33.00000000000001421 ) ;
#23920 = DIRECTION ( 'NONE',  ( 0.000000000000000000, 0.000000000000000000, 1.000000000000000000 ) ) ;
#23921 = EDGE_CURVE ( 'NONE', #6911, #3619, #26218, .T. ) ;
#23922 = EDGE_CURVE ( 'NONE', #3470, #35481, #7063, .T. ) ;
#23923 = CARTESIAN_POINT ( 'NONE',  ( 5.000000000000000000, 2.691270400161075216, -1.881368198414912429 ) ) ;
#23924 = VERTEX_POINT ( 'NONE', #18972 ) ;
#23925 = CARTESIAN_POINT ( 'NONE',  ( 27.78182860042856461, 56.67878100130339902, -4.999999999999997335 ) ) ;
#23926 = DIRECTION ( 'NONE',  ( 1.000000000000000000, 0.000000000000000000, 0.000000000000000000 ) ) ;
#23927 = DIRECTION ( 'NONE',  ( 0.000000000000000000, 0.000000000000000000, 1.000000000000000000 ) ) ;
#23928 = EDGE_LOOP ( 'NONE', ( #14106, #1252, #35931, #14874, #11678, #37072 ) ) ;
#23929 = ORIENTED_EDGE ( 'NONE', *, *, #35360, .F. ) ;
#23930 = VECTOR ( 'NONE', #27937, 1000.000000000000000 ) ;
#23931 = VERTEX_POINT ( 'NONE', #13326 ) ;
#23932 = AXIS2_PLACEMENT_3D ( 'NONE', #31630, #6130, #17748 ) ;
#23933 = DIRECTION ( 'NONE',  ( 0.000000000000000000, 0.000000000000000000, -1.000000000000000000 ) ) ;
#23934 = DIRECTION ( 'NONE',  ( 0.000000000000000000, 0.000000000000000000, 1.000000000000000000 ) ) ;
#23935 = AXIS2_PLACEMENT_3D ( 'NONE', #2496, #25201, #36446 ) ;
#23936 = CARTESIAN_POINT ( 'NONE',  ( -2.308176576174226117E-14, -5.999999999999947597, 27.50000000000000000 ) ) ;
#23937 = DIRECTION ( 'NONE',  ( 0.000000000000000000, 0.000000000000000000, 1.000000000000000000 ) ) ;
#23938 = DIRECTION ( 'NONE',  ( 0.000000000000000000, 0.000000000000000000, 1.000000000000000000 ) ) ;
#23939 = ORIENTED_EDGE ( 'NONE', *, *, #36946, .T. ) ;
#23940 = DIRECTION ( 'NONE',  ( 1.000000000000000000, 0.000000000000000000, 0.000000000000000000 ) ) ;
#23941 = ORIENTED_EDGE ( 'NONE', *, *, #34548, .F. ) ;
#23942 = FACE_BOUND ( 'NONE', #1994, .T. ) ;
#23943 = CIRCLE ( 'NONE', #4780, 2.000000000000001776 ) ;
#23944 = EDGE_CURVE ( 'NONE', #23091, #37038, #11827, .T. ) ;
#23945 = DIRECTION ( 'NONE',  ( -0.5000000000000098810, -0.8660254037844328234, 0.000000000000000000 ) ) ;
#23946 = CARTESIAN_POINT ( 'NONE',  ( 40.99999999999999289, -103.4105893997321743, 32.50000000000000000 ) ) ;
#23947 = ORIENTED_EDGE ( 'NONE', *, *, #34294, .F. ) ;
#23948 = LINE ( 'NONE', #34821, #29627 ) ;
#23949 = AXIS2_PLACEMENT_3D ( 'NONE', #1337, #4170, #6605 ) ;
#23950 = FACE_OUTER_BOUND ( 'NONE', #26410, .T. ) ;
#23951 = AXIS2_PLACEMENT_3D ( 'NONE', #8369, #34412, #11891 ) ;
#23952 = DIRECTION ( 'NONE',  ( -0.000000000000000000, -0.000000000000000000, 1.000000000000000000 ) ) ;
#23953 = CARTESIAN_POINT ( 'NONE',  ( 0.000000000000000000, 0.000000000000000000, -5.000000000000000000 ) ) ;
#23954 = ORIENTED_EDGE ( 'NONE', *, *, #11363, .T. ) ;
#23955 = DIRECTION ( 'NONE',  ( 1.000000000000000000, 0.000000000000000000, 0.000000000000000000 ) ) ;
#23956 = AXIS2_PLACEMENT_3D ( 'NONE', #12490, #15505, #14750 ) ;
#23957 = CARTESIAN_POINT ( 'NONE',  ( -17.14523346298279449, 93.36492675454785228, -49.86561046011506448 ) ) ;
#23958 = CARTESIAN_POINT ( 'NONE',  ( -18.00000337463124467, 69.28203230275516944, 17.49999999999999645 ) ) ;
#23959 = EDGE_LOOP ( 'NONE', ( #1507, #34846, #3247, #25300 ) ) ;
#23960 = ORIENTED_EDGE ( 'NONE', *, *, #24770, .T. ) ;
#23961 = ADVANCED_FACE ( 'NONE', ( #11066 ), #19170, .F. ) ;
#23962 = ORIENTED_EDGE ( 'NONE', *, *, #7456, .T. ) ;
#23963 = CARTESIAN_POINT ( 'NONE',  ( -68.66839587347244844, -56.74224907229008608, -4.999999999999997335 ) ) ;
#23964 = CARTESIAN_POINT ( 'NONE',  ( -57.00000337463109901, -60.62177826491083010, 17.49999999999999645 ) ) ;
#23965 = VECTOR ( 'NONE', #22586, 1000.000000000000000 ) ;
#23966 = CARTESIAN_POINT ( 'NONE',  ( 44.99999662536851019, 77.94228634059959404, 17.49999999999999645 ) ) ;
#23967 = AXIS2_PLACEMENT_3D ( 'NONE', #32856, #10340, #12764 ) ;
#23968 = CARTESIAN_POINT ( 'NONE',  ( 34.99999662536855283, -60.62177826491080168, 12.50000000000000000 ) ) ;
#23969 = CARTESIAN_POINT ( 'NONE',  ( -35.19434990244938888, 52.39915983220783602, 12.49999999999999822 ) ) ;
#23970 = AXIS2_PLACEMENT_3D ( 'NONE', #17994, #18165, #3916 ) ;
#23971 = CARTESIAN_POINT ( 'NONE',  ( -56.67878100130369035, 27.78182860042797131, 12.49999999999999822 ) ) ;
#23972 = ORIENTED_EDGE ( 'NONE', *, *, #15391, .T. ) ;
#23973 = ORIENTED_EDGE ( 'NONE', *, *, #17801, .F. ) ;
#23974 = DIRECTION ( 'NONE',  ( 0.000000000000000000, 0.000000000000000000, -1.000000000000000000 ) ) ;
#23975 = CIRCLE ( 'NONE', #15593, 2.000000000000001776 ) ;
#23976 = DIRECTION ( 'NONE',  ( -1.156482317317870344E-14, -1.000000000000000000, 0.000000000000000000 ) ) ;
#23977 = ORIENTED_EDGE ( 'NONE', *, *, #26640, .F. ) ;
#23978 = CARTESIAN_POINT ( 'NONE',  ( -4.279621169095561228, 62.97617850287782915, -4.999999999999997335 ) ) ;
#23979 = ORIENTED_EDGE ( 'NONE', *, *, #14504, .F. ) ;
#23980 = EDGE_CURVE ( 'NONE', #22867, #13211, #12195, .T. ) ;
#23981 = DIRECTION ( 'NONE',  ( 0.000000000000000000, 0.000000000000000000, -1.000000000000000000 ) ) ;
#23982 = ORIENTED_EDGE ( 'NONE', *, *, #21655, .F. ) ;
#23983 = ORIENTED_EDGE ( 'NONE', *, *, #20884, .T. ) ;
#23984 = AXIS2_PLACEMENT_3D ( 'NONE', #35322, #6426, #26865 ) ;
#23985 = FACE_OUTER_BOUND ( 'NONE', #28780, .T. ) ;
#23986 = ORIENTED_EDGE ( 'NONE', *, *, #5568, .F. ) ;
#23987 = SURFACE_SIDE_STYLE ('',( #12529 ) ) ;
#23988 = FACE_OUTER_BOUND ( 'NONE', #1297, .T. ) ;
#23989 = EDGE_CURVE ( 'NONE', #20259, #30504, #36593, .T. ) ;
#23990 = DIRECTION ( 'NONE',  ( -0.000000000000000000, -0.000000000000000000, 1.000000000000000000 ) ) ;
#23991 = DIRECTION ( 'NONE',  ( 0.000000000000000000, 0.000000000000000000, 1.000000000000000000 ) ) ;
#23992 = AXIS2_PLACEMENT_3D ( 'NONE', #6777, #12592, #36046 ) ;
#23993 = ORIENTED_EDGE ( 'NONE', *, *, #29026, .F. ) ;
#23994 = EDGE_LOOP ( 'NONE', ( #7922, #11991, #25101, #34803 ) ) ;
#23995 = ORIENTED_EDGE ( 'NONE', *, *, #16587, .F. ) ;
#23996 = VERTEX_POINT ( 'NONE', #8279 ) ;
#23997 = VERTEX_POINT ( 'NONE', #22157 ) ;
#23998 = DIRECTION ( 'NONE',  ( 0.000000000000000000, 0.000000000000000000, 1.000000000000000000 ) ) ;
#23999 = EDGE_CURVE ( 'NONE', #25033, #12814, #22642, .T. ) ;
#24000 = CARTESIAN_POINT ( 'NONE',  ( -4.242640687119211051, 4.242640687119288323, 27.50000000000000000 ) ) ;
#24001 = ORIENTED_EDGE ( 'NONE', *, *, #28962, .F. ) ;
#24002 = DIRECTION ( 'NONE',  ( 1.000000000000000000, 0.000000000000000000, 0.000000000000000000 ) ) ;
#24003 = CARTESIAN_POINT ( 'NONE',  ( 69.99999662536841072, 51.96152422706640550, -5.000000000000000000 ) ) ;
#24004 = CARTESIAN_POINT ( 'NONE',  ( -50.00000337463109190, 69.28203230275518365, -5.000000000000000000 ) ) ;
#24005 = VERTEX_POINT ( 'NONE', #30945 ) ;
#24006 = LINE ( 'NONE', #24371, #23053 ) ;
#24007 = DIRECTION ( 'NONE',  ( -1.000000000000000000, -0.000000000000000000, -0.000000000000000000 ) ) ;
#24008 = DIRECTION ( 'NONE',  ( 1.000000000000000000, 0.000000000000000000, 0.000000000000000000 ) ) ;
#24009 = VERTEX_POINT ( 'NONE', #5285 ) ;
#24010 = FACE_OUTER_BOUND ( 'NONE', #12826, .T. ) ;
#24011 = CARTESIAN_POINT ( 'NONE',  ( -108.3061974404896262, 19.22934205795090534, 32.50000000000000000 ) ) ;
#24012 = ORIENTED_EDGE ( 'NONE', *, *, #12961, .T. ) ;
#24013 = EDGE_CURVE ( 'NONE', #36949, #30459, #15465, .T. ) ;
#24014 = ORIENTED_EDGE ( 'NONE', *, *, #22255, .T. ) ;
#24015 = DIRECTION ( 'NONE',  ( 0.000000000000000000, 0.000000000000000000, 1.000000000000000000 ) ) ;
#24016 = EDGE_CURVE ( 'NONE', #26329, #8382, #24611, .T. ) ;
#24017 = DIRECTION ( 'NONE',  ( 0.4999999999999924505, -0.8660254037844429265, 0.000000000000000000 ) ) ;
#24018 = VECTOR ( 'NONE', #35274, 1000.000000000000000 ) ;
#24019 = FACE_OUTER_BOUND ( 'NONE', #22706, .T. ) ;
#24020 = DIRECTION ( 'NONE',  ( 0.000000000000000000, 0.000000000000000000, 1.000000000000000000 ) ) ;
#24021 = ORIENTED_EDGE ( 'NONE', *, *, #33614, .T. ) ;
#24022 = EDGE_CURVE ( 'NONE', #22555, #27665, #22082, .T. ) ;
#24023 = DIRECTION ( 'NONE',  ( 1.000000000000000000, 1.850371707708594366E-15, 0.000000000000000000 ) ) ;
#24024 = DIRECTION ( 'NONE',  ( 1.000000000000000000, 0.000000000000000000, 0.000000000000000000 ) ) ;
#24025 = ORIENTED_EDGE ( 'NONE', *, *, #6303, .T. ) ;
#24026 = EDGE_CURVE ( 'NONE', #29140, #36953, #16672, .T. ) ;
#24027 = CARTESIAN_POINT ( 'NONE',  ( 17.14523346298344109, -93.36492675454773860, 12.49999999999999822 ) ) ;
#24028 = ORIENTED_EDGE ( 'NONE', *, *, #3610, .T. ) ;
#24029 = DIRECTION ( 'NONE',  ( -0.000000000000000000, -0.000000000000000000, 1.000000000000000000 ) ) ;
#24030 = CARTESIAN_POINT ( 'NONE',  ( -85.00000337463092137, -8.660254037844422825, -9.999999999999998224 ) ) ;
#24031 = EDGE_CURVE ( 'NONE', #29299, #29323, #35842, .T. ) ;
#24032 = DIRECTION ( 'NONE',  ( 0.000000000000000000, 0.000000000000000000, 1.000000000000000000 ) ) ;
#24033 = ORIENTED_EDGE ( 'NONE', *, *, #12178, .T. ) ;
#24034 = ORIENTED_EDGE ( 'NONE', *, *, #34380, .F. ) ;
#24035 = AXIS2_PLACEMENT_3D ( 'NONE', #2995, #11235, #29358 ) ;
#24036 = ORIENTED_EDGE ( 'NONE', *, *, #5221, .T. ) ;
#24037 = CARTESIAN_POINT ( 'NONE',  ( 40.98360655737705116, 111.1639425680974398, 27.49999999999999645 ) ) ;
#24038 = DIRECTION ( 'NONE',  ( -1.000000000000000000, 0.000000000000000000, 0.000000000000000000 ) ) ;
#24039 = DIRECTION ( 'NONE',  ( 0.000000000000000000, 0.000000000000000000, 1.000000000000000000 ) ) ;
#24040 = DIRECTION ( 'NONE',  ( -0.000000000000000000, -0.000000000000000000, 1.000000000000000000 ) ) ;
#24041 = DIRECTION ( 'NONE',  ( 0.000000000000000000, 0.000000000000000000, 1.000000000000000000 ) ) ;
#24042 = ORIENTED_EDGE ( 'NONE', *, *, #16979, .F. ) ;
#24043 = CARTESIAN_POINT ( 'NONE',  ( 71.99999662536839651, -17.32050807568879947, -9.999999999999998224 ) ) ;
#24044 = EDGE_CURVE ( 'NONE', #34902, #12512, #20256, .T. ) ;
#24045 = DIRECTION ( 'NONE',  ( 0.000000000000000000, 0.000000000000000000, 1.000000000000000000 ) ) ;
#24046 = CARTESIAN_POINT ( 'NONE',  ( -45.00000337463111322, -77.94228634059960825, -9.999999999999998224 ) ) ;
#24047 = VERTEX_POINT ( 'NONE', #34876 ) ;
#24048 = APPLICATION_CONTEXT ( 'automotive_design' ) ;
#24049 = CARTESIAN_POINT ( 'NONE',  ( -70.00000337463099243, 17.32050807568877460, -9.999999999999998224 ) ) ;
#24050 = DIRECTION ( 'NONE',  ( -1.000000000000000000, 0.000000000000000000, 0.000000000000000000 ) ) ;
#24051 = LINE ( 'NONE', #21219, #3031 ) ;
#24052 = EDGE_LOOP ( 'NONE', ( #4188, #12197, #7793, #811 ) ) ;
#24053 = EDGE_CURVE ( 'NONE', #25880, #15915, #32226, .T. ) ;
#24054 = ORIENTED_EDGE ( 'NONE', *, *, #673, .F. ) ;
#24055 = AXIS2_PLACEMENT_3D ( 'NONE', #13000, #819, #4014 ) ;
#24056 = EDGE_CURVE ( 'NONE', #35643, #7161, #20248, .T. ) ;
#24057 = CARTESIAN_POINT ( 'NONE',  ( 64.99999662536841072, 25.98076211353318854, -9.999999999999998224 ) ) ;
#24058 = FACE_OUTER_BOUND ( 'NONE', #19902, .T. ) ;
#24059 = CARTESIAN_POINT ( 'NONE',  ( -1.546821644788046735, -4.880444798889548963, -0.7375898304884659362 ) ) ;
#24060 = ORIENTED_EDGE ( 'NONE', *, *, #31354, .T. ) ;
#24061 = CIRCLE ( 'NONE', #18682, 3.500000000000003109 ) ;
#24062 = ORIENTED_EDGE ( 'NONE', *, *, #12802, .F. ) ;
#24063 = VERTEX_POINT ( 'NONE', #11603 ) ;
#24064 = DIRECTION ( 'NONE',  ( -1.000000000000000000, 1.798972493605577187E-15, 0.000000000000000000 ) ) ;
#24065 = VERTEX_POINT ( 'NONE', #2831 ) ;
#24066 = ORIENTED_EDGE ( 'NONE', *, *, #21492, .F. ) ;
#24067 = CARTESIAN_POINT ( 'NONE',  ( 56.99999662536844625, 43.30127018922198801, -9.999999999999998224 ) ) ;
#24068 = ORIENTED_EDGE ( 'NONE', *, *, #8535, .F. ) ;
#24069 = ORIENTED_EDGE ( 'NONE', *, *, #31744, .F. ) ;
#24070 = CARTESIAN_POINT ( 'NONE',  ( -52.00000337463109190, 69.28203230275518365, -9.999999999999998224 ) ) ;
#24071 = EDGE_CURVE ( 'NONE', #32385, #15477, #4089, .T. ) ;
#24072 = CARTESIAN_POINT ( 'NONE',  ( 51.99999662536847467, 51.96152422706637708, -9.999999999999998224 ) ) ;
#24073 = EDGE_LOOP ( 'NONE', ( #2952, #32748, #9887, #14039, #8701 ) ) ;
#24074 = ORIENTED_EDGE ( 'NONE', *, *, #15972, .F. ) ;
#24075 = LINE ( 'NONE', #32683, #34080 ) ;
#24076 = DIRECTION ( 'NONE',  ( -0.000000000000000000, -0.000000000000000000, -1.000000000000000000 ) ) ;
#24077 = DIRECTION ( 'NONE',  ( 0.000000000000000000, 0.000000000000000000, 1.000000000000000000 ) ) ;
#24078 = LINE ( 'NONE', #32499, #28052 ) ;
#24079 = ORIENTED_EDGE ( 'NONE', *, *, #24532, .T. ) ;
#24080 = DIRECTION ( 'NONE',  ( 1.000000000000000000, 0.000000000000000000, 0.000000000000000000 ) ) ;
#24081 = AXIS2_PLACEMENT_3D ( 'NONE', #37006, #26104, #31537 ) ;
#24082 = ORIENTED_EDGE ( 'NONE', *, *, #19470, .T. ) ;
#24083 = DIRECTION ( 'NONE',  ( -0.000000000000000000, -0.000000000000000000, 1.000000000000000000 ) ) ;
#24084 = CARTESIAN_POINT ( 'NONE',  ( -82.00000337463094979, 34.64101615137757051, 12.50000000000000000 ) ) ;
#24085 = DIRECTION ( 'NONE',  ( 1.000000000000000000, 0.000000000000000000, 0.000000000000000000 ) ) ;
#24086 = CARTESIAN_POINT ( 'NONE',  ( -0.8333333333333384774, 5.292377467571578009, -3.818275046351164104 ) ) ;
#24087 = EDGE_CURVE ( 'NONE', #35523, #29052, #33456, .T. ) ;
#24088 = CARTESIAN_POINT ( 'NONE',  ( -3.374631327851540519E-06, 86.60254037844397601, 12.50000000000000000 ) ) ;
#24089 = DIRECTION ( 'NONE',  ( 0.000000000000000000, 0.000000000000000000, 1.000000000000000000 ) ) ;
#24090 = EDGE_LOOP ( 'NONE', ( #20332, #10153, #30478 ) ) ;
#24091 = EDGE_CURVE ( 'NONE', #23264, #1584, #17864, .T. ) ;
#24092 = DIRECTION ( 'NONE',  ( -0.000000000000000000, -0.000000000000000000, 1.000000000000000000 ) ) ;
#24093 = CARTESIAN_POINT ( 'NONE',  ( -50.00000337463112032, -51.96152422706641971, 12.50000000000000000 ) ) ;
#24094 = CARTESIAN_POINT ( 'NONE',  ( 66.50937412064257614, -41.98910420248104458, 12.50000000000000000 ) ) ;
#24095 = ORIENTED_EDGE ( 'NONE', *, *, #20614, .F. ) ;
#24096 = ADVANCED_FACE ( 'NONE', ( #9167 ), #11794, .F. ) ;
#24097 = AXIS2_PLACEMENT_3D ( 'NONE', #30038, #4192, #15431 ) ;
#24098 = EDGE_LOOP ( 'NONE', ( #23611, #5450, #35612, #24839 ) ) ;
#24099 = ORIENTED_EDGE ( 'NONE', *, *, #16710, .F. ) ;
#24100 = CARTESIAN_POINT ( 'NONE',  ( -10.00000337463128730, 69.28203230275516944, 12.50000000000000000 ) ) ;
#24101 = CARTESIAN_POINT ( 'NONE',  ( 43.19957991610432657, 47.04203867989531318, 12.49999999999999822 ) ) ;
#24102 = DIRECTION ( 'NONE',  ( 0.000000000000000000, 0.000000000000000000, -1.000000000000000000 ) ) ;
#24103 = ADVANCED_FACE ( 'NONE', ( #17605 ), #3182, .F. ) ;
#24104 = CARTESIAN_POINT ( 'NONE',  ( -60.00000337463107059, -34.64101615137762025, 17.49999999999999645 ) ) ;
#24105 = EDGE_CURVE ( 'NONE', #36485, #32044, #19666, .T. ) ;
#24106 = CARTESIAN_POINT ( 'NONE',  ( -5.000000000000000000, 1.947085426416883980, -5.800379292880308846 ) ) ;
#24107 = AXIS2_PLACEMENT_3D ( 'NONE', #13885, #33772, #5463 ) ;
#24108 = DIRECTION ( 'NONE',  ( 0.000000000000000000, 0.000000000000000000, 1.000000000000000000 ) ) ;
#24109 = EDGE_LOOP ( 'NONE', ( #17395, #16833 ) ) ;
#24110 = DIRECTION ( 'NONE',  ( 0.000000000000000000, 0.000000000000000000, 1.000000000000000000 ) ) ;
#24111 = EDGE_LOOP ( 'NONE', ( #18139, #1036 ) ) ;
#24112 = CARTESIAN_POINT ( 'NONE',  ( -75.00000337463097821, 8.660254037844374864, -9.999999999999998224 ) ) ;
#24113 = EDGE_CURVE ( 'NONE', #7182, #9631, #14288, .T. ) ;
#24114 = EDGE_CURVE ( 'NONE', #3735, #1626, #5889, .T. ) ;
#24115 = DIRECTION ( 'NONE',  ( 0.000000000000000000, 0.000000000000000000, 1.000000000000000000 ) ) ;
#24116 = DIRECTION ( 'NONE',  ( 0.000000000000000000, 0.000000000000000000, -1.000000000000000000 ) ) ;
#24117 = EDGE_CURVE ( 'NONE', #3385, #30697, #17290, .T. ) ;
#24118 = ADVANCED_FACE ( 'NONE', ( #22885 ), #31682, .T. ) ;
#24119 = FILL_AREA_STYLE_COLOUR ( '', #6795 ) ;
#24120 = ORIENTED_EDGE ( 'NONE', *, *, #27181, .T. ) ;
#24121 = CARTESIAN_POINT ( 'NONE',  ( 4.999996625368645198, 77.94228634059957983, 12.50000000000000000 ) ) ;
#24122 = DIRECTION ( 'NONE',  ( 0.000000000000000000, 0.000000000000000000, -1.000000000000000000 ) ) ;
#24123 = AXIS2_PLACEMENT_3D ( 'NONE', #12926, #35463, #32617 ) ;
#24124 = CARTESIAN_POINT ( 'NONE',  ( 74.99999662536836809, 43.30127018922198801, -9.999999999999998224 ) ) ;
#24125 = CARTESIAN_POINT ( 'NONE',  ( -58.88972745734203329, -33.99999999999965894, 12.49999999999999822 ) ) ;
#24126 = ORIENTED_EDGE ( 'NONE', *, *, #4095, .T. ) ;
#24127 = DIRECTION ( 'NONE',  ( 0.000000000000000000, 0.000000000000000000, 1.000000000000000000 ) ) ;
#24128 = CARTESIAN_POINT ( 'NONE',  ( 29.99999662536857770, -69.28203230275519786, 12.50000000000000000 ) ) ;
#24129 = CARTESIAN_POINT ( 'NONE',  ( 51.99999662536847467, -69.28203230275519786, -9.999999999999998224 ) ) ;
#24130 = ORIENTED_EDGE ( 'NONE', *, *, #8137, .T. ) ;
#24131 = ORIENTED_EDGE ( 'NONE', *, *, #17408, .F. ) ;
#24132 = AXIS2_PLACEMENT_3D ( 'NONE', #1579, #7223, #27255 ) ;
#24133 = ORIENTED_EDGE ( 'NONE', *, *, #2321, .F. ) ;
#24134 = CIRCLE ( 'NONE', #753, 2.000000000000001776 ) ;
#24135 = DIRECTION ( 'NONE',  ( 0.000000000000000000, -0.000000000000000000, -1.000000000000000000 ) ) ;
#24136 = CARTESIAN_POINT ( 'NONE',  ( 60.93295298011005201, 19.13981058454729123, 12.49999999999999822 ) ) ;
#24137 = DIRECTION ( 'NONE',  ( -1.000000000000000000, 0.000000000000000000, 0.000000000000000000 ) ) ;
#24138 = DIRECTION ( 'NONE',  ( 1.000000000000000000, 0.000000000000000000, 0.000000000000000000 ) ) ;
#24139 = CARTESIAN_POINT ( 'NONE',  ( -62.00000337463107769, -34.64101615137762025, -9.999999999999998224 ) ) ;
#24140 = CARTESIAN_POINT ( 'NONE',  ( -97.64030476177397588, 67.22390783198484598, 32.50000000000000000 ) ) ;
#24141 = VERTEX_POINT ( 'NONE', #28497 ) ;
#24142 = EDGE_LOOP ( 'NONE', ( #17880, #32500, #11509, #20864 ) ) ;
#24143 = PLANE ( 'NONE',  #13506 ) ;
#24144 = DIRECTION ( 'NONE',  ( 0.000000000000000000, 0.000000000000000000, 1.000000000000000000 ) ) ;
#24145 = ORIENTED_EDGE ( 'NONE', *, *, #13180, .F. ) ;
#24146 = FACE_OUTER_BOUND ( 'NONE', #18713, .T. ) ;
#24147 = ORIENTED_EDGE ( 'NONE', *, *, #33958, .T. ) ;
#24148 = CARTESIAN_POINT ( 'NONE',  ( 3.000000000000000000, 2.935248768560057453, -3.903127820947815962E-15 ) ) ;
#24149 = FACE_BOUND ( 'NONE', #33885, .T. ) ;
#24150 = ORIENTED_EDGE ( 'NONE', *, *, #8159, .F. ) ;
#24151 = CIRCLE ( 'NONE', #4408, 30.00000000000001421 ) ;
#24152 = ORIENTED_EDGE ( 'NONE', *, *, #26869, .F. ) ;
#24153 = EDGE_CURVE ( 'NONE', #26082, #21989, #8623, .T. ) ;
#24154 = CARTESIAN_POINT ( 'NONE',  ( 0.000000000000000000, 0.000000000000000000, -5.000000000000000888 ) ) ;
#24155 = EDGE_LOOP ( 'NONE', ( #25232, #20048 ) ) ;
#24156 =( NAMED_UNIT ( * ) PLANE_ANGLE_UNIT ( ) SI_UNIT ( $, .RADIAN. ) );
#24157 = PRODUCT_DEFINITION_SHAPE ( 'NONE', 'NONE',  #37118 ) ;
#24158 = DIRECTION ( 'NONE',  ( 0.000000000000000000, 0.000000000000000000, -1.000000000000000000 ) ) ;
#24159 = CARTESIAN_POINT ( 'NONE',  ( 13.89091430021463935, 62.33939050065170306, 12.49999999999999822 ) ) ;
#24160 = DIRECTION ( 'NONE',  ( 0.000000000000000000, 0.000000000000000000, -1.000000000000000000 ) ) ;
#24161 = ORIENTED_EDGE ( 'NONE', *, *, #24997, .T. ) ;
#24162 = VECTOR ( 'NONE', #34722, 1000.000000000000000 ) ;
#24163 = ORIENTED_EDGE ( 'NONE', *, *, #2414, .T. ) ;
#24164 = ORIENTED_EDGE ( 'NONE', *, *, #25901, .T. ) ;
#24165 = CIRCLE ( 'NONE', #27746, 1.999999999999998224 ) ;
#24166 = ORIENTED_EDGE ( 'NONE', *, *, #24988, .F. ) ;
#24167 = DIRECTION ( 'NONE',  ( 1.000000000000000000, 0.000000000000000000, 0.000000000000000000 ) ) ;
#24168 = DIRECTION ( 'NONE',  ( 1.000000000000000000, 0.000000000000000000, 0.000000000000000000 ) ) ;
#24169 = VERTEX_POINT ( 'NONE', #20057 ) ;
#24170 = CARTESIAN_POINT ( 'NONE',  ( -5.000000000000000000, -4.846777557549235459E-18, -0.5080592402122449114 ) ) ;
#24171 = FACE_OUTER_BOUND ( 'NONE', #30093, .T. ) ;
#24172 = EDGE_CURVE ( 'NONE', #26391, #12033, #8874, .T. ) ;
#24173 = ORIENTED_EDGE ( 'NONE', *, *, #33724, .F. ) ;
#24174 = DIRECTION ( 'NONE',  ( 1.000000000000000000, 0.000000000000000000, 0.000000000000000000 ) ) ;
#24175 = EDGE_CURVE ( 'NONE', #20479, #13005, #20429, .T. ) ;
#24176 = AXIS2_PLACEMENT_3D ( 'NONE', #3856, #32371, #35941 ) ;
#24177 = DIRECTION ( 'NONE',  ( 0.000000000000000000, 0.000000000000000000, 1.000000000000000000 ) ) ;
#24178 = AXIS2_PLACEMENT_3D ( 'NONE', #17073, #16727, #25338 ) ;
#24179 = DIRECTION ( 'NONE',  ( 0.000000000000000000, 0.000000000000000000, -1.000000000000000000 ) ) ;
#24180 = CARTESIAN_POINT ( 'NONE',  ( 101.8360233522598719, -31.92205067127980200, 32.50000000000001421 ) ) ;
#24181 = CARTESIAN_POINT ( 'NONE',  ( 42.99999662536850309, 77.94228634059959404, -9.999999999999998224 ) ) ;
#24182 = CIRCLE ( 'NONE', #30143, 2.000000000000001776 ) ;
#24183 = ORIENTED_EDGE ( 'NONE', *, *, #5637, .T. ) ;
#24184 = ORIENTED_EDGE ( 'NONE', *, *, #1295, .F. ) ;
#24185 = EDGE_CURVE ( 'NONE', #15311, #4442, #28646, .T. ) ;
#24186 = CARTESIAN_POINT ( 'NONE',  ( 111.8061974404897825, -19.22934205795014151, 27.50000000000000000 ) ) ;
#24187 = DIRECTION ( 'NONE',  ( 1.000000000000000000, 0.000000000000000000, 0.000000000000000000 ) ) ;
#24188 = DIRECTION ( 'NONE',  ( -1.000000000000000000, 0.000000000000000000, 0.000000000000000000 ) ) ;
#24189 = DIRECTION ( 'NONE',  ( 0.000000000000000000, 0.000000000000000000, 1.000000000000000000 ) ) ;
#24190 = ORIENTED_EDGE ( 'NONE', *, *, #2974, .F. ) ;
#24191 = CARTESIAN_POINT ( 'NONE',  ( -20.00000337463124112, 69.28203230275516944, 12.50000000000000000 ) ) ;
#24192 = DIRECTION ( 'NONE',  ( -0.000000000000000000, -0.000000000000000000, 1.000000000000000000 ) ) ;
#24193 = AXIS2_PLACEMENT_3D ( 'NONE', #11568, #23021, #9526 ) ;
#24194 = ORIENTED_EDGE ( 'NONE', *, *, #15768, .F. ) ;
#24195 = ADVANCED_FACE ( 'NONE', ( #34505 ), #8813, .F. ) ;
#24196 = CARTESIAN_POINT ( 'NONE',  ( 0.000000000000000000, 0.000000000000000000, -5.000000000000000000 ) ) ;
#24197 = ORIENTED_EDGE ( 'NONE', *, *, #33329, .F. ) ;
#24198 = CARTESIAN_POINT ( 'NONE',  ( -75.00000337463097821, 25.98076211353318854, -5.000000000000000000 ) ) ;
#24199 = CIRCLE ( 'NONE', #8033, 3.500000000000000888 ) ;
#24200 = DIRECTION ( 'NONE',  ( 0.000000000000000000, 0.000000000000000000, 1.000000000000000000 ) ) ;
#24201 = AXIS2_PLACEMENT_3D ( 'NONE', #8822, #17276, #3029 ) ;
#24202 = DIRECTION ( 'NONE',  ( 0.000000000000000000, 0.000000000000000000, 1.000000000000000000 ) ) ;
#24203 = ORIENTED_EDGE ( 'NONE', *, *, #25459, .F. ) ;
#24204 = ORIENTED_EDGE ( 'NONE', *, *, #22365, .T. ) ;
#24205 = ORIENTED_EDGE ( 'NONE', *, *, #25717, .T. ) ;
#24206 = CARTESIAN_POINT ( 'NONE',  ( 17.55872235085559652, 89.94802294027088863, -23.00000000000000000 ) ) ;
#24207 = EDGE_CURVE ( 'NONE', #18201, #34855, #20859, .T. ) ;
#24208 = CARTESIAN_POINT ( 'NONE',  ( -12.97563234535667753, 90.60231327712331506, -49.86561046011506448 ) ) ;
#24209 = AXIS2_PLACEMENT_3D ( 'NONE', #12340, #23998, #15170 ) ;
#24210 = DIRECTION ( 'NONE',  ( 1.000000000000000000, 0.000000000000000000, 0.000000000000000000 ) ) ;
#24211 = DIRECTION ( 'NONE',  ( -0.4999999999999979461, 0.8660254037844397068, 0.000000000000000000 ) ) ;
#24212 = DIRECTION ( 'NONE',  ( 0.000000000000000000, 0.000000000000000000, 1.000000000000000000 ) ) ;
#24213 = ORIENTED_EDGE ( 'NONE', *, *, #15291, .F. ) ;
#24214 = DIRECTION ( 'NONE',  ( -1.000000000000000000, 0.000000000000000000, 0.000000000000000000 ) ) ;
#24215 = VECTOR ( 'NONE', #10984, 1000.000000000000000 ) ;
#24216 = DIRECTION ( 'NONE',  ( 0.000000000000000000, 0.000000000000000000, 1.000000000000000000 ) ) ;
#24217 = ORIENTED_EDGE ( 'NONE', *, *, #17644, .F. ) ;
#24218 = DIRECTION ( 'NONE',  ( 0.000000000000000000, 0.000000000000000000, 1.000000000000000000 ) ) ;
#24219 = EDGE_CURVE ( 'NONE', #8433, #33109, #29597, .T. ) ;
#24220 = CYLINDRICAL_SURFACE ( 'NONE', #32729, 2.000000000000001776 ) ;
#24221 = AXIS2_PLACEMENT_3D ( 'NONE', #10110, #26788, #27144 ) ;
#24222 = ORIENTED_EDGE ( 'NONE', *, *, #12880, .T. ) ;
#24223 = CIRCLE ( 'NONE', #12837, 95.00000000000000000 ) ;
#24224 = ORIENTED_EDGE ( 'NONE', *, *, #10619, .F. ) ;
#24225 = EDGE_CURVE ( 'NONE', #35478, #17057, #35448, .T. ) ;
#24226 = CARTESIAN_POINT ( 'NONE',  ( 35.83991598322140248, 56.52018970185221036, -4.999999999999997335 ) ) ;
#24227 = DIRECTION ( 'NONE',  ( 1.000000000000000000, 0.000000000000000000, 0.000000000000000000 ) ) ;
#24228 = LINE ( 'NONE', #1186, #21423 ) ;
#24229 = EDGE_LOOP ( 'NONE', ( #29449, #20988, #11533, #20284, #14237 ) ) ;
#24230 = VERTEX_POINT ( 'NONE', #15003 ) ;
#24231 = VERTEX_POINT ( 'NONE', #32599 ) ;
#24232 = CARTESIAN_POINT ( 'NONE',  ( 0.000000000000000000, 0.000000000000000000, 2.266666666667000563 ) ) ;
#24233 = AXIS2_PLACEMENT_3D ( 'NONE', #26058, #23061, #31845 ) ;
#24234 = ORIENTED_EDGE ( 'NONE', *, *, #35783, .F. ) ;
#24235 = AXIS2_PLACEMENT_3D ( 'NONE', #14533, #36678, #22415 ) ;
#24236 = EDGE_LOOP ( 'NONE', ( #20723, #36071, #18432, #31433 ) ) ;
#24237 = DIRECTION ( 'NONE',  ( -0.000000000000000000, -0.000000000000000000, 1.000000000000000000 ) ) ;
#24238 = VERTEX_POINT ( 'NONE', #9733 ) ;
#24239 = ORIENTED_EDGE ( 'NONE', *, *, #27473, .F. ) ;
#24240 = VECTOR ( 'NONE', #7692, 1000.000000000000000 ) ;
#24241 = EDGE_CURVE ( 'NONE', #28829, #24245, #13071, .T. ) ;
#24242 = CARTESIAN_POINT ( 'NONE',  ( -5.750000000000035527, 83.21147890756138565, 32.49999999999999289 ) ) ;
#24243 = DIRECTION ( 'NONE',  ( 1.000000000000000000, 0.000000000000000000, 0.000000000000000000 ) ) ;
#24244 = ORIENTED_EDGE ( 'NONE', *, *, #23154, .F. ) ;
#24245 = VERTEX_POINT ( 'NONE', #18368 ) ;
#24246 = FACE_OUTER_BOUND ( 'NONE', #24274, .T. ) ;
#24247 = DIRECTION ( 'NONE',  ( 0.000000000000000000, 0.000000000000000000, -1.000000000000000000 ) ) ;
#24248 = AXIS2_PLACEMENT_3D ( 'NONE', #29539, #1060, #7065 ) ;
#24249 = ADVANCED_FACE ( 'NONE', ( #737, #29240 ), #3569, .F. ) ;
#24250 = FACE_OUTER_BOUND ( 'NONE', #36197, .T. ) ;
#24251 = AXIS2_PLACEMENT_3D ( 'NONE', #19282, #24905, #24719 ) ;
#24252 = DIRECTION ( 'NONE',  ( 0.000000000000000000, 0.000000000000000000, 1.000000000000000000 ) ) ;
#24253 = EDGE_LOOP ( 'NONE', ( #31068, #8767, #6845, #26169 ) ) ;
#24254 = CARTESIAN_POINT ( 'NONE',  ( 56.67878100130369035, -27.78182860042797131, -4.999999999999997335 ) ) ;
#24256 = EDGE_LOOP ( 'NONE', ( #9834, #19106, #28992, #20067, #143 ) ) ;
#24255 = EDGE_CURVE ( 'NONE', #1094, #30126, #2922, .T. ) ;
#24257 = DIRECTION ( 'NONE',  ( 1.000000000000000000, 0.000000000000000000, 0.000000000000000000 ) ) ;
#24258 = CARTESIAN_POINT ( 'NONE',  ( 0.000000000000000000, 0.000000000000000000, 27.50000000000000000 ) ) ;
#24259 = DIRECTION ( 'NONE',  ( 0.000000000000000000, 0.000000000000000000, 1.000000000000000000 ) ) ;
#24260 = DIRECTION ( 'NONE',  ( 1.000000000000000000, 0.000000000000000000, 0.000000000000000000 ) ) ;
#24261 = CARTESIAN_POINT ( 'NONE',  ( 0.000000000000000000, 0.000000000000000000, -6.000000000000000000 ) ) ;
#24262 = CARTESIAN_POINT ( 'NONE',  ( 69.99999662536839651, 17.32050807568879236, -9.999999999999998224 ) ) ;
#24263 = AXIS2_PLACEMENT_3D ( 'NONE', #1974, #32735, #7061 ) ;
#24264 = CARTESIAN_POINT ( 'NONE',  ( 5.000000000000000000, 2.488344183252611419, -1.689918788536298289 ) ) ;
#24265 = EDGE_LOOP ( 'NONE', ( #18548, #33827, #11680 ) ) ;
#24267 = VECTOR ( 'NONE', #31771, 1000.000000000000000 ) ;
#24266 = DIRECTION ( 'NONE',  ( -1.000000000000000000, 0.000000000000000000, 0.000000000000000000 ) ) ;
#24268 = CARTESIAN_POINT ( 'NONE',  ( -10.00000337463127842, -69.28203230275519786, -9.999999999999998224 ) ) ;
#24269 = DIRECTION ( 'NONE',  ( 0.000000000000000000, 0.000000000000000000, 1.000000000000000000 ) ) ;
#24270 = AXIS2_PLACEMENT_3D ( 'NONE', #27132, #7275, #26775 ) ;
#24271 = VERTEX_POINT ( 'NONE', #1299 ) ;
#24272 = CIRCLE ( 'NONE', #8110, 2.000000000000001776 ) ;
#24273 = ORIENTED_EDGE ( 'NONE', *, *, #21115, .T. ) ;
#24274 = EDGE_LOOP ( 'NONE', ( #5198, #5948, #33764, #27201 ) ) ;
#24275 = ADVANCED_FACE ( 'NONE', ( #4127 ), #15364, .T. ) ;
#24276 = CARTESIAN_POINT ( 'NONE',  ( 6.249999999999998224, 3.980102097228899218E-16, 3.250000000000001332 ) ) ;
#24277 = CARTESIAN_POINT ( 'NONE',  ( 87.99999662536828282, 2.449293598294703949E-16, -5.000000000000000000 ) ) ;
#24278 = CARTESIAN_POINT ( 'NONE',  ( -2.000003374631303732, -86.60254037844400443, 12.50000000000000000 ) ) ;
#24279 = ORIENTED_EDGE ( 'NONE', *, *, #28921, .T. ) ;
#24280 = AXIS2_PLACEMENT_3D ( 'NONE', #6492, #6289, #20528 ) ;
#24281 = AXIS2_PLACEMENT_3D ( 'NONE', #21514, #12681, #3707 ) ;
#24282 = CARTESIAN_POINT ( 'NONE',  ( 0.000000000000000000, 0.000000000000000000, -5.000000000000000000 ) ) ;
#24283 = DIRECTION ( 'NONE',  ( 1.000000000000000000, 0.000000000000000000, 0.000000000000000000 ) ) ;
#24284 = VERTEX_POINT ( 'NONE', #17996 ) ;
#24285 = DIRECTION ( 'NONE',  ( -0.000000000000000000, -0.000000000000000000, -1.000000000000000000 ) ) ;
#24286 = VERTEX_POINT ( 'NONE', #29422 ) ;
#24287 = DIRECTION ( 'NONE',  ( -1.000000000000000000, 0.000000000000000000, 0.000000000000000000 ) ) ;
#24288 = EDGE_CURVE ( 'NONE', #11378, #25226, #24465, .T. ) ;
#24289 = LINE ( 'NONE', #13232, #20181 ) ;
#24290 = DIRECTION ( 'NONE',  ( 1.000000000000000000, 0.000000000000000000, 0.000000000000000000 ) ) ;
#24291 = CIRCLE ( 'NONE', #15319, 2.000000000000001776 ) ;
#24292 = CARTESIAN_POINT ( 'NONE',  ( 87.99999662536828282, 2.449293598294706414E-16, -9.999999999999998224 ) ) ;
#24293 = ADVANCED_FACE ( 'NONE', ( #26987 ), #12546, .F. ) ;
#24294 = AXIS2_PLACEMENT_3D ( 'NONE', #34562, #3779, #26471 ) ;
#24295 = ORIENTED_EDGE ( 'NONE', *, *, #11380, .F. ) ;
#24296 = CARTESIAN_POINT ( 'NONE',  ( 5.000000000000000000, 2.419979747126332903, -5.688163366729713566 ) ) ;
#24297 = CIRCLE ( 'NONE', #22502, 2.000000000000001776 ) ;
#24298 = AXIS2_PLACEMENT_3D ( 'NONE', #10313, #19150, #7503 ) ;
#24299 = ITEM_DEFINED_TRANSFORMATION ( 'NONE', 'NONE', #32119,  #21385 ) ;
#24300 = CIRCLE ( 'NONE', #18301, 2.000000000000001776 ) ;
#24301 = EDGE_CURVE ( 'NONE', #17303, #32102, #29231, .T. ) ;
#24302 = CIRCLE ( 'NONE', #14092, 2.500000000000000000 ) ;
#24303 = CARTESIAN_POINT ( 'NONE',  ( -31.74999999999995737, 0.000000000000000000, 3.000000000000000888 ) ) ;
#24304 = DIRECTION ( 'NONE',  ( 1.000000000000000000, 0.000000000000000000, 0.000000000000000000 ) ) ;
#24305 = DIRECTION ( 'NONE',  ( -0.000000000000000000, -0.000000000000000000, 1.000000000000000000 ) ) ;
#24306 = ORIENTED_EDGE ( 'NONE', *, *, #27886, .F. ) ;
#24307 = CARTESIAN_POINT ( 'NONE',  ( 64.99999662536842493, 43.30127018922200222, 17.49999999999999645 ) ) ;
#24308 = EDGE_CURVE ( 'NONE', #15434, #26833, #21458, .T. ) ;
#24309 = DIRECTION ( 'NONE',  ( -0.000000000000000000, -0.000000000000000000, -1.000000000000000000 ) ) ;
#24310 = DIRECTION ( 'NONE',  ( 0.000000000000000000, 0.000000000000000000, -1.000000000000000000 ) ) ;
#24311 = EDGE_CURVE ( 'NONE', #5101, #10635, #27450, .T. ) ;
#24312 = VECTOR ( 'NONE', #18544, 1000.000000000000000 ) ;
#24313 = VERTEX_POINT ( 'NONE', #23554 ) ;
#24314 = ORIENTED_EDGE ( 'NONE', *, *, #33872, .T. ) ;
#24315 = B_SPLINE_CURVE_WITH_KNOTS ( 'NONE', 3,
 ( #10132, #25675, #35186, #25472, #22671, #19477 ),
 .UNSPECIFIED., .F., .F.,
 ( 4, 2, 4 ),
 ( 0.002950759650825637587, 0.004429055062152260219, 0.005907350473478882417 ),
 .UNSPECIFIED. ) ;
#24316 = PLANE ( 'NONE',  #24960 ) ;
#24317 = DIRECTION ( 'NONE',  ( 1.000000000000000000, -1.850371707708594366E-15, 0.000000000000000000 ) ) ;
#24318 = ADVANCED_FACE ( 'NONE', ( #29177 ), #23002, .F. ) ;
#24319 = EDGE_CURVE ( 'NONE', #29609, #5247, #11738, .T. ) ;
#24320 = CARTESIAN_POINT ( 'NONE',  ( 7.999996625368618552, 69.28203230275516944, -9.999999999999998224 ) ) ;
#24321 = ORIENTED_EDGE ( 'NONE', *, *, #8853, .F. ) ;
#24322 = ADVANCED_FACE ( 'NONE', ( #12091, #11549, #34269, #17943, #34448, #20731, #20193 ), #28629, .F. ) ;
#24323 = CIRCLE ( 'NONE', #15345, 2.000000000000001776 ) ;
#24324 = EDGE_CURVE ( 'NONE', #25888, #4290, #28674, .T. ) ;
#24325 = FACE_OUTER_BOUND ( 'NONE', #14664, .T. ) ;
#24326 = FACE_OUTER_BOUND ( 'NONE', #29065, .T. ) ;
#24327 = ADVANCED_FACE ( 'NONE', ( #26191 ), #32168, .F. ) ;
#24328 = CARTESIAN_POINT ( 'NONE',  ( 5.749999999999999112, 96.68456697298042002, -25.00000000000000000 ) ) ;
#24329 = AXIS2_PLACEMENT_3D ( 'NONE', #9836, #35924, #7407 ) ;
#24330 = AXIS2_PLACEMENT_3D ( 'NONE', #27180, #34899, #21015 ) ;
#24331 = CARTESIAN_POINT ( 'NONE',  ( -82.47399748121956975, 72.51968985770598408, 32.50000000000001421 ) ) ;
#24332 = AXIS2_PLACEMENT_3D ( 'NONE', #11754, #20955, #20393 ) ;
#24333 = VERTEX_POINT ( 'NONE', #23197 ) ;
#24334 = AXIS2_PLACEMENT_3D ( 'NONE', #5141, #25036, #16580 ) ;
#24335 = VERTEX_POINT ( 'NONE', #31623 ) ;
#24336 = CARTESIAN_POINT ( 'NONE',  ( 69.99999662536839651, -17.32050807568879947, 12.50000000000000000 ) ) ;
#24337 = AXIS2_PLACEMENT_3D ( 'NONE', #1856, #28094, #5419 ) ;
#24338 = CARTESIAN_POINT ( 'NONE',  ( -52.00000337463112032, -51.96152422706641971, -9.999999999999998224 ) ) ;
#24339 = VERTEX_POINT ( 'NONE', #6504 ) ;
#24340 = DIRECTION ( 'NONE',  ( 1.000000000000000000, 0.000000000000000000, 0.000000000000000000 ) ) ;
#24341 = ORIENTED_EDGE ( 'NONE', *, *, #34953, .T. ) ;
#24342 = CARTESIAN_POINT ( 'NONE',  ( -87.00000337463093558, -25.98076211353322051, -9.999999999999998224 ) ) ;
#24343 = AXIS2_PLACEMENT_3D ( 'NONE', #25233, #2529, #13952 ) ;
#24344 = DIRECTION ( 'NONE',  ( 0.000000000000000000, 0.000000000000000000, 1.000000000000000000 ) ) ;
#24345 = VERTEX_POINT ( 'NONE', #9112 ) ;
#24346 = ORIENTED_EDGE ( 'NONE', *, *, #35075, .T. ) ;
#24347 = CARTESIAN_POINT ( 'NONE',  ( 0.000000000000000000, 0.000000000000000000, -5.000000000000000000 ) ) ;
#24348 = ORIENTED_EDGE ( 'NONE', *, *, #13572, .F. ) ;
#24349 = AXIS2_PLACEMENT_3D ( 'NONE', #15210, #35106, #3772 ) ;
#24350 = DIRECTION ( 'NONE',  ( 0.5000000000000039968, 0.8660254037844363761, 0.000000000000000000 ) ) ;
#24351 = AXIS2_PLACEMENT_3D ( 'NONE', #4129, #24740, #26989 ) ;
#24352 = DIRECTION ( 'NONE',  ( 1.000000000000000000, 0.000000000000000000, 0.000000000000000000 ) ) ;
#24353 = CARTESIAN_POINT ( 'NONE',  ( -67.00000337463104927, -25.98076211353322051, -9.999999999999998224 ) ) ;
#24354 = ORIENTED_EDGE ( 'NONE', *, *, #7907, .T. ) ;
#24355 = PLANE ( 'NONE',  #26236 ) ;
#24356 = AXIS2_PLACEMENT_3D ( 'NONE', #29971, #861, #26549 ) ;
#24357 = CARTESIAN_POINT ( 'NONE',  ( 2.778182860043481028, 66.86787810013034061, 12.49999999999999822 ) ) ;
#24358 = CIRCLE ( 'NONE', #8195, 3.000000000000001332 ) ;
#24359 = ORIENTED_EDGE ( 'NONE', *, *, #31954, .T. ) ;
#24360 = AXIS2_PLACEMENT_3D ( 'NONE', #15696, #10429, #24520 ) ;
#24361 = CIRCLE ( 'NONE', #33949, 2.000000000000000000 ) ;
#24362 = ORIENTED_EDGE ( 'NONE', *, *, #20307, .T. ) ;
#24363 = CIRCLE ( 'NONE', #12338, 2.000000000000001776 ) ;
#24364 = ORIENTED_EDGE ( 'NONE', *, *, #16458, .T. ) ;
#24365 = LINE ( 'NONE', #18365, #14034 ) ;
#24366 = DIRECTION ( 'NONE',  ( 0.000000000000000000, -1.000000000000000000, 1.034244904716769672E-15 ) ) ;
#24367 = ORIENTED_EDGE ( 'NONE', *, *, #10591, .F. ) ;
#24368 = DIRECTION ( 'NONE',  ( -1.000000000000000000, 0.000000000000000000, -0.000000000000000000 ) ) ;
#24369 = DIRECTION ( 'NONE',  ( 0.000000000000000000, 0.000000000000000000, -1.000000000000000000 ) ) ;
#24370 = VERTEX_POINT ( 'NONE', #5761 ) ;
#24371 = CARTESIAN_POINT ( 'NONE',  ( -2.000003374631334818, 69.28203230275516944, -9.999999999999998224 ) ) ;
#24372 = AXIS2_PLACEMENT_3D ( 'NONE', #8105, #30981, #5313 ) ;
#24373 = EDGE_CURVE ( 'NONE', #14204, #33302, #18498, .T. ) ;
#24374 = LINE ( 'NONE', #35825, #20412 ) ;
#24375 = EDGE_CURVE ( 'NONE', #23282, #11624, #1141, .T. ) ;
#24376 = DIRECTION ( 'NONE',  ( -0.000000000000000000, -0.000000000000000000, 1.000000000000000000 ) ) ;
#24377 = CARTESIAN_POINT ( 'NONE',  ( -82.00000337463096400, -34.64101615137762025, -9.999999999999998224 ) ) ;
#24378 = CYLINDRICAL_SURFACE ( 'NONE', #16600, 3.500000000000003109 ) ;
#24379 = AXIS2_PLACEMENT_3D ( 'NONE', #13257, #30520, #16268 ) ;
#24380 = CARTESIAN_POINT ( 'NONE',  ( 6.726859516510129033, 0.000000000000000000, -4.599999999999999645 ) ) ;
#24381 = VERTEX_POINT ( 'NONE', #28805 ) ;
#24382 = CIRCLE ( 'NONE', #12987, 2.000000000000001776 ) ;
#24383 = ORIENTED_EDGE ( 'NONE', *, *, #3953, .T. ) ;
#24384 = DIRECTION ( 'NONE',  ( 1.000000000000000000, 0.000000000000000000, 0.000000000000000000 ) ) ;
#24385 = AXIS2_PLACEMENT_3D ( 'NONE', #17717, #15095, #31941 ) ;
#24386 = AXIS2_PLACEMENT_3D ( 'NONE', #11094, #25746, #22542 ) ;
#24387 = CARTESIAN_POINT ( 'NONE',  ( 66.99999662536839651, -43.30127018922199511, 12.50000000000000000 ) ) ;
#24388 = CARTESIAN_POINT ( 'NONE',  ( -67.30619744048885877, 84.18124734178336155, 27.50000000000000000 ) ) ;
#24389 = DIRECTION ( 'NONE',  ( -1.000000000000000000, 0.000000000000000000, 0.000000000000000000 ) ) ;
#24390 = EDGE_CURVE ( 'NONE', #12599, #20765, #29746, .T. ) ;
#24391 = VERTEX_POINT ( 'NONE', #5957 ) ;
#24392 = VECTOR ( 'NONE', #2711, 1000.000000000000000 ) ;
#24394 = AXIS2_PLACEMENT_3D ( 'NONE', #12725, #9744, #7135 ) ;
#24393 = CARTESIAN_POINT ( 'NONE',  ( 62.99999662536841072, 25.98076211353318854, -9.999999999999998224 ) ) ;
#24395 = DIRECTION ( 'NONE',  ( 0.000000000000000000, 0.000000000000000000, 1.000000000000000000 ) ) ;
#24396 = AXIS2_PLACEMENT_3D ( 'NONE', #22810, #28950, #14163 ) ;
#24397 = ORIENTED_EDGE ( 'NONE', *, *, #24044, .T. ) ;
#24398 = FACE_OUTER_BOUND ( 'NONE', #36759, .T. ) ;
#24399 = VERTEX_POINT ( 'NONE', #14193 ) ;
#24400 = CIRCLE ( 'NONE', #27388, 2.000000000000001776 ) ;
#24401 = ADVANCED_FACE ( 'NONE', ( #11926 ), #17389, .F. ) ;
#24402 = FACE_OUTER_BOUND ( 'NONE', #28676, .T. ) ;
#24403 = AXIS2_PLACEMENT_3D ( 'NONE', #33390, #5449, #30381 ) ;
#24404 = CARTESIAN_POINT ( 'NONE',  ( 67.99999662536836809, -34.64101615137759183, 12.50000000000000000 ) ) ;
#24405 = CARTESIAN_POINT ( 'NONE',  ( 5.000000000000000000, 2.886751345948134428, -2.080000000000000071 ) ) ;
#24406 = ORIENTED_EDGE ( 'NONE', *, *, #30490, .F. ) ;
#24407 = ORIENTED_EDGE ( 'NONE', *, *, #10744, .F. ) ;
#24408 = AXIS2_PLACEMENT_3D ( 'NONE', #10931, #22202, #19376 ) ;
#24409 = AXIS2_PLACEMENT_3D ( 'NONE', #17647, #213, #34745 ) ;
#24410 = EDGE_CURVE ( 'NONE', #3167, #6253, #36455, .T. ) ;
#24411 = AXIS2_PLACEMENT_3D ( 'NONE', #11659, #2688, #36817 ) ;
#24412 = VERTEX_POINT ( 'NONE', #17741 ) ;
#24413 = CARTESIAN_POINT ( 'NONE',  ( 4.242640687119292764, 4.242640687119187071, 32.50000000000000000 ) ) ;
#24414 = FACE_BOUND ( 'NONE', #17304, .T. ) ;
#24415 = CARTESIAN_POINT ( 'NONE',  ( -52.00000337463109190, 69.28203230275518365, 17.49999999999999645 ) ) ;
#24416 = CARTESIAN_POINT ( 'NONE',  ( -83.67710216016716629, 27.48073957228723430, 12.50000000000000000 ) ) ;
#24417 = DIRECTION ( 'NONE',  ( -1.000000000000000000, -0.000000000000000000, -0.000000000000000000 ) ) ;
#24418 = EDGE_LOOP ( 'NONE', ( #1565, #4895 ) ) ;
#24419 = PLANE ( 'NONE',  #21831 ) ;
#24420 = AXIS2_PLACEMENT_3D ( 'NONE', #29673, #12618, #17891 ) ;
#24421 = CARTESIAN_POINT ( 'NONE',  ( -62.97617850287781494, -4.279621169095772615, 12.49999999999999822 ) ) ;
#24422 = EDGE_CURVE ( 'NONE', #4180, #14960, #26863, .T. ) ;
#24423 = DIRECTION ( 'NONE',  ( -0.000000000000000000, -0.8660254037844413721, -0.4999999999999952816 ) ) ;
#24424 = ORIENTED_EDGE ( 'NONE', *, *, #35551, .T. ) ;
#24425 = DIRECTION ( 'NONE',  ( -0.8660254037844380415, 0.5000000000000009992, 0.000000000000000000 ) ) ;
#24426 = CARTESIAN_POINT ( 'NONE',  ( -47.63139720814380951, 27.50000000000055422, 5.000000000000000888 ) ) ;
#24427 = AXIS2_PLACEMENT_3D ( 'NONE', #25804, #26155, #12239 ) ;
#24428 = VERTEX_POINT ( 'NONE', #3513 ) ;
#24429 = ORIENTED_EDGE ( 'NONE', *, *, #35048, .T. ) ;
#24430 = AXIS2_PLACEMENT_3D ( 'NONE', #34582, #17495, #26673 ) ;
#24431 = DIRECTION ( 'NONE',  ( -1.000000000000000000, 0.000000000000000000, -0.000000000000000000 ) ) ;
#24432 = LINE ( 'NONE', #35872, #25376 ) ;
#24433 = FACE_OUTER_BOUND ( 'NONE', #1458, .T. ) ;
#24434 = EDGE_LOOP ( 'NONE', ( #6785, #701, #29322, #22501 ) ) ;
#24435 = ORIENTED_EDGE ( 'NONE', *, *, #12113, .T. ) ;
#24436 = AXIS2_PLACEMENT_3D ( 'NONE', #13985, #13821, #2392 ) ;
#24437 = CIRCLE ( 'NONE', #1057, 2.000000000000001776 ) ;
#24438 = ORIENTED_EDGE ( 'NONE', *, *, #137, .F. ) ;
#24439 = VECTOR ( 'NONE', #35576, 1000.000000000000000 ) ;
#24440 = DIRECTION ( 'NONE',  ( 1.000000000000000000, 0.000000000000000000, 0.000000000000000000 ) ) ;
#24441 = CIRCLE ( 'NONE', #8274, 2.000000000000001776 ) ;
#24442 = ORIENTED_EDGE ( 'NONE', *, *, #33140, .F. ) ;
#24443 = EDGE_CURVE ( 'NONE', #19786, #11022, #26376, .T. ) ;
#24444 = VERTEX_POINT ( 'NONE', #3466 ) ;
#24445 = DIRECTION ( 'NONE',  ( -0.7071067811865539010, -0.7071067811865411334, 0.000000000000000000 ) ) ;
#24446 = ORIENTED_EDGE ( 'NONE', *, *, #30515, .F. ) ;
#24447 = EDGE_CURVE ( 'NONE', #37014, #27017, #16702, .T. ) ;
#24448 = VERTEX_POINT ( 'NONE', #31760 ) ;
#24449 = CIRCLE ( 'NONE', #35241, 2.000000000000001776 ) ;
#24450 = CARTESIAN_POINT ( 'NONE',  ( 0.000000000000000000, 0.000000000000000000, -5.000000000000000000 ) ) ;
#24451 = FACE_OUTER_BOUND ( 'NONE', #22596, .T. ) ;
#24452 = ORIENTED_EDGE ( 'NONE', *, *, #23433, .F. ) ;
#24453 = EDGE_CURVE ( 'NONE', #3457, #30601, #23516, .T. ) ;
#24454 = EDGE_LOOP ( 'NONE', ( #36984, #7508 ) ) ;
#24455 = LINE ( 'NONE', #35895, #31664 ) ;
#24456 = CARTESIAN_POINT ( 'NONE',  ( -33.00000337463116296, -60.62177826491080168, -5.000000000000000000 ) ) ;
#24457 = LINE ( 'NONE', #26694, #17464 ) ;
#24458 = CARTESIAN_POINT ( 'NONE',  ( -5.248988766908547099, 2.532174945215621253, -4.266961984436636435 ) ) ;
#24459 = EDGE_CURVE ( 'NONE', #30221, #22077, #17514, .T. ) ;
#24460 = ORIENTED_EDGE ( 'NONE', *, *, #33227, .T. ) ;
#24461 = CYLINDRICAL_SURFACE ( 'NONE', #7595, 2.000000000000000000 ) ;
#24462 = CIRCLE ( 'NONE', #19058, 2.000000000000001776 ) ;
#24463 = ORIENTED_EDGE ( 'NONE', *, *, #8447, .F. ) ;
#24464 = CARTESIAN_POINT ( 'NONE',  ( 0.000000000000000000, 81.28776890242656350, -29.99999999999985434 ) ) ;
#24465 = CIRCLE ( 'NONE', #8306, 2.000000000000000000 ) ;
#24466 = CARTESIAN_POINT ( 'NONE',  ( 0.000000000000000000, 0.000000000000000000, -5.000000000000000000 ) ) ;
#24467 = DIRECTION ( 'NONE',  ( 1.000000000000000000, 9.251858538542971828E-16, 0.000000000000000000 ) ) ;
#24468 = DIRECTION ( 'NONE',  ( -1.000000000000000000, 0.000000000000000000, 0.000000000000000000 ) ) ;
#24470 = CIRCLE ( 'NONE', #1710, 2.000000000000001776 ) ;
#24469 = DIRECTION ( 'NONE',  ( 0.000000000000000000, 0.000000000000000000, -1.000000000000000000 ) ) ;
#24471 = DIRECTION ( 'NONE',  ( 0.000000000000000000, 0.000000000000000000, 1.000000000000000000 ) ) ;
#24472 = CIRCLE ( 'NONE', #25096, 2.000000000000001776 ) ;
#24473 = EDGE_CURVE ( 'NONE', #25394, #24524, #22108, .T. ) ;
#24474 = CARTESIAN_POINT ( 'NONE',  ( 110.2237710830536770, 101.7384897088147397, 27.50000000000000000 ) ) ;
#24475 = ORIENTED_EDGE ( 'NONE', *, *, #3481, .T. ) ;
#24476 = LINE ( 'NONE', #7399, #27373 ) ;
#24477 = FACE_OUTER_BOUND ( 'NONE', #1317, .T. ) ;
#24478 = CYLINDRICAL_SURFACE ( 'NONE', #4966, 2.000000000000001776 ) ;
#24479 = AXIS2_PLACEMENT_3D ( 'NONE', #15579, #27005, #21382 ) ;
#24480 = EDGE_LOOP ( 'NONE', ( #34698, #6431, #35071, #888 ) ) ;
#24481 = CIRCLE ( 'NONE', #15479, 2.000000000000001776 ) ;
#24482 = ORIENTED_EDGE ( 'NONE', *, *, #6661, .T. ) ;
#24483 = ORIENTED_EDGE ( 'NONE', *, *, #28430, .T. ) ;
#24484 = FACE_OUTER_BOUND ( 'NONE', #1420, .T. ) ;
#24485 = LINE ( 'NONE', #3673, #2891 ) ;
#24486 = ORIENTED_EDGE ( 'NONE', *, *, #21822, .T. ) ;
#24487 = EDGE_CURVE ( 'NONE', #985, #12428, #9075, .T. ) ;
#24488 = PRODUCT_DEFINITION_SHAPE ( 'NONE', 'NONE',  #37121 ) ;
#24489 = DIRECTION ( 'NONE',  ( 0.000000000000000000, 0.000000000000000000, 1.000000000000000000 ) ) ;
#24490 = AXIS2_PLACEMENT_3D ( 'NONE', #162, #34493, #11784 ) ;
#24491 = CARTESIAN_POINT ( 'NONE',  ( -65.00000337463104927, -25.98076211353322051, 12.50000000000000000 ) ) ;
#24492 = ORIENTED_EDGE ( 'NONE', *, *, #16794, .T. ) ;
#24493 = EDGE_CURVE ( 'NONE', #14843, #18158, #14897, .T. ) ;
#24494 = CARTESIAN_POINT ( 'NONE',  ( -60.00000337463104216, 51.96152422706639129, 12.50000000000000000 ) ) ;
#24495 = ORIENTED_EDGE ( 'NONE', *, *, #27739, .T. ) ;
#24496 = CONICAL_SURFACE ( 'NONE', #22690, 3.050000000000000711, 0.7853981633974498333 ) ;
#24497 = DIRECTION ( 'NONE',  ( 1.000000000000000000, 0.000000000000000000, 0.000000000000000000 ) ) ;
#24498 = DIRECTION ( 'NONE',  ( 0.000000000000000000, 0.000000000000000000, 1.000000000000000000 ) ) ;
#24499 = CARTESIAN_POINT ( 'NONE',  ( 5.253368672218635460, -3.033033817057790404, -4.359491423763655504 ) ) ;
#24500 = VECTOR ( 'NONE', #15801, 1000.000000000000000 ) ;
#24501 = ADVANCED_FACE ( 'NONE', ( #26336 ), #34956, .F. ) ;
#24502 = ORIENTED_EDGE ( 'NONE', *, *, #17585, .F. ) ;
#24503 = DIRECTION ( 'NONE',  ( 1.000000000000000000, 0.000000000000000000, 0.000000000000000000 ) ) ;
#24504 = AXIS2_PLACEMENT_3D ( 'NONE', #33933, #147, #16692 ) ;
#24505 = FACE_OUTER_BOUND ( 'NONE', #12908, .T. ) ;
#24506 = FACE_OUTER_BOUND ( 'NONE', #33087, .T. ) ;
#24507 = AXIS2_PLACEMENT_3D ( 'NONE', #11194, #22831, #17006 ) ;
#24508 = ADVANCED_FACE ( 'NONE', ( #6259 ), #24496, .F. ) ;
#24509 = CARTESIAN_POINT ( 'NONE',  ( 32.99999662536853862, 77.94228634059959404, -5.000000000000000000 ) ) ;
#24510 = CARTESIAN_POINT ( 'NONE',  ( 69.99999662536839651, 34.64101615137758472, 12.50000000000000000 ) ) ;
#24511 = ORIENTED_EDGE ( 'NONE', *, *, #32975, .F. ) ;
#24512 = VECTOR ( 'NONE', #12068, 1000.000000000000000 ) ;
#24513 = CARTESIAN_POINT ( 'NONE',  ( 79.99999662536833966, 17.32050807568879236, -9.999999999999998224 ) ) ;
#24514 = DIRECTION ( 'NONE',  ( 0.000000000000000000, 0.000000000000000000, 1.000000000000000000 ) ) ;
#24515 = CYLINDRICAL_SURFACE ( 'NONE', #24964, 1.999999999999998224 ) ;
#24516 = VERTEX_POINT ( 'NONE', #25960 ) ;
#24517 = AXIS2_PLACEMENT_3D ( 'NONE', #36159, #28263, #10462 ) ;
#24518 = ORIENTED_EDGE ( 'NONE', *, *, #18337, .T. ) ;
#24519 = AXIS2_PLACEMENT_3D ( 'NONE', #2020, #19287, #27538 ) ;
#24520 = DIRECTION ( 'NONE',  ( 1.000000000000000000, 0.000000000000000000, 0.000000000000000000 ) ) ;
#24521 = CARTESIAN_POINT ( 'NONE',  ( 101.4249800177814933, 31.43204461043894327, 27.50000000000000000 ) ) ;
#24522 = CARTESIAN_POINT ( 'NONE',  ( 89.67878100130370456, -27.78182860042797131, -49.86348611802629449 ) ) ;
#24523 = EDGE_CURVE ( 'NONE', #5915, #18905, #29854, .T. ) ;
#24524 = VERTEX_POINT ( 'NONE', #31921 ) ;
#24525 = CIRCLE ( 'NONE', #13727, 65.00000000000000000 ) ;
#24526 = CYLINDRICAL_SURFACE ( 'NONE', #35585, 2.000000000000001776 ) ;
#24527 = CARTESIAN_POINT ( 'NONE',  ( 79.99999662536833966, 34.64101615137759183, 12.50000000000000000 ) ) ;
#24528 = DIRECTION ( 'NONE',  ( 1.000000000000000000, 0.000000000000000000, 0.000000000000000000 ) ) ;
#24530 = CARTESIAN_POINT ( 'NONE',  ( -75.00000337463097821, 43.30127018922197379, -9.999999999999998224 ) ) ;
#24529 = VECTOR ( 'NONE', #29171, 1000.000000000000000 ) ;
#24531 = ORIENTED_EDGE ( 'NONE', *, *, #34311, .T. ) ;
#24532 = EDGE_CURVE ( 'NONE', #5973, #2865, #5334, .T. ) ;
#24533 = ORIENTED_EDGE ( 'NONE', *, *, #10827, .T. ) ;
#24534 = DIRECTION ( 'NONE',  ( 0.000000000000000000, 0.000000000000000000, 1.000000000000000000 ) ) ;
#24535 = VECTOR ( 'NONE', #21848, 1000.000000000000000 ) ;
#24536 = DIRECTION ( 'NONE',  ( 0.4999999999999922839, -0.8660254037844431485, 0.000000000000000000 ) ) ;
#24537 = ORIENTED_EDGE ( 'NONE', *, *, #5529, .T. ) ;
#24538 = EDGE_CURVE ( 'NONE', #20697, #21238, #20148, .T. ) ;
#24539 = CIRCLE ( 'NONE', #19737, 2.000000000000001776 ) ;
#24540 = CARTESIAN_POINT ( 'NONE',  ( 0.03111943836866551752, -6.084399642271208997, -4.366192694417998510 ) ) ;
#24541 = ADVANCED_FACE ( 'NONE', ( #5916 ), #28774, .F. ) ;
#24542 = ORIENTED_EDGE ( 'NONE', *, *, #36442, .T. ) ;
#24543 = DIRECTION ( 'NONE',  ( 0.000000000000000000, 0.000000000000000000, 1.000000000000000000 ) ) ;
#24544 = CARTESIAN_POINT ( 'NONE',  ( -80.00000337463094979, 17.32050807568878525, 12.50000000000000000 ) ) ;
#24545 = CIRCLE ( 'NONE', #21535, 2.000000000000001776 ) ;
#24546 = EDGE_LOOP ( 'NONE', ( #11505, #13056 ) ) ;
#24547 = AXIS2_PLACEMENT_3D ( 'NONE', #1461, #21542, #1663 ) ;
#24548 = CARTESIAN_POINT ( 'NONE',  ( 1.721886139904373003, 5.052888355616772742, -4.057689166958494020 ) ) ;
#24549 = ORIENTED_EDGE ( 'NONE', *, *, #8044, .F. ) ;
#24550 =( NAMED_UNIT ( * ) SI_UNIT ( $, .STERADIAN. ) SOLID_ANGLE_UNIT ( ) );
#24551 = DIRECTION ( 'NONE',  ( -0.000000000000000000, 0.000000000000000000, -1.000000000000000000 ) ) ;
#24552 = EDGE_CURVE ( 'NONE', #3751, #34152, #31643, .T. ) ;
#24553 = LINE ( 'NONE', #5021, #17784 ) ;
#24554 = DIRECTION ( 'NONE',  ( 1.000000000000000000, 0.000000000000000000, -0.000000000000000000 ) ) ;
#24555 = ORIENTED_EDGE ( 'NONE', *, *, #35816, .F. ) ;
#24556 =( REPRESENTATION_RELATIONSHIP ('NONE','NONE', #15268, #22738 ) REPRESENTATION_RELATIONSHIP_WITH_TRANSFORMATION ( #13960 )SHAPE_REPRESENTATION_RELATIONSHIP( ) );
#24557 = DIRECTION ( 'NONE',  ( -1.000000000000000000, 0.000000000000000000, 0.000000000000000000 ) ) ;
#24558 = CARTESIAN_POINT ( 'NONE',  ( -63.00000337463106348, -60.62177826491083010, -9.999999999999998224 ) ) ;
#24559 = DIRECTION ( 'NONE',  ( 1.000000000000000000, 0.000000000000000000, 0.000000000000000000 ) ) ;
#24560 = CIRCLE ( 'NONE', #34725, 27.00000000000001066 ) ;
#24561 = VERTEX_POINT ( 'NONE', #15077 ) ;
#24562 = EDGE_LOOP ( 'NONE', ( #248, #29757, #29403, #24695 ) ) ;
#24563 = VECTOR ( 'NONE', #8050, 1000.000000000000000 ) ;
#24564 = ORIENTED_EDGE ( 'NONE', *, *, #14238, .T. ) ;
#24565 = DIRECTION ( 'NONE',  ( 0.000000000000000000, 0.000000000000000000, 1.000000000000000000 ) ) ;
#24566 = VECTOR ( 'NONE', #31543, 1000.000000000000000 ) ;
#24567 = CARTESIAN_POINT ( 'NONE',  ( 5.749999999999999112, 96.68456697298042002, 32.49999999999999289 ) ) ;
#24568 = ORIENTED_EDGE ( 'NONE', *, *, #33958, .F. ) ;
#24569 = DIRECTION ( 'NONE',  ( 1.224646799147353207E-16, 1.000000000000000000, 0.000000000000000000 ) ) ;
#24570 = CIRCLE ( 'NONE', #9564, 2.000000000000000000 ) ;
#24571 = DIRECTION ( 'NONE',  ( -0.000000000000000000, -0.000000000000000000, 1.000000000000000000 ) ) ;
#24572 = CARTESIAN_POINT ( 'NONE',  ( 72.99999662536836809, -8.660254037844401509, 12.50000000000000000 ) ) ;
#24573 = B_SPLINE_CURVE_WITH_KNOTS ( 'NONE', 3,
 ( #1805, #18863, #12664, #18297, #24296, #15501 ),
 .UNSPECIFIED., .F., .F.,
 ( 4, 2, 4 ),
 ( 0.008070708573309213693, 0.009531758523483289253, 0.01099280847365736308 ),
 .UNSPECIFIED. ) ;
#24574 = CARTESIAN_POINT ( 'NONE',  ( 19.99999662536858835, 69.28203230275516944, -9.999999999999998224 ) ) ;
#24575 = EDGE_CURVE ( 'NONE', #24399, #16885, #34664, .T. ) ;
#24576 = VECTOR ( 'NONE', #6818, 1000.000000000000000 ) ;
#24577 = LINE ( 'NONE', #36561, #5652 ) ;
#24578 = CARTESIAN_POINT ( 'NONE',  ( -80.00000337463094979, 34.64101615137757051, 12.50000000000000000 ) ) ;
#24579 = EDGE_CURVE ( 'NONE', #25853, #23244, #8902, .T. ) ;
#24580 = AXIS2_PLACEMENT_3D ( 'NONE', #33303, #10617, #22064 ) ;
#24581 = CARTESIAN_POINT ( 'NONE',  ( -10.00000337463128730, 69.28203230275516944, -9.999999999999998224 ) ) ;
#24582 = CARTESIAN_POINT ( 'NONE',  ( 35.19434990244975126, -52.39915983220758022, -4.999999999999997335 ) ) ;
#24583 = VERTEX_POINT ( 'NONE', #23346 ) ;
#24584 = VERTEX_POINT ( 'NONE', #29131 ) ;
#24585 = DIRECTION ( 'NONE',  ( 1.000000000000000000, 0.000000000000000000, 0.000000000000000000 ) ) ;
#24586 = CARTESIAN_POINT ( 'NONE',  ( -68.00000337463099243, 51.96152422706637708, -9.999999999999998224 ) ) ;
#24587 = CIRCLE ( 'NONE', #5416, 3.500000000000000888 ) ;
#24588 = DIRECTION ( 'NONE',  ( 0.000000000000000000, 0.000000000000000000, 1.000000000000000000 ) ) ;
#24589 = ADVANCED_FACE ( 'NONE', ( #20337 ), #9461, .T. ) ;
#24590 = EDGE_LOOP ( 'NONE', ( #24668, #900, #9000, #9049 ) ) ;
#24591 = CARTESIAN_POINT ( 'NONE',  ( 69.99999662536839651, 34.64101615137758472, 12.50000000000000000 ) ) ;
#24592 = CARTESIAN_POINT ( 'NONE',  ( -12.00000337463128197, 86.60254037844397601, 12.50000000000000000 ) ) ;
#24593 = CYLINDRICAL_SURFACE ( 'NONE', #23376, 2.000000000000001776 ) ;
#24594 = ORIENTED_EDGE ( 'NONE', *, *, #21070, .T. ) ;
#24595 = DIRECTION ( 'NONE',  ( 1.000000000000000000, 0.000000000000000000, 0.000000000000000000 ) ) ;
#24596 = CIRCLE ( 'NONE', #35370, 2.000000000000001776 ) ;
#24597 = EDGE_LOOP ( 'NONE', ( #7782, #4337 ) ) ;
#24598 = EDGE_CURVE ( 'NONE', #6801, #5741, #2328, .T. ) ;
#24599 = CARTESIAN_POINT ( 'NONE',  ( 42.99999662536848888, 60.62177826491077326, -9.999999999999998224 ) ) ;
#24600 = EDGE_CURVE ( 'NONE', #12497, #13005, #23903, .T. ) ;
#24601 = DIRECTION ( 'NONE',  ( 0.000000000000000000, 0.000000000000000000, 1.000000000000000000 ) ) ;
#24602 = ADVANCED_FACE ( 'NONE', ( #32495 ), #12434, .F. ) ;
#24603 = CARTESIAN_POINT ( 'NONE',  ( -61.25926521283079040, 32.16008401677976281, -4.999999999999997335 ) ) ;
#24604 = EDGE_CURVE ( 'NONE', #22954, #13911, #32257, .T. ) ;
#24605 = VERTEX_POINT ( 'NONE', #12623 ) ;
#24606 = EDGE_LOOP ( 'NONE', ( #11419, #10120, #9033, #36760 ) ) ;
#24607 = DIRECTION ( 'NONE',  ( -0.000000000000000000, 0.000000000000000000, -1.000000000000000000 ) ) ;
#24608 = ORIENTED_EDGE ( 'NONE', *, *, #6212, .F. ) ;
#24609 = CARTESIAN_POINT ( 'NONE',  ( 35.19434990244975126, -52.39915983220758022, 12.49999999999999822 ) ) ;
#24610 = CARTESIAN_POINT ( 'NONE',  ( -72.00000337463100664, -17.32050807568882078, -9.999999999999998224 ) ) ;
#24611 = LINE ( 'NONE', #1903, #18468 ) ;
#24612 = DIRECTION ( 'NONE',  ( 1.000000000000000000, 0.000000000000000000, 0.000000000000000000 ) ) ;
#24613 = CYLINDRICAL_SURFACE ( 'NONE', #11146, 30.00000000000001421 ) ;
#24614 = VERTEX_POINT ( 'NONE', #32888 ) ;
#24615 = DIRECTION ( 'NONE',  ( 1.000000000000000000, 0.000000000000000000, 0.000000000000000000 ) ) ;
#24616 = DIRECTION ( 'NONE',  ( 1.000000000000000000, 0.000000000000000000, 0.000000000000000000 ) ) ;
#24617 = AXIS2_PLACEMENT_3D ( 'NONE', #8420, #31645, #3147 ) ;
#24618 = DIRECTION ( 'NONE',  ( -1.000000000000000000, 0.000000000000000000, 0.000000000000000000 ) ) ;
#24619 = VERTEX_POINT ( 'NONE', #18457 ) ;
#24620 = DIRECTION ( 'NONE',  ( 1.000000000000000000, 0.000000000000000000, 0.000000000000000000 ) ) ;
#24621 = CARTESIAN_POINT ( 'NONE',  ( 82.99999662536832545, 25.98076211353319565, -9.999999999999998224 ) ) ;
#24622 = EDGE_CURVE ( 'NONE', #25195, #24912, #18818, .T. ) ;
#24623 = ORIENTED_EDGE ( 'NONE', *, *, #12116, .T. ) ;
#24624 = ORIENTED_EDGE ( 'NONE', *, *, #31984, .T. ) ;
#24625 = CARTESIAN_POINT ( 'NONE',  ( -80.00000337463094979, 34.64101615137757051, 17.49999999999999645 ) ) ;
#24626 = CARTESIAN_POINT ( 'NONE',  ( 9.999996625368655856, -86.60254037844400443, -9.999999999999998224 ) ) ;
#24627 = CARTESIAN_POINT ( 'NONE',  ( -3.667169054266697259, -3.656261651251520917, -0.8603634151101461347 ) ) ;
#24628 = VERTEX_POINT ( 'NONE', #7206 ) ;
#24629 = VERTEX_POINT ( 'NONE', #36072 ) ;
#24630 = ORIENTED_EDGE ( 'NONE', *, *, #24598, .F. ) ;
#24631 = DIRECTION ( 'NONE',  ( 0.000000000000000000, 0.000000000000000000, 1.000000000000000000 ) ) ;
#24632 = ORIENTED_EDGE ( 'NONE', *, *, #10808, .T. ) ;
#24633 = FACE_OUTER_BOUND ( 'NONE', #11074, .T. ) ;
#24634 = ORIENTED_EDGE ( 'NONE', *, *, #34398, .F. ) ;
#24635 = ORIENTED_EDGE ( 'NONE', *, *, #9805, .T. ) ;
#24636 = DIRECTION ( 'NONE',  ( -0.000000000000000000, -0.000000000000000000, 1.000000000000000000 ) ) ;
#24637 = DIRECTION ( 'NONE',  ( 0.000000000000000000, 0.000000000000000000, 1.000000000000000000 ) ) ;
#24638 = ADVANCED_FACE ( 'NONE', ( #18246 ), #21634, .F. ) ;
#24639 = ORIENTED_EDGE ( 'NONE', *, *, #5667, .T. ) ;
#24640 = ORIENTED_EDGE ( 'NONE', *, *, #6671, .F. ) ;
#24641 = CARTESIAN_POINT ( 'NONE',  ( 69.99999662536838230, -34.64101615137759183, -9.999999999999998224 ) ) ;
#24642 = CARTESIAN_POINT ( 'NONE',  ( 19.13981058454793072, -60.93295298010985306, 12.49999999999999822 ) ) ;
#24643 = DIRECTION ( 'NONE',  ( 0.000000000000000000, 0.000000000000000000, 1.000000000000000000 ) ) ;
#24644 = CARTESIAN_POINT ( 'NONE',  ( 74.99999662536836809, -8.660254037844401509, -9.999999999999998224 ) ) ;
#24645 = ORIENTED_EDGE ( 'NONE', *, *, #11776, .F. ) ;
#24646 = DIRECTION ( 'NONE',  ( 0.000000000000000000, 0.000000000000000000, 1.000000000000000000 ) ) ;
#24647 = VERTEX_POINT ( 'NONE', #30058 ) ;
#24648 = DIRECTION ( 'NONE',  ( 0.000000000000000000, 0.000000000000000000, 1.000000000000000000 ) ) ;
#24649 = DIRECTION ( 'NONE',  ( 0.000000000000000000, 0.000000000000000000, -1.000000000000000000 ) ) ;
#24650 = CARTESIAN_POINT ( 'NONE',  ( -28.00000337463119493, -69.28203230275522628, 17.49999999999999645 ) ) ;
#24651 = CYLINDRICAL_SURFACE ( 'NONE', #26081, 3.499999999999989342 ) ;
#24652 = CARTESIAN_POINT ( 'NONE',  ( 42.99999662536848888, -77.94228634059960825, -9.999999999999998224 ) ) ;
#24653 = CARTESIAN_POINT ( 'NONE',  ( 87.83969979969882047, 14.80603122773025504, -4.999999999999997335 ) ) ;
#24654 = LINE ( 'NONE', #1945, #30138 ) ;
#24655 = ORIENTED_EDGE ( 'NONE', *, *, #33247, .F. ) ;
#24656 = DIRECTION ( 'NONE',  ( 0.000000000000000000, 0.000000000000000000, 1.000000000000000000 ) ) ;
#24657 = AXIS2_PLACEMENT_3D ( 'NONE', #27571, #30175, #7318 ) ;
#24658 = CARTESIAN_POINT ( 'NONE',  ( 42.97377950131529190, 96.90768712682505281, -19.99999999999999645 ) ) ;
#24659 = CARTESIAN_POINT ( 'NONE',  ( -45.00000337463112743, -60.62177826491080168, -5.000000000000000000 ) ) ;
#24660 = EDGE_CURVE ( 'NONE', #32261, #16885, #1374, .T. ) ;
#24661 = ADVANCED_FACE ( 'NONE', ( #7011 ), #4010, .F. ) ;
#24662 = ORIENTED_EDGE ( 'NONE', *, *, #30366, .F. ) ;
#24663 = ORIENTED_EDGE ( 'NONE', *, *, #33222, .F. ) ;
#24664 = VERTEX_POINT ( 'NONE', #1204 ) ;
#24665 = FACE_OUTER_BOUND ( 'NONE', #8748, .T. ) ;
#24666 = DIRECTION ( 'NONE',  ( 0.000000000000000000, 0.000000000000000000, 1.000000000000000000 ) ) ;
#24667 = EDGE_CURVE ( 'NONE', #12006, #20765, #24075, .T. ) ;
#24668 = ORIENTED_EDGE ( 'NONE', *, *, #1175, .F. ) ;
#24669 = LINE ( 'NONE', #19399, #10122 ) ;
#24670 = ADVANCED_FACE ( 'NONE', ( #27059 ), #33061, .F. ) ;
#24671 = CYLINDRICAL_SURFACE ( 'NONE', #20092, 2.000000000000001776 ) ;
#24672 = EDGE_LOOP ( 'NONE', ( #5083, #6549 ) ) ;
#24673 = CARTESIAN_POINT ( 'NONE',  ( 34.99999662536855283, -60.62177826491080168, -5.000000000000000000 ) ) ;
#24674 = ORIENTED_EDGE ( 'NONE', *, *, #32987, .F. ) ;
#24675 = CYLINDRICAL_SURFACE ( 'NONE', #13543, 2.000000000000001776 ) ;
#24676 = CARTESIAN_POINT ( 'NONE',  ( 47.99999662536846756, -69.28203230275519786, 17.49999999999999645 ) ) ;
#24677 = CARTESIAN_POINT ( 'NONE',  ( -7.000003374631269537, -77.94228634059960825, -9.999999999999998224 ) ) ;
#24678 = AXIS2_PLACEMENT_3D ( 'NONE', #19754, #33246, #2320 ) ;
#24679 = FACE_OUTER_BOUND ( 'NONE', #17095, .T. ) ;
#24680 = ADVANCED_FACE ( 'NONE', ( #12793 ), #16011, .F. ) ;
#24681 = ORIENTED_EDGE ( 'NONE', *, *, #89, .F. ) ;
#24682 = CYLINDRICAL_SURFACE ( 'NONE', #7512, 27.00000000000001421 ) ;
#24683 = SHAPE_DEFINITION_REPRESENTATION ( #31296, #35880 ) ;
#24684 = DIRECTION ( 'NONE',  ( 1.000000000000000000, 0.000000000000000000, 0.000000000000000000 ) ) ;
#24685 = DIRECTION ( 'NONE',  ( 1.000000000000000000, 0.000000000000000000, 0.000000000000000000 ) ) ;
#24686 = EDGE_LOOP ( 'NONE', ( #11089, #29928, #23827, #26321, #2872 ) ) ;
#24687 = CARTESIAN_POINT ( 'NONE',  ( 79.99999662536833966, 17.32050807568879236, -5.000000000000000000 ) ) ;
#24688 = CARTESIAN_POINT ( 'NONE',  ( 2.999996625368676728, -77.94228634059960825, -9.999999999999998224 ) ) ;
#24689 = EDGE_LOOP ( 'NONE', ( #29069, #36980, #29108, #10324 ) ) ;
#24690 = DIRECTION ( 'NONE',  ( 1.000000000000000000, 0.000000000000000000, 0.000000000000000000 ) ) ;
#24691 = CARTESIAN_POINT ( 'NONE',  ( 64.99999662536839651, 60.62177826491078747, -5.000000000000000000 ) ) ;
#24692 = DIRECTION ( 'NONE',  ( 0.000000000000000000, 0.000000000000000000, 1.000000000000000000 ) ) ;
#24693 = ORIENTED_EDGE ( 'NONE', *, *, #22464, .T. ) ;
#24694 = ADVANCED_FACE ( 'NONE', ( #24246 ), #12996, .F. ) ;
#24695 = ORIENTED_EDGE ( 'NONE', *, *, #20366, .T. ) ;
#24696 = DIRECTION ( 'NONE',  ( -0.000000000000000000, -0.000000000000000000, 1.000000000000000000 ) ) ;
#24697 = DIRECTION ( 'NONE',  ( 0.000000000000000000, 0.000000000000000000, -1.000000000000000000 ) ) ;
#24698 = DIRECTION ( 'NONE',  ( -0.000000000000000000, -0.000000000000000000, -1.000000000000000000 ) ) ;
#24699 = ORIENTED_EDGE ( 'NONE', *, *, #9083, .T. ) ;
#24700 = ORIENTED_EDGE ( 'NONE', *, *, #30580, .F. ) ;
#24701 = AXIS2_PLACEMENT_3D ( 'NONE', #3613, #12391, #23860 ) ;
#24702 = CARTESIAN_POINT ( 'NONE',  ( -45.00000337463112743, -60.62177826491080168, 12.50000000000000000 ) ) ;
#24703 = CARTESIAN_POINT ( 'NONE',  ( -0.3487148583350038744, 5.572172074566123179, -1.686035282245269995 ) ) ;
#24704 = EDGE_CURVE ( 'NONE', #26494, #25226, #24455, .T. ) ;
#24705 = DIRECTION ( 'NONE',  ( 0.000000000000000000, 0.000000000000000000, -1.000000000000000000 ) ) ;
#24706 = CARTESIAN_POINT ( 'NONE',  ( -95.78743416778654307, 68.56885790715003282, 32.50000000000000000 ) ) ;
#24707 = ORIENTED_EDGE ( 'NONE', *, *, #20552, .F. ) ;
#24708 = ORIENTED_EDGE ( 'NONE', *, *, #36539, .T. ) ;
#24709 = CARTESIAN_POINT ( 'NONE',  ( -32.16008401677955675, -61.25926521283091830, -4.999999999999997335 ) ) ;
#24710 = ADVANCED_FACE ( 'NONE', ( #27236 ), #1558, .F. ) ;
#24711 = CARTESIAN_POINT ( 'NONE',  ( 0.000000000000000000, 0.000000000000000000, -5.674599999999998090 ) ) ;
#24712 = ORIENTED_EDGE ( 'NONE', *, *, #15512, .T. ) ;
#24713 = CARTESIAN_POINT ( 'NONE',  ( 69.99999662536841072, 51.96152422706640550, 12.50000000000000000 ) ) ;
#24714 = EDGE_LOOP ( 'NONE', ( #34486, #3037, #34943, #35511 ) ) ;
#24715 = LINE ( 'NONE', #7097, #24312 ) ;
#24716 = AXIS2_PLACEMENT_3D ( 'NONE', #12774, #9790, #15990 ) ;
#24717 = DIRECTION ( 'NONE',  ( 0.000000000000000000, 0.000000000000000000, 1.000000000000000000 ) ) ;
#24718 = ORIENTED_EDGE ( 'NONE', *, *, #14403, .F. ) ;
#24719 = DIRECTION ( 'NONE',  ( 1.000000000000000000, 0.000000000000000000, 0.000000000000000000 ) ) ;
#24720 = VERTEX_POINT ( 'NONE', #30439 ) ;
#24721 = SURFACE_STYLE_USAGE ( .BOTH. , #16286 ) ;
#24722 = CARTESIAN_POINT ( 'NONE',  ( -3.567687560464436025, 3.713697318477624520, -0.1121614189353325186 ) ) ;
#24723 = EDGE_CURVE ( 'NONE', #20815, #7230, #33517, .T. ) ;
#24724 = CIRCLE ( 'NONE', #33692, 2.000000000000000000 ) ;
#24725 = CYLINDRICAL_SURFACE ( 'NONE', #24547, 2.000000000000001776 ) ;
#24726 = DIRECTION ( 'NONE',  ( 0.000000000000000000, 0.000000000000000000, 1.000000000000000000 ) ) ;
#24727 = ORIENTED_EDGE ( 'NONE', *, *, #8002, .T. ) ;
#24728 = AXIS2_PLACEMENT_3D ( 'NONE', #36647, #7781, #13378 ) ;
#24729 = CARTESIAN_POINT ( 'NONE',  ( 86.99999662536832545, 25.98076211353319565, 17.49999999999999645 ) ) ;
#24730 = LINE ( 'NONE', #24558, #35787 ) ;
#24731 = DIRECTION ( 'NONE',  ( 0.000000000000000000, 0.000000000000000000, 1.000000000000000000 ) ) ;
#24732 = ORIENTED_EDGE ( 'NONE', *, *, #31220, .T. ) ;
#24733 = EDGE_CURVE ( 'NONE', #26481, #36697, #5969, .T. ) ;
#24734 = ORIENTED_EDGE ( 'NONE', *, *, #19958, .T. ) ;
#24735 = EDGE_LOOP ( 'NONE', ( #19631, #480, #12903, #18534 ) ) ;
#24736 = ADVANCED_FACE ( 'NONE', ( #13359 ), #36996, .F. ) ;
#24737 = CARTESIAN_POINT ( 'NONE',  ( 64.99999662536839651, -43.30127018922199511, 17.49999999999999645 ) ) ;
#24738 = ORIENTED_EDGE ( 'NONE', *, *, #14200, .T. ) ;
#24739 = CYLINDRICAL_SURFACE ( 'NONE', #9128, 65.00000000000000000 ) ;
#24740 = DIRECTION ( 'NONE',  ( 0.000000000000000000, 0.000000000000000000, -1.000000000000000000 ) ) ;
#24741 = VECTOR ( 'NONE', #13684, 1000.000000000000000 ) ;
#24742 = CARTESIAN_POINT ( 'NONE',  ( 33.21453428580180400, -78.84346569788027637, -5.000000000000000000 ) ) ;
#24743 = DIRECTION ( 'NONE',  ( 0.000000000000000000, 0.000000000000000000, -1.000000000000000000 ) ) ;
#24744 = CARTESIAN_POINT ( 'NONE',  ( 6.249999999999998224, 0.000000000000000000, -3.250000000000001332 ) ) ;
#24745 = DIRECTION ( 'NONE',  ( 0.000000000000000000, 0.000000000000000000, 1.000000000000000000 ) ) ;
#24746 = DIRECTION ( 'NONE',  ( 0.000000000000000000, 0.000000000000000000, 1.000000000000000000 ) ) ;
#24747 = LINE ( 'NONE', #1486, #4701 ) ;
#24748 = ORIENTED_EDGE ( 'NONE', *, *, #27891, .F. ) ;
#24749 = ORIENTED_EDGE ( 'NONE', *, *, #30749, .T. ) ;
#24750 = CARTESIAN_POINT ( 'NONE',  ( 6.000000000000000000, 0.000000000000000000, 0.000000000000000000 ) ) ;
#24751 = EDGE_CURVE ( 'NONE', #8894, #26711, #8489, .T. ) ;
#24752 = FACE_OUTER_BOUND ( 'NONE', #2397, .T. ) ;
#24753 = DIRECTION ( 'NONE',  ( 0.000000000000000000, 0.000000000000000000, -1.000000000000000000 ) ) ;
#24754 = CARTESIAN_POINT ( 'NONE',  ( 36.99999662536855283, -77.94228634059960825, -9.999999999999998224 ) ) ;
#24755 = VERTEX_POINT ( 'NONE', #16758 ) ;
#24756 = DIRECTION ( 'NONE',  ( 0.000000000000000000, 0.000000000000000000, 1.000000000000000000 ) ) ;
#24757 = CARTESIAN_POINT ( 'NONE',  ( 5.000000000000000000, -0.5603747650654238299, -0.5678343202077608121 ) ) ;
#24758 = ORIENTED_EDGE ( 'NONE', *, *, #24053, .T. ) ;
#24759 =( REPRESENTATION_RELATIONSHIP ('NONE','NONE', #15268, #35440 ) REPRESENTATION_RELATIONSHIP_WITH_TRANSFORMATION ( #27288 )SHAPE_REPRESENTATION_RELATIONSHIP( ) );
#24760 = DIRECTION ( 'NONE',  ( 0.000000000000000000, 0.000000000000000000, 1.000000000000000000 ) ) ;
#24761 = CIRCLE ( 'NONE', #8584, 2.000000000000001776 ) ;
#24762 = ORIENTED_EDGE ( 'NONE', *, *, #25711, .F. ) ;
#24763 = PRESENTATION_STYLE_ASSIGNMENT (( #33587 ) ) ;
#24764 = CARTESIAN_POINT ( 'NONE',  ( -35.00000337463116296, 77.94228634059957983, -9.999999999999998224 ) ) ;
#24765 = CIRCLE ( 'NONE', #3205, 3.000000000000007105 ) ;
#24766 = DIRECTION ( 'NONE',  ( 0.000000000000000000, 0.000000000000000000, 1.000000000000000000 ) ) ;
#24767 = EDGE_CURVE ( 'NONE', #15438, #8840, #13918, .T. ) ;
#24768 = CARTESIAN_POINT ( 'NONE',  ( -5.000003374631269537, -77.94228634059960825, -5.000000000000000000 ) ) ;
#24769 = ORIENTED_EDGE ( 'NONE', *, *, #27978, .F. ) ;
#24770 = EDGE_CURVE ( 'NONE', #698, #24284, #32281, .T. ) ;
#24771 = ORIENTED_EDGE ( 'NONE', *, *, #6174, .F. ) ;
#24772 = AXIS2_PLACEMENT_3D ( 'NONE', #7245, #12841, #15862 ) ;
#24773 = ADVANCED_FACE ( 'NONE', ( #2111 ), #22192, .F. ) ;
#24774 = ORIENTED_EDGE ( 'NONE', *, *, #33875, .T. ) ;
#24775 = CARTESIAN_POINT ( 'NONE',  ( 3.000000000000000000, 2.935248768560057453, -3.903127820947815962E-15 ) ) ;
#24776 = VECTOR ( 'NONE', #9220, 1000.000000000000000 ) ;
#24777 = DIRECTION ( 'NONE',  ( -0.000000000000000000, -0.000000000000000000, -1.000000000000000000 ) ) ;
#24778 = ADVANCED_FACE ( 'NONE', ( #30618 ), #31342, .T. ) ;
#24779 = DIRECTION ( 'NONE',  ( 0.000000000000000000, 0.000000000000000000, 1.000000000000000000 ) ) ;
#24780 = DIRECTION ( 'NONE',  ( 1.000000000000000000, 0.000000000000000000, 0.000000000000000000 ) ) ;
#24781 = CARTESIAN_POINT ( 'NONE',  ( -72.00000337463100664, 34.64101615137758472, -9.999999999999998224 ) ) ;
#24782 = ADVANCED_FACE ( 'NONE', ( #25365 ), #27621, .F. ) ;
#24783 = ORIENTED_EDGE ( 'NONE', *, *, #32837, .F. ) ;
#24784 = DIRECTION ( 'NONE',  ( 0.000000000000000000, 0.000000000000000000, 1.000000000000000000 ) ) ;
#24785 = PRODUCT_DEFINITION_SHAPE ( 'NONE', 'NONE',  #37122 ) ;
#24786 = CARTESIAN_POINT ( 'NONE',  ( 69.99999662536839651, -3.469446951953614189E-15, -5.000000000000000000 ) ) ;
#24787 = CARTESIAN_POINT ( 'NONE',  ( 19.99999662536861678, -69.28203230275519786, -9.999999999999998224 ) ) ;
#24788 = ORIENTED_EDGE ( 'NONE', *, *, #36465, .T. ) ;
#24789 = DIRECTION ( 'NONE',  ( 1.000000000000000000, 0.000000000000000000, 0.000000000000000000 ) ) ;
#24790 = DIRECTION ( 'NONE',  ( 0.000000000000000000, 0.000000000000000000, 1.000000000000000000 ) ) ;
#24791 = EDGE_CURVE ( 'NONE', #7889, #27142, #7761, .T. ) ;
#24792 = ORIENTED_EDGE ( 'NONE', *, *, #33421, .F. ) ;
#24793 = EDGE_CURVE ( 'NONE', #25244, #5952, #2970, .T. ) ;
#24794 = AXIS2_PLACEMENT_3D ( 'NONE', #10824, #31411, #11176 ) ;
#24795 = VERTEX_POINT ( 'NONE', #33446 ) ;
#24796 = EDGE_CURVE ( 'NONE', #27057, #21230, #13136, .T. ) ;
#24797 = EDGE_CURVE ( 'NONE', #15477, #32385, #34689, .T. ) ;
#24798 = DIRECTION ( 'NONE',  ( 0.000000000000000000, 0.000000000000000000, -1.000000000000000000 ) ) ;
#24799 = CARTESIAN_POINT ( 'NONE',  ( 1.598077599633028090, -4.850852159562031751, -3.971474537231029611 ) ) ;
#24800 = EDGE_CURVE ( 'NONE', #17212, #4310, #16561, .T. ) ;
#24801 = CARTESIAN_POINT ( 'NONE',  ( 62.99999662536839651, 60.62177826491078747, -9.999999999999998224 ) ) ;
#24802 = ORIENTED_EDGE ( 'NONE', *, *, #29357, .T. ) ;
#24803 = VERTEX_POINT ( 'NONE', #36627 ) ;
#24804 = ORIENTED_EDGE ( 'NONE', *, *, #23838, .T. ) ;
#24805 = AXIS2_PLACEMENT_3D ( 'NONE', #13145, #19157, #7510 ) ;
#24806 = CARTESIAN_POINT ( 'NONE',  ( 67.99999662536836809, -51.96152422706639840, -9.999999999999998224 ) ) ;
#24807 = PRESENTATION_LAYER_ASSIGNMENT (  '', '', ( #28373 ) ) ;
#24808 = ORIENTED_EDGE ( 'NONE', *, *, #29809, .F. ) ;
#24809 = FACE_BOUND ( 'NONE', #6727, .T. ) ;
#24810 = EDGE_LOOP ( 'NONE', ( #27191, #32912, #22478, #36587 ) ) ;
#24811 = ORIENTED_EDGE ( 'NONE', *, *, #3496, .T. ) ;
#24812 = DIRECTION ( 'NONE',  ( 1.000000000000000000, 0.000000000000000000, 0.000000000000000000 ) ) ;
#24813 = B_SPLINE_CURVE_WITH_KNOTS ( 'NONE', 3,
 ( #33327, #7838, #27126, #19093, #21522, #30522, #4840, #19267, #36139, #4276, #16269, #1831, #24889, #12870, #36331, #24140, #9886, #24706, #32765, #35972, #4451, #27686, #24331, #10641, #32959, #4649, #7271, #12685 ),
 .UNSPECIFIED., .F., .F.,
 ( 4, 2, 2, 1, 1, 2, 2, 1, 2, 2, 1, 1, 2, 2, 1, 2, 4 ),
 ( 0.1667295141962928384, 0.1840819284725213056, 0.1927581356106355948, 0.2014343427487499116, 0.2361391713012070959, 0.2448153784393213295, 0.2534915855774355076, 0.2708439998536639748, 0.3055488284061209647, 0.3142250355442351983, 0.3229012426823494319, 0.3402536569585778992, 0.3749584855110348336, 0.4096633140634917125, 0.4270157283397201242, 0.4356919354778343578, 0.4443681426159485914 ),
 .UNSPECIFIED. ) ;
#24814 = LINE ( 'NONE', #18815, #7502 ) ;
#24815 = ORIENTED_EDGE ( 'NONE', *, *, #2676, .F. ) ;
#24816 = EDGE_LOOP ( 'NONE', ( #15094, #35508, #21839 ) ) ;
#24817 = DIRECTION ( 'NONE',  ( -1.000000000000000000, 0.000000000000000000, 0.000000000000000000 ) ) ;
#24818 = DIRECTION ( 'NONE',  ( 0.000000000000000000, 0.000000000000000000, 1.000000000000000000 ) ) ;
#24819 = DIRECTION ( 'NONE',  ( -1.000000000000000000, 0.000000000000000000, -0.000000000000000000 ) ) ;
#24820 = CYLINDRICAL_SURFACE ( 'NONE', #7713, 2.000000000000000000 ) ;
#24821 = AXIS2_PLACEMENT_3D ( 'NONE', #22990, #8734, #12078 ) ;
#24822 = EDGE_LOOP ( 'NONE', ( #18506, #713, #23327 ) ) ;
#24823 = DIRECTION ( 'NONE',  ( 0.000000000000000000, 0.000000000000000000, 1.000000000000000000 ) ) ;
#24824 = FACE_BOUND ( 'NONE', #13989, .T. ) ;
#24825 = LINE ( 'NONE', #36806, #23199 ) ;
#24826 = FACE_BOUND ( 'NONE', #20556, .T. ) ;
#24827 = CARTESIAN_POINT ( 'NONE',  ( -42.97377950131527058, 96.90768712682508124, -11.00000000000000000 ) ) ;
#24828 = CARTESIAN_POINT ( 'NONE',  ( -65.00000337463104927, -25.98076211353322051, -9.999999999999998224 ) ) ;
#24829 = CIRCLE ( 'NONE', #8644, 2.000000000000001776 ) ;
#24830 = VECTOR ( 'NONE', #23424, 1000.000000000000000 ) ;
#24831 = PLANE ( 'NONE',  #14406 ) ;
#24832 = CIRCLE ( 'NONE', #2061, 2.000000000000001776 ) ;
#24833 = CARTESIAN_POINT ( 'NONE',  ( -17.14523346298280160, 93.36492675454785228, -4.999999999999997335 ) ) ;
#24834 = EDGE_LOOP ( 'NONE', ( #34816, #677, #28246, #9531 ) ) ;
#24835 = CARTESIAN_POINT ( 'NONE',  ( 57.99999662536842493, 51.96152422706639129, -9.999999999999998224 ) ) ;
#24836 = CARTESIAN_POINT ( 'NONE',  ( 5.000000000000000000, 2.886751345948125991, -6.000000000000000000 ) ) ;
#24837 = DIRECTION ( 'NONE',  ( -1.000000000000000000, 0.000000000000000000, 0.000000000000000000 ) ) ;
#24838 = EDGE_LOOP ( 'NONE', ( #17183, #1009 ) ) ;
#24839 = ORIENTED_EDGE ( 'NONE', *, *, #36064, .F. ) ;
#24840 = VERTEX_POINT ( 'NONE', #22549 ) ;
#24841 = AXIS2_PLACEMENT_3D ( 'NONE', #20603, #34880, #34708 ) ;
#24842 = ADVANCED_FACE ( 'NONE', ( #2316 ), #22361, .F. ) ;
#24843 = CARTESIAN_POINT ( 'NONE',  ( -70.00000337463099243, 34.64101615137758472, -9.999999999999998224 ) ) ;
#24844 = CARTESIAN_POINT ( 'NONE',  ( -43.00000337463111322, 60.62177826491077326, -9.999999999999998224 ) ) ;
#24845 = AXIS2_PLACEMENT_3D ( 'NONE', #29984, #32986, #13112 ) ;
#24846 = ORIENTED_EDGE ( 'NONE', *, *, #15362, .T. ) ;
#24847 = CIRCLE ( 'NONE', #21240, 2.000000000000001776 ) ;
#24848 = FACE_OUTER_BOUND ( 'NONE', #7213, .T. ) ;
#24849 = CARTESIAN_POINT ( 'NONE',  ( 49.99999662536846756, 69.28203230275516944, -9.999999999999998224 ) ) ;
#24850 = VERTEX_POINT ( 'NONE', #8116 ) ;
#24851 = DIRECTION ( 'NONE',  ( 1.000000000000000000, 0.000000000000000000, 0.000000000000000000 ) ) ;
#24852 = EDGE_LOOP ( 'NONE', ( #27852, #32013 ) ) ;
#24853 = FACE_BOUND ( 'NONE', #6759, .T. ) ;
#24854 = CIRCLE ( 'NONE', #28444, 2.000000000000001776 ) ;
#24855 = AXIS2_PLACEMENT_3D ( 'NONE', #5063, #16499, #27933 ) ;
#24856 = VECTOR ( 'NONE', #2948, 1000.000000000000000 ) ;
#24857 = CARTESIAN_POINT ( 'NONE',  ( -2.074714256722481664, 4.575665857285980742, -5.989444439476608650 ) ) ;
#24858 = CARTESIAN_POINT ( 'NONE',  ( 1.738521435313294727, -5.045405839192998343, -4.085926550512748001 ) ) ;
#24859 = DIRECTION ( 'NONE',  ( -1.000000000000000000, -0.000000000000000000, -0.000000000000000000 ) ) ;
#24860 = ORIENTED_EDGE ( 'NONE', *, *, #19735, .T. ) ;
#24861 = CARTESIAN_POINT ( 'NONE',  ( 76.99999662536835388, -43.30127018922199511, -9.999999999999998224 ) ) ;
#24862 = CONTEXT_DEPENDENT_SHAPE_REPRESENTATION ( #7292, #22101 ) ;
#24863 = EDGE_CURVE ( 'NONE', #8511, #6351, #10757, .T. ) ;
#24864 = CARTESIAN_POINT ( 'NONE',  ( 56.67878100130369035, -27.78182860042797131, 12.49999999999999822 ) ) ;
#24865 = DIRECTION ( 'NONE',  ( 1.000000000000000000, 0.000000000000000000, 0.000000000000000000 ) ) ;
#24866 = AXIS2_PLACEMENT_3D ( 'NONE', #30163, #27161, #9567 ) ;
#24867 = ORIENTED_EDGE ( 'NONE', *, *, #28554, .F. ) ;
#24868 = DIRECTION ( 'NONE',  ( 0.000000000000000000, 0.000000000000000000, 1.000000000000000000 ) ) ;
#24869 = CARTESIAN_POINT ( 'NONE',  ( -45.00000337463111322, 60.62177826491077326, -9.999999999999998224 ) ) ;
#24870 = ORIENTED_EDGE ( 'NONE', *, *, #12341, .T. ) ;
#24871 = CARTESIAN_POINT ( 'NONE',  ( 82.27241335952179213, 47.49999999999982236, 32.50002500000000083 ) ) ;
#24872 = CIRCLE ( 'NONE', #16480, 3.000000000000000888 ) ;
#24873 = CARTESIAN_POINT ( 'NONE',  ( -2.374207310413330682E-13, -68.00000000000000000, 12.49999999999999822 ) ) ;
#24874 = DIRECTION ( 'NONE',  ( -1.000000000000000000, 0.000000000000000000, -0.000000000000000000 ) ) ;
#24875 = AXIS2_PLACEMENT_3D ( 'NONE', #34812, #25822, #5947 ) ;
#24876 = ORIENTED_EDGE ( 'NONE', *, *, #5679, .F. ) ;
#24877 = ORIENTED_EDGE ( 'NONE', *, *, #11475, .F. ) ;
#24878 = DIRECTION ( 'NONE',  ( 0.4999999999999919509, -0.8660254037844432595, 0.000000000000000000 ) ) ;
#24879 = CARTESIAN_POINT ( 'NONE',  ( 79.99999662536832545, -17.32050807568879591, -9.999999999999998224 ) ) ;
#24880 = AXIS2_PLACEMENT_3D ( 'NONE', #33715, #25279, #14003 ) ;
#24881 = CIRCLE ( 'NONE', #29619, 8.500000000000007105 ) ;
#24882 = LINE ( 'NONE', #33317, #24908 ) ;
#24883 = ORIENTED_EDGE ( 'NONE', *, *, #6316, .F. ) ;
#24884 = ORIENTED_EDGE ( 'NONE', *, *, #14938, .F. ) ;
#24885 = EDGE_CURVE ( 'NONE', #33342, #22150, #30990, .T. ) ;
#24886 = CARTESIAN_POINT ( 'NONE',  ( 4.999999999999997335, 0.000000000000000000, 0.000000000000000000 ) ) ;
#24887 = CARTESIAN_POINT ( 'NONE',  ( 76.99999662536835388, -43.30127018922199511, 17.49999999999999645 ) ) ;
#24888 = DIRECTION ( 'NONE',  ( -0.000000000000000000, -0.000000000000000000, -1.000000000000000000 ) ) ;
#24889 = CARTESIAN_POINT ( 'NONE',  ( -101.6272589138252442, 63.51387141301889727, 32.49999999999999289 ) ) ;
#24890 = ORIENTED_EDGE ( 'NONE', *, *, #7890, .F. ) ;
#24891 = VERTEX_POINT ( 'NONE', #35043 ) ;
#24892 = LINE ( 'NONE', #35596, #4528 ) ;
#24893 = VECTOR ( 'NONE', #31384, 1000.000000000000000 ) ;
#24894 = CARTESIAN_POINT ( 'NONE',  ( -65.00000337463102085, 60.62177826491077326, 17.49999999999999645 ) ) ;
#24895 = ORIENTED_EDGE ( 'NONE', *, *, #14932, .T. ) ;
#24896 = CIRCLE ( 'NONE', #15298, 2.000000000000001776 ) ;
#24897 = CYLINDRICAL_SURFACE ( 'NONE', #23317, 2.000000000000001776 ) ;
#24898 = ORIENTED_EDGE ( 'NONE', *, *, #36244, .F. ) ;
#24899 = FACE_OUTER_BOUND ( 'NONE', #27295, .T. ) ;
#24900 = CIRCLE ( 'NONE', #8720, 2.000000000000001776 ) ;
#24901 = CIRCLE ( 'NONE', #29663, 1.999999999999998224 ) ;
#24902 = CIRCLE ( 'NONE', #23092, 3.000000000000002665 ) ;
#24903 = LINE ( 'NONE', #8013, #22705 ) ;
#24904 = ADVANCED_FACE ( 'NONE', ( #14304 ), #723, .F. ) ;
#24905 = DIRECTION ( 'NONE',  ( 0.000000000000000000, 0.000000000000000000, 1.000000000000000000 ) ) ;
#24906 = ORIENTED_EDGE ( 'NONE', *, *, #33042, .F. ) ;
#24907 = EDGE_CURVE ( 'NONE', #8706, #34583, #6547, .T. ) ;
#24908 = VECTOR ( 'NONE', #7440, 1000.000000000000000 ) ;
#24909 = DIRECTION ( 'NONE',  ( -0.000000000000000000, -0.000000000000000000, 1.000000000000000000 ) ) ;
#24910 = CARTESIAN_POINT ( 'NONE',  ( 74.99999662536836809, -8.660254037844401509, 12.50000000000000000 ) ) ;
#24911 = DIRECTION ( 'NONE',  ( 1.000000000000000000, 0.000000000000000000, 0.000000000000000000 ) ) ;
#24912 = VERTEX_POINT ( 'NONE', #18155 ) ;
#24913 = CARTESIAN_POINT ( 'NONE',  ( 61.99999662536842493, -51.96152422706639840, -9.999999999999998224 ) ) ;
#24914 = EDGE_CURVE ( 'NONE', #32504, #9552, #21510, .T. ) ;
#24915 = CARTESIAN_POINT ( 'NONE',  ( -60.00000337463104216, 34.64101615137757051, -5.000000000000000000 ) ) ;
#24916 = DIRECTION ( 'NONE',  ( 1.000000000000000000, 0.000000000000000000, 0.000000000000000000 ) ) ;
#24917 = ORIENTED_EDGE ( 'NONE', *, *, #30070, .T. ) ;
#24918 = AXIS2_PLACEMENT_3D ( 'NONE', #4388, #9817, #24080 ) ;
#24919 = ORIENTED_EDGE ( 'NONE', *, *, #19595, .F. ) ;
#24920 = ADVANCED_FACE ( 'NONE', ( #26975 ), #29579, .F. ) ;
#24921 = VERTEX_POINT ( 'NONE', #6348 ) ;
#24922 = FACE_OUTER_BOUND ( 'NONE', #30868, .T. ) ;
#24923 = ORIENTED_EDGE ( 'NONE', *, *, #13716, .T. ) ;
#24924 = AXIS2_PLACEMENT_3D ( 'NONE', #11070, #11268, #19525 ) ;
#24925 = PRESENTATION_LAYER_ASSIGNMENT (  '', '', ( #3949 ) ) ;
#24926 = CARTESIAN_POINT ( 'NONE',  ( -5.000000000000000000, -1.472375319565265794, -0.9369361380397573935 ) ) ;
#24927 = CARTESIAN_POINT ( 'NONE',  ( -77.00000337463097821, 25.98076211353318854, 12.50000000000000000 ) ) ;
#24928 = AXIS2_PLACEMENT_3D ( 'NONE', #33008, #24756, #7323 ) ;
#24929 = CIRCLE ( 'NONE', #23746, 2.000000000000000000 ) ;
#24930 = CIRCLE ( 'NONE', #9953, 3.250000000000001332 ) ;
#24931 = DIRECTION ( 'NONE',  ( 0.000000000000000000, 0.000000000000000000, 1.000000000000000000 ) ) ;
#24932 = VECTOR ( 'NONE', #33356, 1000.000000000000000 ) ;
#24933 = LINE ( 'NONE', #12919, #10444 ) ;
#24934 = DIRECTION ( 'NONE',  ( 1.000000000000000000, 0.000000000000000000, 0.000000000000000000 ) ) ;
#24935 = CARTESIAN_POINT ( 'NONE',  ( -18.00000337463124467, 69.28203230275516944, 12.50000000000000000 ) ) ;
#24936 = CARTESIAN_POINT ( 'NONE',  ( -37.50000000000000000, -103.4105893997321743, 32.50000000000000000 ) ) ;
#24937 = CARTESIAN_POINT ( 'NONE',  ( 81.99999662536833966, -3.469446951953614189E-15, -9.999999999999998224 ) ) ;
#24938 = VERTEX_POINT ( 'NONE', #21156 ) ;
#24939 = CIRCLE ( 'NONE', #26098, 2.000000000000001776 ) ;
#24940 = ORIENTED_EDGE ( 'NONE', *, *, #3763, .F. ) ;
#24941 = ADVANCED_FACE ( 'NONE', ( #3907 ), #12135, .F. ) ;
#24942 = CARTESIAN_POINT ( 'NONE',  ( -8.000003374631278419, -69.28203230275519786, -9.999999999999998224 ) ) ;
#24943 = DIRECTION ( 'NONE',  ( 0.4999999999999922839, -0.8660254037844431485, 0.000000000000000000 ) ) ;
#24944 = CARTESIAN_POINT ( 'NONE',  ( -53.00000337463109190, -60.62177826491083010, 17.49999999999999645 ) ) ;
#24945 = DIRECTION ( 'NONE',  ( -0.5000000000000101030, -0.8660254037844329345, 0.000000000000000000 ) ) ;
#24946 = ORIENTED_EDGE ( 'NONE', *, *, #17656, .T. ) ;
#24947 = UNCERTAINTY_MEASURE_WITH_UNIT (LENGTH_MEASURE( 1.000000000000000082E-05 ), #19503, 'distance_accuracy_value', 'NONE');
#24948 = AXIS2_PLACEMENT_3D ( 'NONE', #52, #7767, #16927 ) ;
#24949 = EDGE_CURVE ( 'NONE', #33082, #16790, #19816, .T. ) ;
#24950 = CARTESIAN_POINT ( 'NONE',  ( -73.00000337463100664, -43.30127018922202353, -9.999999999999998224 ) ) ;
#24951 = AXIS2_PLACEMENT_3D ( 'NONE', #29242, #35060, #15176 ) ;
#24952 = CARTESIAN_POINT ( 'NONE',  ( 56.99999662536844625, 60.62177826491077326, 12.50000000000000000 ) ) ;
#24953 = ORIENTED_EDGE ( 'NONE', *, *, #17386, .T. ) ;
#24954 = EDGE_CURVE ( 'NONE', #7561, #10165, #30507, .T. ) ;
#24955 = PRESENTATION_LAYER_ASSIGNMENT (  '', '', ( #33323 ) ) ;
#24956 = CYLINDRICAL_SURFACE ( 'NONE', #33215, 2.000000000000001776 ) ;
#24957 = EDGE_LOOP ( 'NONE', ( #33987, #34298 ) ) ;
#24958 = CIRCLE ( 'NONE', #8772, 2.000000000000001776 ) ;
#24959 = AXIS2_PLACEMENT_3D ( 'NONE', #12997, #30059, #1205 ) ;
#24960 = AXIS2_PLACEMENT_3D ( 'NONE', #16260, #35765, #1990 ) ;
#24961 = DIRECTION ( 'NONE',  ( 1.000000000000000000, 0.000000000000000000, 0.000000000000000000 ) ) ;
#24962 = AXIS2_PLACEMENT_3D ( 'NONE', #6063, #32293, #20860 ) ;
#24963 = DIRECTION ( 'NONE',  ( 0.4999999999999919509, -0.8660254037844432595, 0.000000000000000000 ) ) ;
#24964 = AXIS2_PLACEMENT_3D ( 'NONE', #1818, #10974, #35956 ) ;
#24965 = CARTESIAN_POINT ( 'NONE',  ( -58.88972745734155723, 34.00000000000049027, 12.49999999999999822 ) ) ;
#24966 = ORIENTED_EDGE ( 'NONE', *, *, #23758, .T. ) ;
#24967 = EDGE_LOOP ( 'NONE', ( #29040, #21151, #6928, #21437 ) ) ;
#24968 = AXIS2_PLACEMENT_3D ( 'NONE', #14139, #33664, #7968 ) ;
#24969 = EDGE_CURVE ( 'NONE', #875, #8614, #9723, .T. ) ;
#24970 = ORIENTED_EDGE ( 'NONE', *, *, #29264, .F. ) ;
#24971 = CARTESIAN_POINT ( 'NONE',  ( 66.99999662536842493, 43.30127018922200222, 12.50000000000000000 ) ) ;
#24972 = CARTESIAN_POINT ( 'NONE',  ( 77.99999662536832545, -17.32050807568879591, -9.999999999999998224 ) ) ;
#24973 = CARTESIAN_POINT ( 'NONE',  ( -33.00000337463116296, -60.62177826491080168, -9.999999999999998224 ) ) ;
#24974 = CARTESIAN_POINT ( 'NONE',  ( -4.999999999999999112, 1.924500897298729196, -3.818275046351159219 ) ) ;
#24975 = CARTESIAN_POINT ( 'NONE',  ( -145.0000000000000568, 1.518182058997189877E-12, 27.50000000000000000 ) ) ;
#24976 = ORIENTED_EDGE ( 'NONE', *, *, #21115, .F. ) ;
#24977 = LINE ( 'NONE', #10892, #17127 ) ;
#24978 = FACE_OUTER_BOUND ( 'NONE', #24434, .T. ) ;
#24979 = AXIS2_PLACEMENT_3D ( 'NONE', #18572, #29989, #1475 ) ;
#24980 = DIRECTION ( 'NONE',  ( 0.000000000000000000, 0.000000000000000000, -1.000000000000000000 ) ) ;
#24981 = ORIENTED_EDGE ( 'NONE', *, *, #30013, .T. ) ;
#24982 = DIRECTION ( 'NONE',  ( 1.000000000000000000, 0.000000000000000000, 0.000000000000000000 ) ) ;
#24983 = FACE_OUTER_BOUND ( 'NONE', #17920, .T. ) ;
#24984 = ORIENTED_EDGE ( 'NONE', *, *, #29576, .T. ) ;
#24985 = VECTOR ( 'NONE', #7312, 1000.000000000000000 ) ;
#24986 = VERTEX_POINT ( 'NONE', #23800 ) ;
#24987 = AXIS2_PLACEMENT_3D ( 'NONE', #10018, #32336, #6654 ) ;
#24988 = EDGE_CURVE ( 'NONE', #27017, #10608, #31692, .T. ) ;
#24989 = FACE_OUTER_BOUND ( 'NONE', #18481, .T. ) ;
#24990 = CARTESIAN_POINT ( 'NONE',  ( 2.999996625368645198, 77.94228634059957983, -9.999999999999998224 ) ) ;
#24991 = CARTESIAN_POINT ( 'NONE',  ( 4.400655246572464208, -3.515428273943662862, -4.176900509771739323 ) ) ;
#24992 = ADVANCED_FACE ( 'NONE', ( #17791 ), #12705, .F. ) ;
#24993 = CARTESIAN_POINT ( 'NONE',  ( -2.618768541235303005, -4.261555969668739507, -0.5078976954042990766 ) ) ;
#24994 = ORIENTED_EDGE ( 'NONE', *, *, #15585, .F. ) ;
#24995 = ORIENTED_EDGE ( 'NONE', *, *, #6887, .F. ) ;
#24996 = AXIS2_PLACEMENT_3D ( 'NONE', #4759, #21438, #27430 ) ;
#24997 = EDGE_CURVE ( 'NONE', #29968, #9610, #36486, .T. ) ;
#24998 = DIRECTION ( 'NONE',  ( -1.000000000000000000, 0.000000000000000000, 0.000000000000000000 ) ) ;
#24999 = VERTEX_POINT ( 'NONE', #25753 ) ;
#25000 = EDGE_CURVE ( 'NONE', #32624, #30112, #17341, .T. ) ;
#25001 = EDGE_CURVE ( 'NONE', #28672, #32425, #3556, .T. ) ;
#25002 = PLANE ( 'NONE',  #11789 ) ;
#25003 = ORIENTED_EDGE ( 'NONE', *, *, #34211, .T. ) ;
#25004 = ADVANCED_FACE ( 'NONE', ( #3729 ), #26594, .F. ) ;
#25005 = CIRCLE ( 'NONE', #36378, 27.00000000000000711 ) ;
#25006 = VERTEX_POINT ( 'NONE', #1849 ) ;
#25007 = DIRECTION ( 'NONE',  ( 0.000000000000000000, 0.000000000000000000, -1.000000000000000000 ) ) ;
#25008 = VECTOR ( 'NONE', #7950, 1000.000000000000000 ) ;
#25009 = DIRECTION ( 'NONE',  ( -0.000000000000000000, -0.000000000000000000, 1.000000000000000000 ) ) ;
#25010 = VERTEX_POINT ( 'NONE', #18556 ) ;
#25011 = EDGE_LOOP ( 'NONE', ( #10558, #9720 ) ) ;
#25012 = CARTESIAN_POINT ( 'NONE',  ( -70.80619744049063513, -84.18124734178186941, 27.50000000000000000 ) ) ;
#25013 = CARTESIAN_POINT ( 'NONE',  ( 73.90204319670435495, -6.988578749851858340, 12.50000000000000000 ) ) ;
#25014 = ADVANCED_FACE ( 'NONE', ( #21714 ), #10113, .F. ) ;
#25015 = AXIS2_PLACEMENT_3D ( 'NONE', #34232, #33846, #19602 ) ;
#25016 = VECTOR ( 'NONE', #8970, 1000.000000000000000 ) ;
#25017 = CARTESIAN_POINT ( 'NONE',  ( 9.999996625368618552, 69.28203230275516944, 12.50000000000000000 ) ) ;
#25018 = ADVANCED_FACE ( 'NONE', ( #35802 ), #16289, .F. ) ;
#25019 = DIRECTION ( 'NONE',  ( 0.000000000000000000, 0.000000000000000000, 1.000000000000000000 ) ) ;
#25020 = VECTOR ( 'NONE', #3262, 1000.000000000000000 ) ;
#25021 = EDGE_CURVE ( 'NONE', #2623, #22366, #16730, .T. ) ;
#25022 = EDGE_LOOP ( 'NONE', ( #33867, #21536 ) ) ;
#25023 = DIRECTION ( 'NONE',  ( 1.000000000000000000, 0.000000000000000000, 0.000000000000000000 ) ) ;
#25024 = DIRECTION ( 'NONE',  ( 1.000000000000000000, 0.000000000000000000, 0.000000000000000000 ) ) ;
#25025 = DIRECTION ( 'NONE',  ( -0.000000000000000000, -0.000000000000000000, -1.000000000000000000 ) ) ;
#25026 = CARTESIAN_POINT ( 'NONE',  ( 19.99999662536857770, 86.60254037844397601, 12.50000000000000000 ) ) ;
#25027 = AXIS2_PLACEMENT_3D ( 'NONE', #1816, #1253, #23955 ) ;
#25028 = DIRECTION ( 'NONE',  ( 1.000000000000000000, 0.000000000000000000, 0.000000000000000000 ) ) ;
#25029 = CARTESIAN_POINT ( 'NONE',  ( 74.99999662536835388, -43.30127018922199511, -5.000000000000000000 ) ) ;
#25030 = CARTESIAN_POINT ( 'NONE',  ( 23.49188653442568864, 103.5527583403323035, 27.49999400000000094 ) ) ;
#25031 = AXIS2_PLACEMENT_3D ( 'NONE', #432, #34223, #17676 ) ;
#25032 = CARTESIAN_POINT ( 'NONE',  ( -35.00000337463117717, -77.94228634059963667, -5.000000000000000000 ) ) ;
#25033 = VERTEX_POINT ( 'NONE', #13100 ) ;
#25034 = CARTESIAN_POINT ( 'NONE',  ( -10.00000337463128197, 86.60254037844397601, -9.999999999999998224 ) ) ;
#25035 = CIRCLE ( 'NONE', #18441, 2.000000000000001776 ) ;
#25036 = DIRECTION ( 'NONE',  ( -0.000000000000000000, -0.000000000000000000, 1.000000000000000000 ) ) ;
#25037 = CARTESIAN_POINT ( 'NONE',  ( 5.999999999999999112, 3.980102097228899218E-16, 3.250000000000001332 ) ) ;
#25038 = CIRCLE ( 'NONE', #31593, 95.00000000000001421 ) ;
#25039 = ORIENTED_EDGE ( 'NONE', *, *, #35009, .T. ) ;
#25040 = ORIENTED_EDGE ( 'NONE', *, *, #29359, .T. ) ;
#25041 = EDGE_CURVE ( 'NONE', #20586, #11580, #3552, .T. ) ;
#25042 = ORIENTED_EDGE ( 'NONE', *, *, #33020, .F. ) ;
#25043 = AXIS2_PLACEMENT_3D ( 'NONE', #6062, #17487, #36644 ) ;
#25044 = DIRECTION ( 'NONE',  ( 1.000000000000000000, 0.000000000000000000, 0.000000000000000000 ) ) ;
#25045 = LINE ( 'NONE', #13945, #29827 ) ;
#25046 = ADVANCED_FACE ( 'NONE', ( #12896 ), #13274, .F. ) ;
#25047 = EDGE_LOOP ( 'NONE', ( #2910, #7191, #29886, #23337, #6641, #14959, #3597, #12141 ) ) ;
#25048 = CARTESIAN_POINT ( 'NONE',  ( -58.00000337463107059, -34.64101615137762025, 12.50000000000000000 ) ) ;
#25049 = DIRECTION ( 'NONE',  ( 1.000000000000000000, 0.000000000000000000, 0.000000000000000000 ) ) ;
#25050 = EDGE_LOOP ( 'NONE', ( #31208, #12214 ) ) ;
#25051 = CARTESIAN_POINT ( 'NONE',  ( 106.7731239591688848, 98.28784258492994752, 32.55002500000000509 ) ) ;
#25053 = ADVANCED_FACE ( 'NONE', ( #13447 ), #24725, .F. ) ;
#25052 = ORIENTED_EDGE ( 'NONE', *, *, #1794, .T. ) ;
#25054 = CARTESIAN_POINT ( 'NONE',  ( -82.00000337463096400, -34.64101615137762025, -9.999999999999998224 ) ) ;
#25055 = CIRCLE ( 'NONE', #3467, 2.000000000000001776 ) ;
#25056 = CARTESIAN_POINT ( 'NONE',  ( 86.99999662536831124, -8.660254037844397956, -9.999999999999998224 ) ) ;
#25057 = CARTESIAN_POINT ( 'NONE',  ( -35.00000337463117717, -77.94228634059963667, 12.50000000000000000 ) ) ;
#25058 = CIRCLE ( 'NONE', #8869, 2.000000000000001776 ) ;
#25059 = VERTEX_POINT ( 'NONE', #10661 ) ;
#25060 = LINE ( 'NONE', #2921, #12877 ) ;
#25061 = CIRCLE ( 'NONE', #7086, 2.000000000000001776 ) ;
#25062 = AXIS2_PLACEMENT_3D ( 'NONE', #31308, #5627, #17065 ) ;
#25063 = EDGE_CURVE ( 'NONE', #27693, #29836, #32314, .T. ) ;
#25064 = AXIS2_PLACEMENT_3D ( 'NONE', #6693, #18120, #15308 ) ;
#25065 = DIRECTION ( 'NONE',  ( 0.000000000000000000, 0.000000000000000000, 1.000000000000000000 ) ) ;
#25066 = EDGE_CURVE ( 'NONE', #30130, #29077, #3580, .T. ) ;
#25067 = DIRECTION ( 'NONE',  ( -0.000000000000000000, -0.000000000000000000, -1.000000000000000000 ) ) ;
#25068 = AXIS2_PLACEMENT_3D ( 'NONE', #28319, #11075, #5636 ) ;
#25069 = EDGE_CURVE ( 'NONE', #35055, #32859, #36158, .T. ) ;
#25070 = ORIENTED_EDGE ( 'NONE', *, *, #19520, .T. ) ;
#25071 = CARTESIAN_POINT ( 'NONE',  ( -62.97617850287781494, -4.279621169095772615, 12.49999999999999822 ) ) ;
#25072 = CARTESIAN_POINT ( 'NONE',  ( 0.000000000000000000, 0.000000000000000000, 15.00000000000000000 ) ) ;
#25073 = ADVANCED_FACE ( 'NONE', ( #30703 ), #10461, .F. ) ;
#25074 = ORIENTED_EDGE ( 'NONE', *, *, #28914, .T. ) ;
#25075 = LINE ( 'NONE', #28231, #25606 ) ;
#25076 = CARTESIAN_POINT ( 'NONE',  ( 0.000000000000000000, -2.935248768560059229, 3.469446951953614189E-15 ) ) ;
#25077 = FACE_OUTER_BOUND ( 'NONE', #9898, .T. ) ;
#25078 = AXIS2_PLACEMENT_3D ( 'NONE', #20103, #8855, #34362 ) ;
#25079 = ORIENTED_EDGE ( 'NONE', *, *, #34940, .T. ) ;
#25080 = ORIENTED_EDGE ( 'NONE', *, *, #12876, .T. ) ;
#25081 = CARTESIAN_POINT ( 'NONE',  ( 3.000000000000000000, 1.467624384280024730, -2.542000000000001592 ) ) ;
#25082 = AXIS2_PLACEMENT_3D ( 'NONE', #35100, #7470, #9909 ) ;
#25083 = CARTESIAN_POINT ( 'NONE',  ( 4.999999999999999112, 2.886751345948125991, -3.984345921091767551 ) ) ;
#25084 = LINE ( 'NONE', #30854, #30273 ) ;
#25085 = ORIENTED_EDGE ( 'NONE', *, *, #23576, .T. ) ;
#25086 = ORIENTED_EDGE ( 'NONE', *, *, #7808, .F. ) ;
#25087 = AXIS2_PLACEMENT_3D ( 'NONE', #346, #11972, #14991 ) ;
#25088 = CARTESIAN_POINT ( 'NONE',  ( 66.99999662536841072, 25.98076211353318854, -9.999999999999998224 ) ) ;
#25089 = CARTESIAN_POINT ( 'NONE',  ( -81.86307664143558327, 18.04780306571548820, -5.000000000000000000 ) ) ;
#25090 = VECTOR ( 'NONE', #8707, 1000.000000000000000 ) ;
#25091 = CARTESIAN_POINT ( 'NONE',  ( 3.000000000000000000, -1.467624384280032501, -2.541999999999998483 ) ) ;
#25092 = CARTESIAN_POINT ( 'NONE',  ( -2.000003374631303732, -86.60254037844400443, 17.49999999999999645 ) ) ;
#25093 = ADVANCED_FACE ( 'NONE', ( #27145 ), #13654, .F. ) ;
#25094 = ORIENTED_EDGE ( 'NONE', *, *, #30701, .F. ) ;
#25095 = ORIENTED_EDGE ( 'NONE', *, *, #1405, .F. ) ;
#25096 = AXIS2_PLACEMENT_3D ( 'NONE', #8423, #28277, #28457 ) ;
#25097 = CARTESIAN_POINT ( 'NONE',  ( -34.00000000000000000, 103.4105893997321743, 32.50000000000000000 ) ) ;
#25098 = EDGE_LOOP ( 'NONE', ( #34333, #26821 ) ) ;
#25099 = CIRCLE ( 'NONE', #18503, 65.00000000000000000 ) ;
#25100 = DIRECTION ( 'NONE',  ( 1.000000000000000000, 0.000000000000000000, 0.000000000000000000 ) ) ;
#25101 = ORIENTED_EDGE ( 'NONE', *, *, #29216, .F. ) ;
#25102 = FACE_BOUND ( 'NONE', #21626, .T. ) ;
#25103 = CIRCLE ( 'NONE', #23916, 1.999999999999998224 ) ;
#25104 = AXIS2_PLACEMENT_3D ( 'NONE', #29082, #14651, #21721 ) ;
#25105 = DIRECTION ( 'NONE',  ( 0.000000000000000000, 0.000000000000000000, 1.000000000000000000 ) ) ;
#25106 = CARTESIAN_POINT ( 'NONE',  ( -10.00000337463127842, -69.28203230275519786, -9.999999999999998224 ) ) ;
#25107 = EDGE_LOOP ( 'NONE', ( #1635, #28612 ) ) ;
#25108 = DIRECTION ( 'NONE',  ( 0.4245330536251072928, 0.9054124399298598691, 0.000000000000000000 ) ) ;
#25109 = CARTESIAN_POINT ( 'NONE',  ( 52.99999662536844625, 60.62177826491077326, 12.50000000000000000 ) ) ;
#25110 = CIRCLE ( 'NONE', #4739, 2.000000000000001776 ) ;
#25111 = DIRECTION ( 'NONE',  ( 1.000000000000000000, 0.000000000000000000, 0.000000000000000000 ) ) ;
#25112 = CARTESIAN_POINT ( 'NONE',  ( 69.99999662536841072, 51.96152422706640550, -9.999999999999998224 ) ) ;
#25113 = EDGE_CURVE ( 'NONE', #7675, #22212, #15725, .T. ) ;
#25114 = ORIENTED_EDGE ( 'NONE', *, *, #26435, .T. ) ;
#25115 = CARTESIAN_POINT ( 'NONE',  ( 44.99999662536851019, -60.62177826491080168, 12.50000000000000000 ) ) ;
#25116 = VECTOR ( 'NONE', #34194, 1000.000000000000000 ) ;
#25117 = CARTESIAN_POINT ( 'NONE',  ( -55.27226924886021919, 77.26562141134635908, 27.50000000000000000 ) ) ;
#25118 = DIRECTION ( 'NONE',  ( 0.000000000000000000, 0.000000000000000000, 1.000000000000000000 ) ) ;
#25119 = ORIENTED_EDGE ( 'NONE', *, *, #20778, .F. ) ;
#25120 = ORIENTED_EDGE ( 'NONE', *, *, #24723, .F. ) ;
#25121 = AXIS2_PLACEMENT_3D ( 'NONE', #22683, #17242, #19011 ) ;
#25122 = DIRECTION ( 'NONE',  ( 0.000000000000000000, 0.000000000000000000, 1.000000000000000000 ) ) ;
#25123 = ORIENTED_EDGE ( 'NONE', *, *, #26567, .T. ) ;
#25124 = CYLINDRICAL_SURFACE ( 'NONE', #22926, 2.000000000000001776 ) ;
#25125 = DIRECTION ( 'NONE',  ( 0.000000000000000000, 0.000000000000000000, 1.000000000000000000 ) ) ;
#25126 = AXIS2_PLACEMENT_3D ( 'NONE', #28801, #13994, #8747 ) ;
#25127 = CARTESIAN_POINT ( 'NONE',  ( 76.99999662536836809, 43.30127018922198801, -5.000000000000000000 ) ) ;
#25128 = AXIS2_PLACEMENT_3D ( 'NONE', #16107, #30534, #10103 ) ;
#25129 = CARTESIAN_POINT ( 'NONE',  ( 66.99999662536839651, -60.62177826491080168, -9.999999999999998224 ) ) ;
#25130 = CIRCLE ( 'NONE', #13738, 2.000000000000000000 ) ;
#25131 = CARTESIAN_POINT ( 'NONE',  ( 88.03900239164613595, -71.83446256730503876, 32.49999999999999289 ) ) ;
#25132 = DIRECTION ( 'NONE',  ( 0.000000000000000000, 0.000000000000000000, 1.000000000000000000 ) ) ;
#25133 = CARTESIAN_POINT ( 'NONE',  ( 0.000000000000000000, 89.94802294027094547, 32.49999999999999289 ) ) ;
#25134 = EDGE_CURVE ( 'NONE', #34700, #36279, #24553, .T. ) ;
#25135 = CARTESIAN_POINT ( 'NONE',  ( -27.00000337463121625, -77.94228634059963667, -5.000000000000000000 ) ) ;
#25136 = ORIENTED_EDGE ( 'NONE', *, *, #6005, .T. ) ;
#25137 = ORIENTED_EDGE ( 'NONE', *, *, #35695, .F. ) ;
#25138 = CIRCLE ( 'NONE', #13742, 2.000000000000001776 ) ;
#25139 = DIRECTION ( 'NONE',  ( 0.000000000000000000, 0.000000000000000000, 1.000000000000000000 ) ) ;
#25140 = LINE ( 'NONE', #36570, #36701 ) ;
#25141 = CARTESIAN_POINT ( 'NONE',  ( 0.000000000000000000, -1.467624384280032501, -2.541999999999998483 ) ) ;
#25142 = DIRECTION ( 'NONE',  ( -0.000000000000000000, -0.000000000000000000, -1.000000000000000000 ) ) ;
#25143 = EDGE_CURVE ( 'NONE', #1110, #36232, #10282, .T. ) ;
#25144 = ORIENTED_EDGE ( 'NONE', *, *, #15845, .F. ) ;
#25145 = AXIS2_PLACEMENT_3D ( 'NONE', #37092, #36893, #16657 ) ;
#25146 = EDGE_CURVE ( 'NONE', #16685, #33091, #20949, .T. ) ;
#25147 = CARTESIAN_POINT ( 'NONE',  ( 5.000000000000000000, -2.058885705017528878, -1.328630925609301183 ) ) ;
#25148 = ORIENTED_EDGE ( 'NONE', *, *, #4748, .F. ) ;
#25149 = ORIENTED_EDGE ( 'NONE', *, *, #9686, .F. ) ;
#25150 = CARTESIAN_POINT ( 'NONE',  ( 17.99999662536858835, 69.28203230275516944, -5.000000000000000000 ) ) ;
#25151 = ORIENTED_EDGE ( 'NONE', *, *, #4957, .F. ) ;
#25152 = CIRCLE ( 'NONE', #29922, 2.000000000000001776 ) ;
#25153 = DIRECTION ( 'NONE',  ( 0.000000000000000000, 0.000000000000000000, 1.000000000000000000 ) ) ;
#25154 = DIRECTION ( 'NONE',  ( 0.000000000000000000, 0.000000000000000000, 1.000000000000000000 ) ) ;
#25155 = AXIS2_PLACEMENT_3D ( 'NONE', #4056, #17940, #29368 ) ;
#25156 = DIRECTION ( 'NONE',  ( -1.000000000000000000, 0.000000000000000000, 0.000000000000000000 ) ) ;
#25157 = CIRCLE ( 'NONE', #11379, 150.0000000000000284 ) ;
#25158 = EDGE_CURVE ( 'NONE', #16300, #27851, #8378, .T. ) ;
#25159 = ORIENTED_EDGE ( 'NONE', *, *, #29905, .F. ) ;
#25160 = VERTEX_POINT ( 'NONE', #17010 ) ;
#25161 = VECTOR ( 'NONE', #25328, 1000.000000000000000 ) ;
#25162 = ORIENTED_EDGE ( 'NONE', *, *, #19451, .T. ) ;
#25163 = EDGE_LOOP ( 'NONE', ( #30686, #13062 ) ) ;
#25164 = CARTESIAN_POINT ( 'NONE',  ( -65.00000337463104927, -25.98076211353322051, 17.49999999999999645 ) ) ;
#25165 = AXIS2_PLACEMENT_3D ( 'NONE', #1899, #13151, #33195 ) ;
#25166 = LINE ( 'NONE', #36410, #17966 ) ;
#25167 = VECTOR ( 'NONE', #27107, 1000.000000000000000 ) ;
#25168 = DIRECTION ( 'NONE',  ( 1.000000000000000000, 0.000000000000000000, 0.000000000000000000 ) ) ;
#25169 = FACE_OUTER_BOUND ( 'NONE', #20346, .T. ) ;
#25170 = CARTESIAN_POINT ( 'NONE',  ( 4.999999999999998224, 1.026530412860235053, -3.969857242416569232 ) ) ;
#25171 = EDGE_LOOP ( 'NONE', ( #16058, #10433, #3748, #3290 ) ) ;
#25172 = FACE_OUTER_BOUND ( 'NONE', #26922, .T. ) ;
#25173 = EDGE_CURVE ( 'NONE', #16509, #28869, #10170, .T. ) ;
#25174 = DIRECTION ( 'NONE',  ( 0.000000000000000000, 0.000000000000000000, -1.000000000000000000 ) ) ;
#25175 = ADVANCED_FACE ( 'NONE', ( #13836 ), #22837, .F. ) ;
#25176 = DIRECTION ( 'NONE',  ( 1.000000000000000000, -3.846960960290410782E-15, 0.000000000000000000 ) ) ;
#25177 = VERTEX_POINT ( 'NONE', #3135 ) ;
#25178 = PLANE ( 'NONE',  #32204 ) ;
#25179 = CARTESIAN_POINT ( 'NONE',  ( 59.99999662536842493, 51.96152422706639129, -9.999999999999998224 ) ) ;
#25180 = AXIS2_PLACEMENT_3D ( 'NONE', #25311, #36194, #36576 ) ;
#25181 = ORIENTED_EDGE ( 'NONE', *, *, #32520, .F. ) ;
#25182 = ORIENTED_EDGE ( 'NONE', *, *, #25707, .T. ) ;
#25183 = DIRECTION ( 'NONE',  ( 0.000000000000000000, 0.000000000000000000, 1.000000000000000000 ) ) ;
#25184 = DIRECTION ( 'NONE',  ( 0.000000000000000000, 0.000000000000000000, 1.000000000000000000 ) ) ;
#25185 = AXIS2_PLACEMENT_3D ( 'NONE', #22890, #29043, #34709 ) ;
#25186 = CARTESIAN_POINT ( 'NONE',  ( 1.582370436567792638, -4.859920694386177686, -3.719399823475529665 ) ) ;
#25187 = CARTESIAN_POINT ( 'NONE',  ( -0.8082922630888651483, -5.306834936218053578, -0.2701150775514121749 ) ) ;
#25188 = ADVANCED_FACE ( 'NONE', ( #5218 ), #2582, .T. ) ;
#25189 = ORIENTED_EDGE ( 'NONE', *, *, #8887, .F. ) ;
#25190 = ORIENTED_EDGE ( 'NONE', *, *, #30969, .T. ) ;
#25191 = LINE ( 'NONE', #10742, #33861 ) ;
#25192 = EDGE_CURVE ( 'NONE', #8893, #4052, #11364, .T. ) ;
#25193 = ORIENTED_EDGE ( 'NONE', *, *, #2349, .T. ) ;
#25194 = FACE_OUTER_BOUND ( 'NONE', #36742, .T. ) ;
#25195 = VERTEX_POINT ( 'NONE', #31256 ) ;
#25196 = ORIENTED_EDGE ( 'NONE', *, *, #7587, .F. ) ;
#25197 = CARTESIAN_POINT ( 'NONE',  ( 66.86787810013036903, -2.778182860042780700, 12.49999999999999645 ) ) ;
#25198 = CARTESIAN_POINT ( 'NONE',  ( 5.999999999999998224, 145.0000000000000568, 32.50000000000000000 ) ) ;
#25199 = EDGE_LOOP ( 'NONE', ( #29287, #2140, #23365, #10540 ) ) ;
#25200 = ORIENTED_EDGE ( 'NONE', *, *, #6232, .F. ) ;
#25201 = DIRECTION ( 'NONE',  ( -0.000000000000000000, -0.000000000000000000, 1.000000000000000000 ) ) ;
#25202 = DIRECTION ( 'NONE',  ( -1.000000000000000000, 0.000000000000000000, 0.000000000000000000 ) ) ;
#25203 = DIRECTION ( 'NONE',  ( 0.000000000000000000, 0.000000000000000000, 1.000000000000000000 ) ) ;
#25204 = FACE_OUTER_BOUND ( 'NONE', #13102, .T. ) ;
#25205 = EDGE_CURVE ( 'NONE', #15973, #9156, #8954, .T. ) ;
#25206 = ORIENTED_EDGE ( 'NONE', *, *, #3350, .F. ) ;
#25207 = FACE_OUTER_BOUND ( 'NONE', #31508, .T. ) ;
#25208 = FACE_BOUND ( 'NONE', #3778, .T. ) ;
#25209 = CARTESIAN_POINT ( 'NONE',  ( -35.00000337463116296, -60.62177826491080168, -9.999999999999998224 ) ) ;
#25210 = DIRECTION ( 'NONE',  ( -0.8660254037844380415, 0.5000000000000009992, 0.000000000000000000 ) ) ;
#25211 = CYLINDRICAL_SURFACE ( 'NONE', #14114, 45.00000000000000000 ) ;
#25212 = DIRECTION ( 'NONE',  ( 1.000000000000000000, 0.000000000000000000, 0.000000000000000000 ) ) ;
#25213 = EDGE_CURVE ( 'NONE', #4661, #19051, #13750, .T. ) ;
#25214 = CARTESIAN_POINT ( 'NONE',  ( -32.16008401677955675, -61.25926521283091830, 12.49999999999999645 ) ) ;
#25215 = EDGE_CURVE ( 'NONE', #18936, #10178, #2966, .T. ) ;
#25216 = DIRECTION ( 'NONE',  ( 0.000000000000000000, 0.000000000000000000, 1.000000000000000000 ) ) ;
#25217 = ORIENTED_EDGE ( 'NONE', *, *, #29961, .T. ) ;
#25218 = DIRECTION ( 'NONE',  ( 0.000000000000000000, 0.000000000000000000, 1.000000000000000000 ) ) ;
#25219 = DIRECTION ( 'NONE',  ( -0.8660254037844379305, 0.5000000000000011102, 0.000000000000000000 ) ) ;
#25220 = DIRECTION ( 'NONE',  ( 0.000000000000000000, 0.000000000000000000, 1.000000000000000000 ) ) ;
#25221 = ORIENTED_EDGE ( 'NONE', *, *, #29549, .T. ) ;
#25222 = ORIENTED_EDGE ( 'NONE', *, *, #10515, .F. ) ;
#25223 = ORIENTED_EDGE ( 'NONE', *, *, #30016, .T. ) ;
#25224 = CARTESIAN_POINT ( 'NONE',  ( -4.220252828340121276, -79.78402168683115292, -5.000000000000000000 ) ) ;
#25225 = CYLINDRICAL_SURFACE ( 'NONE', #16380, 6.000000000000005329 ) ;
#25226 = VERTEX_POINT ( 'NONE', #26002 ) ;
#25227 = DIRECTION ( 'NONE',  ( 1.000000000000000000, 0.000000000000000000, 0.000000000000000000 ) ) ;
#25228 = EDGE_CURVE ( 'NONE', #7161, #20458, #28120, .T. ) ;
#25229 = FACE_OUTER_BOUND ( 'NONE', #6975, .T. ) ;
#25230 = ORIENTED_EDGE ( 'NONE', *, *, #3405, .T. ) ;
#25231 = DIRECTION ( 'NONE',  ( 0.000000000000000000, 0.000000000000000000, 1.000000000000000000 ) ) ;
#25232 = ORIENTED_EDGE ( 'NONE', *, *, #4365, .T. ) ;
#25233 = CARTESIAN_POINT ( 'NONE',  ( 43.19957991610432657, 47.04203867989531318, 12.49999999999999822 ) ) ;
#25234 = CARTESIAN_POINT ( 'NONE',  ( -2.287832656137188891, 4.452621892014637872, -6.000000000000004441 ) ) ;
#25235 = DIRECTION ( 'NONE',  ( 1.000000000000000000, 0.000000000000000000, 0.000000000000000000 ) ) ;
#25236 = EDGE_LOOP ( 'NONE', ( #14348, #11325, #11598, #23604 ) ) ;
#25237 = CARTESIAN_POINT ( 'NONE',  ( -33.00000337463116296, 77.94228634059957983, -9.999999999999998224 ) ) ;
#25238 = CARTESIAN_POINT ( 'NONE',  ( 49.99999662536846756, 69.28203230275516944, -5.000000000000000000 ) ) ;
#25239 = DIRECTION ( 'NONE',  ( 0.000000000000000000, 0.000000000000000000, 1.000000000000000000 ) ) ;
#25240 = ADVANCED_FACE ( 'NONE', ( #20200 ), #16841, .F. ) ;
#25241 = ORIENTED_EDGE ( 'NONE', *, *, #23458, .T. ) ;
#25242 = DIRECTION ( 'NONE',  ( 0.000000000000000000, 0.000000000000000000, 1.000000000000000000 ) ) ;
#25243 = CARTESIAN_POINT ( 'NONE',  ( 72.72667006429115588, 101.6652913307178636, 32.50000000000000000 ) ) ;
#25244 = VERTEX_POINT ( 'NONE', #17393 ) ;
#25245 = ADVANCED_FACE ( 'NONE', ( #11743 ), #30884, .F. ) ;
#25246 = DIRECTION ( 'NONE',  ( -0.000000000000000000, -0.000000000000000000, -1.000000000000000000 ) ) ;
#25247 = VECTOR ( 'NONE', #19684, 1000.000000000000000 ) ;
#25248 = CARTESIAN_POINT ( 'NONE',  ( -85.00000337463092137, 25.98076211353317433, -5.000000000000000000 ) ) ;
#25249 = CARTESIAN_POINT ( 'NONE',  ( 34.60911832077664485, -75.98085468209112037, -5.000000000000000000 ) ) ;
#25250 = CARTESIAN_POINT ( 'NONE',  ( 7.999996625368618552, 69.28203230275516944, 12.50000000000000000 ) ) ;
#25251 = EDGE_CURVE ( 'NONE', #34636, #13116, #34716, .T. ) ;
#25252 = ORIENTED_EDGE ( 'NONE', *, *, #21716, .T. ) ;
#25253 = ORIENTED_EDGE ( 'NONE', *, *, #32048, .F. ) ;
#25254 = EDGE_CURVE ( 'NONE', #4855, #36034, #2386, .T. ) ;
#25255 = FACE_OUTER_BOUND ( 'NONE', #22264, .T. ) ;
#25256 = CARTESIAN_POINT ( 'NONE',  ( 64.99999662536841072, 25.98076211353318854, -9.999999999999998224 ) ) ;
#25257 = EDGE_CURVE ( 'NONE', #13225, #26423, #35343, .T. ) ;
#25258 = ORIENTED_EDGE ( 'NONE', *, *, #24219, .T. ) ;
#25259 = ORIENTED_EDGE ( 'NONE', *, *, #9656, .T. ) ;
#25260 = DIRECTION ( 'NONE',  ( 0.000000000000000000, 0.000000000000000000, 1.000000000000000000 ) ) ;
#25261 = DIRECTION ( 'NONE',  ( -1.000000000000000000, 0.000000000000000000, 0.000000000000000000 ) ) ;
#25262 = CARTESIAN_POINT ( 'NONE',  ( -40.98360655737705827, 111.1639425680974398, -19.99999999999999645 ) ) ;
#25263 = EDGE_CURVE ( 'NONE', #26293, #19500, #14368, .T. ) ;
#25264 = VERTEX_POINT ( 'NONE', #5413 ) ;
#25266 = EDGE_LOOP ( 'NONE', ( #1477, #27090, #21613, #47, #27509 ) ) ;
#25265 = EDGE_CURVE ( 'NONE', #5579, #33065, #17952, .T. ) ;
#25267 = EDGE_CURVE ( 'NONE', #13323, #26293, #26941, .T. ) ;
#25268 = VECTOR ( 'NONE', #33449, 1000.000000000000000 ) ;
#25269 = CYLINDRICAL_SURFACE ( 'NONE', #21891, 1.999999999999998224 ) ;
#25271 = EDGE_CURVE ( 'NONE', #33506, #32494, #31438, .T. ) ;
#25270 = EDGE_LOOP ( 'NONE', ( #12356, #13747, #22751, #17969 ) ) ;
#25272 = CARTESIAN_POINT ( 'NONE',  ( 34.99999662536855283, -60.62177826491080168, -9.999999999999998224 ) ) ;
#25273 = ORIENTED_EDGE ( 'NONE', *, *, #27193, .T. ) ;
#25274 = VECTOR ( 'NONE', #14461, 1000.000000000000000 ) ;
#25275 = FACE_BOUND ( 'NONE', #30879, .T. ) ;
#25276 = DIRECTION ( 'NONE',  ( -0.000000000000000000, -0.000000000000000000, -1.000000000000000000 ) ) ;
#25277 = ORIENTED_EDGE ( 'NONE', *, *, #5859, .F. ) ;
#25278 = DIRECTION ( 'NONE',  ( 0.000000000000000000, 0.000000000000000000, 1.000000000000000000 ) ) ;
#25279 = DIRECTION ( 'NONE',  ( 0.000000000000000000, 0.000000000000000000, -1.000000000000000000 ) ) ;
#25280 = B_SPLINE_CURVE_WITH_KNOTS ( 'NONE', 3,
 ( #15159, #21157, #26595, #9724, #23801 ),
 .UNSPECIFIED., .F., .F.,
 ( 4, 1, 4 ),
 ( 0.000000000000000000, 0.002886751345948134623, 0.005773502691896269245 ),
 .UNSPECIFIED. ) ;
#25281 = CARTESIAN_POINT ( 'NONE',  ( 79.99999662536833966, 17.32050807568879236, -9.999999999999998224 ) ) ;
#25282 = DIRECTION ( 'NONE',  ( 1.000000000000000000, 0.000000000000000000, 0.000000000000000000 ) ) ;
#25283 = EDGE_LOOP ( 'NONE', ( #3934, #3680 ) ) ;
#25284 = CARTESIAN_POINT ( 'NONE',  ( 64.99999662536839651, -43.30127018922199511, -9.999999999999998224 ) ) ;
#25285 = DIRECTION ( 'NONE',  ( 0.000000000000000000, 0.000000000000000000, 1.000000000000000000 ) ) ;
#25286 = LINE ( 'NONE', #36716, #14742 ) ;
#25287 = ORIENTED_EDGE ( 'NONE', *, *, #2751, .F. ) ;
#25288 = ORIENTED_EDGE ( 'NONE', *, *, #33626, .F. ) ;
#25289 = AXIS2_PLACEMENT_3D ( 'NONE', #10172, #33203, #36042 ) ;
#25290 = DIRECTION ( 'NONE',  ( 1.000000000000000000, 0.000000000000000000, 0.000000000000000000 ) ) ;
#25291 = ORIENTED_EDGE ( 'NONE', *, *, #18390, .F. ) ;
#25292 = DIRECTION ( 'NONE',  ( -1.000000000000000000, 0.000000000000000000, 0.000000000000000000 ) ) ;
#25293 = DIRECTION ( 'NONE',  ( 0.000000000000000000, 0.000000000000000000, -1.000000000000000000 ) ) ;
#25294 = FACE_OUTER_BOUND ( 'NONE', #2836, .T. ) ;
#25295 = LINE ( 'NONE', #28456, #25437 ) ;
#25296 = CARTESIAN_POINT ( 'NONE',  ( 97.20652429509418369, -67.55932235215701098, 32.50000000000000711 ) ) ;
#25297 = CARTESIAN_POINT ( 'NONE',  ( 77.93337651276290501, -72.12094976675109592, 32.50001250000000397 ) ) ;
#25298 = CARTESIAN_POINT ( 'NONE',  ( -10.00000337463127842, -69.28203230275519786, 12.50000000000000000 ) ) ;
#25299 = LINE ( 'NONE', #20226, #25658 ) ;
#25300 = ORIENTED_EDGE ( 'NONE', *, *, #10347, .F. ) ;
#25301 = VERTEX_POINT ( 'NONE', #12282 ) ;
#25302 = AXIS2_PLACEMENT_3D ( 'NONE', #21594, #13144, #15590 ) ;
#25303 = CIRCLE ( 'NONE', #20487, 3.000000000000007550 ) ;
#25304 = DIRECTION ( 'NONE',  ( 0.000000000000000000, 0.000000000000000000, 1.000000000000000000 ) ) ;
#25305 = CARTESIAN_POINT ( 'NONE',  ( 102.5304832720488832, -102.5304832720499633, 32.55002500000000509 ) ) ;
#25306 = ADVANCED_FACE ( 'NONE', ( #21116 ), #35209, .F. ) ;
#25307 = DIRECTION ( 'NONE',  ( 0.000000000000000000, 0.000000000000000000, 1.000000000000000000 ) ) ;
#25308 = FACE_OUTER_BOUND ( 'NONE', #31651, .T. ) ;
#25309 = EDGE_LOOP ( 'NONE', ( #4164, #335, #9127, #36881 ) ) ;
#25310 = PRODUCT_DEFINITION_CONTEXT ( 'detailed design', #8705, 'design' ) ;
#25311 = CARTESIAN_POINT ( 'NONE',  ( 34.99999662536855283, -60.62177826491080168, -5.000000000000000000 ) ) ;
#25312 = EDGE_LOOP ( 'NONE', ( #30770, #30613, #22392, #1900, #23890 ) ) ;
#25313 = AXIS2_PLACEMENT_3D ( 'NONE', #20058, #22513, #5628 ) ;
#25314 = ORIENTED_EDGE ( 'NONE', *, *, #6188, .F. ) ;
#25315 = DIRECTION ( 'NONE',  ( 1.000000000000000000, 0.000000000000000000, 0.000000000000000000 ) ) ;
#25316 = EDGE_LOOP ( 'NONE', ( #34915, #5409, #31026, #31550 ) ) ;
#25317 = DIRECTION ( 'NONE',  ( 0.000000000000000000, 0.000000000000000000, 1.000000000000000000 ) ) ;
#25318 = LINE ( 'NONE', #31128, #32591 ) ;
#25319 = DIRECTION ( 'NONE',  ( -1.000000000000000000, -0.000000000000000000, -0.000000000000000000 ) ) ;
#25320 = EDGE_LOOP ( 'NONE', ( #24222, #32919 ) ) ;
#25321 = EDGE_LOOP ( 'NONE', ( #4230, #21796, #15699, #17248 ) ) ;
#25322 = ADVANCED_FACE ( 'NONE', ( #32376 ), #3314, .T. ) ;
#25323 = ORIENTED_EDGE ( 'NONE', *, *, #29359, .F. ) ;
#25324 = EDGE_CURVE ( 'NONE', #17904, #21445, #1788, .T. ) ;
#25325 = EDGE_LOOP ( 'NONE', ( #1113, #15066, #32905, #8100 ) ) ;
#25326 = VERTEX_POINT ( 'NONE', #18115 ) ;
#25327 = CARTESIAN_POINT ( 'NONE',  ( -5.000000000000000000, 6.123233995736766282E-16, 2.266666666666666607 ) ) ;
#25328 = DIRECTION ( 'NONE',  ( 0.000000000000000000, 0.000000000000000000, 1.000000000000000000 ) ) ;
#25329 = CARTESIAN_POINT ( 'NONE',  ( 74.99999662536836809, 43.30127018922198801, -9.999999999999998224 ) ) ;
#25330 = CARTESIAN_POINT ( 'NONE',  ( -77.00000337463097821, 25.98076211353318854, 17.49999999999999645 ) ) ;
#25331 = B_SPLINE_CURVE_WITH_KNOTS ( 'NONE', 3,
 ( #33741, #33371, #36564, #4697, #19139, #2239 ),
 .UNSPECIFIED., .F., .F.,
 ( 4, 2, 4 ),
 ( -3.988673288092903537E-06, 0.0002483701411510707939, 0.0005007289555902344176 ),
 .UNSPECIFIED. ) ;
#25332 = CARTESIAN_POINT ( 'NONE',  ( 4.999999999999999112, 3.131512667671952688, -4.027950064282237896 ) ) ;
#25333 = VERTEX_POINT ( 'NONE', #26383 ) ;
#25334 = CARTESIAN_POINT ( 'NONE',  ( -72.72667006428976322, 101.6652913307188868, 32.50000000000000000 ) ) ;
#25335 = DIRECTION ( 'NONE',  ( -1.000000000000000000, 0.000000000000000000, 0.000000000000000000 ) ) ;
#25336 = ADVANCED_FACE ( 'NONE', ( #6129 ), #29732, .F. ) ;
#25337 = AXIS2_PLACEMENT_3D ( 'NONE', #6829, #17913, #35171 ) ;
#25338 = DIRECTION ( 'NONE',  ( -1.000000000000000000, 0.000000000000000000, 0.000000000000000000 ) ) ;
#25339 = VERTEX_POINT ( 'NONE', #15304 ) ;
#25340 = CARTESIAN_POINT ( 'NONE',  ( 3.000000000000000000, 1.467624384280029615, 2.541999999999997151 ) ) ;
#25341 = DIRECTION ( 'NONE',  ( 0.000000000000000000, 0.000000000000000000, 1.000000000000000000 ) ) ;
#25342 = EDGE_LOOP ( 'NONE', ( #15139, #730 ) ) ;
#25343 = VERTEX_POINT ( 'NONE', #32176 ) ;
#25344 = CARTESIAN_POINT ( 'NONE',  ( 58.88972745734226066, 33.99999999999924682, 12.49999999999999822 ) ) ;
#25345 = CARTESIAN_POINT ( 'NONE',  ( -3.514986608498369414, 4.017641317390100220, -4.057689166958530436 ) ) ;
#25346 = EDGE_CURVE ( 'NONE', #17463, #1110, #572, .T. ) ;
#25347 = CARTESIAN_POINT ( 'NONE',  ( 74.99999662536836809, 8.660254037844394404, 17.49999999999999645 ) ) ;
#25348 = CARTESIAN_POINT ( 'NONE',  ( -107.0890852396554891, -43.89229305394454173, 32.50000000000001421 ) ) ;
#25349 = ORIENTED_EDGE ( 'NONE', *, *, #6260, .F. ) ;
#25350 = EDGE_LOOP ( 'NONE', ( #27974, #24568 ) ) ;
#25351 = VECTOR ( 'NONE', #15432, 1000.000000000000000 ) ;
#25352 = DIRECTION ( 'NONE',  ( 0.000000000000000000, 0.000000000000000000, 1.000000000000000000 ) ) ;
#25353 = AXIS2_PLACEMENT_3D ( 'NONE', #25305, #8047, #11234 ) ;
#25354 = VERTEX_POINT ( 'NONE', #3863 ) ;
#25355 = DIRECTION ( 'NONE',  ( 0.000000000000000000, 0.000000000000000000, 1.000000000000000000 ) ) ;
#25356 = EDGE_LOOP ( 'NONE', ( #372, #35399, #33142, #24749, #4932 ) ) ;
#25357 = FACE_OUTER_BOUND ( 'NONE', #26719, .T. ) ;
#25358 = CIRCLE ( 'NONE', #16978, 2.000000000000001776 ) ;
#25359 = CARTESIAN_POINT ( 'NONE',  ( 61.25926521283100357, -32.16008401677932227, -4.999999999999997335 ) ) ;
#25360 = AXIS2_PLACEMENT_3D ( 'NONE', #22019, #33821, #7397 ) ;
#25361 = EDGE_CURVE ( 'NONE', #5647, #21660, #20944, .T. ) ;
#25362 = DIRECTION ( 'NONE',  ( 1.000000000000000000, 0.000000000000000000, 0.000000000000000000 ) ) ;
#25363 = ORIENTED_EDGE ( 'NONE', *, *, #8739, .F. ) ;
#25364 = VERTEX_POINT ( 'NONE', #4067 ) ;
#25365 = FACE_OUTER_BOUND ( 'NONE', #23234, .T. ) ;
#25366 = LINE ( 'NONE', #1933, #5197 ) ;
#25367 = EDGE_CURVE ( 'NONE', #36567, #21017, #16167, .T. ) ;
#25368 = AXIS2_PLACEMENT_3D ( 'NONE', #25979, #3114, #11366 ) ;
#25369 = DIRECTION ( 'NONE',  ( 0.000000000000000000, 0.000000000000000000, 1.000000000000000000 ) ) ;
#25370 = DIRECTION ( 'NONE',  ( 0.000000000000000000, 0.000000000000000000, 1.000000000000000000 ) ) ;
#25371 = ORIENTED_EDGE ( 'NONE', *, *, #16979, .T. ) ;
#25372 = CARTESIAN_POINT ( 'NONE',  ( 44.99999662536849598, 60.62177826491077326, 12.50000000000000000 ) ) ;
#25373 = FACE_BOUND ( 'NONE', #17678, .T. ) ;
#25374 = EDGE_CURVE ( 'NONE', #26476, #8984, #5994, .T. ) ;
#25375 = DIRECTION ( 'NONE',  ( -1.000000000000000000, 0.000000000000000000, 0.000000000000000000 ) ) ;
#25376 = VECTOR ( 'NONE', #21616, 1000.000000000000000 ) ;
#25377 = DIRECTION ( 'NONE',  ( 0.000000000000000000, -0.8660254037844420383, -0.4999999999999941713 ) ) ;
#25378 = DIRECTION ( 'NONE',  ( 0.000000000000000000, 0.000000000000000000, 1.000000000000000000 ) ) ;
#25379 = FACE_OUTER_BOUND ( 'NONE', #9623, .T. ) ;
#25380 = DIRECTION ( 'NONE',  ( 0.000000000000000000, 0.000000000000000000, 1.000000000000000000 ) ) ;
#25381 = EDGE_CURVE ( 'NONE', #18749, #11572, #17747, .T. ) ;
#25382 = DIRECTION ( 'NONE',  ( 0.000000000000000000, 0.000000000000000000, 1.000000000000000000 ) ) ;
#25383 = ORIENTED_EDGE ( 'NONE', *, *, #21563, .F. ) ;
#25384 = CYLINDRICAL_SURFACE ( 'NONE', #26224, 2.000000000000001776 ) ;
#25385 = DIRECTION ( 'NONE',  ( 0.000000000000000000, 0.000000000000000000, -1.000000000000000000 ) ) ;
#25386 = CARTESIAN_POINT ( 'NONE',  ( 2.778182860043481028, 66.86787810013034061, -49.86348611802629449 ) ) ;
#25387 = CIRCLE ( 'NONE', #21788, 2.000000000000001776 ) ;
#25388 = ORIENTED_EDGE ( 'NONE', *, *, #37064, .F. ) ;
#25389 = ORIENTED_EDGE ( 'NONE', *, *, #1887, .T. ) ;
#25390 = ORIENTED_EDGE ( 'NONE', *, *, #1879, .T. ) ;
#25391 = VECTOR ( 'NONE', #1909, 1000.000000000000000 ) ;
#25392 = LINE ( 'NONE', #20129, #14149 ) ;
#25393 = DIRECTION ( 'NONE',  ( 1.000000000000000000, 0.000000000000000000, 0.000000000000000000 ) ) ;
#25394 = VERTEX_POINT ( 'NONE', #9692 ) ;
#25395 = CARTESIAN_POINT ( 'NONE',  ( 27.78182860042856461, 56.67878100130339902, -4.999999999999997335 ) ) ;
#25396 = ADVANCED_FACE ( 'NONE', ( #8950 ), #31797, .F. ) ;
#25397 = ORIENTED_EDGE ( 'NONE', *, *, #4827, .T. ) ;
#25398 = CARTESIAN_POINT ( 'NONE',  ( 16.35123109063852098, -113.9563289638309413, 32.50000000000000711 ) ) ;
#25399 = ORIENTED_EDGE ( 'NONE', *, *, #30097, .F. ) ;
#25400 = CARTESIAN_POINT ( 'NONE',  ( 56.67878100130369035, -27.78182860042797131, 12.49999999999999822 ) ) ;
#25401 = ORIENTED_EDGE ( 'NONE', *, *, #13618, .F. ) ;
#25402 = ADVANCED_FACE ( 'NONE', ( #23394 ), #9302, .F. ) ;
#25403 = AXIS2_PLACEMENT_3D ( 'NONE', #34429, #26362, #29353 ) ;
#25404 = CARTESIAN_POINT ( 'NONE',  ( -37.00000337463117717, -77.94228634059963667, 17.49999999999999645 ) ) ;
#25405 = CARTESIAN_POINT ( 'NONE',  ( 47.63139720814418610, 27.49999999999988987, -5.000000000000000888 ) ) ;
#25406 = ADVANCED_FACE ( 'NONE', ( #864 ), #29184, .F. ) ;
#25407 = ORIENTED_EDGE ( 'NONE', *, *, #10744, .T. ) ;
#25408 = CARTESIAN_POINT ( 'NONE',  ( 0.000000000000000000, 0.000000000000000000, -6.000000000000001776 ) ) ;
#25409 = VECTOR ( 'NONE', #7158, 1000.000000000000000 ) ;
#25410 = CARTESIAN_POINT ( 'NONE',  ( -2.778182860042080815, 69.13212189986968781, -49.86348611802629449 ) ) ;
#25411 = DIRECTION ( 'NONE',  ( 0.000000000000000000, 0.000000000000000000, 1.000000000000000000 ) ) ;
#25412 = ORIENTED_EDGE ( 'NONE', *, *, #11161, .F. ) ;
#25413 = CARTESIAN_POINT ( 'NONE',  ( 82.99999662536832545, 25.98076211353319565, -5.000000000000000000 ) ) ;
#25414 = CARTESIAN_POINT ( 'NONE',  ( -82.00000337463094979, -2.404119930384582903E-14, 12.50000000000000000 ) ) ;
#25415 = ORIENTED_EDGE ( 'NONE', *, *, #7122, .F. ) ;
#25416 = CARTESIAN_POINT ( 'NONE',  ( -45.00000000000000711, 5.510910596163090344E-15, -5.000000000000000000 ) ) ;
#25417 = FACE_OUTER_BOUND ( 'NONE', #7734, .T. ) ;
#25418 = FACE_OUTER_BOUND ( 'NONE', #2096, .T. ) ;
#25419 = DIRECTION ( 'NONE',  ( 1.000000000000000000, 0.000000000000000000, 0.000000000000000000 ) ) ;
#25420 = ORIENTED_EDGE ( 'NONE', *, *, #13830, .T. ) ;
#25421 = EDGE_CURVE ( 'NONE', #8381, #34620, #30562, .T. ) ;
#25422 = ORIENTED_EDGE ( 'NONE', *, *, #10917, .T. ) ;
#25423 = VECTOR ( 'NONE', #30156, 1000.000000000000000 ) ;
#25424 = DIRECTION ( 'NONE',  ( 0.000000000000000000, 0.000000000000000000, 1.000000000000000000 ) ) ;
#25425 = DIRECTION ( 'NONE',  ( 0.000000000000000000, 0.000000000000000000, -1.000000000000000000 ) ) ;
#25426 = CIRCLE ( 'NONE', #9246, 2.000000000000001776 ) ;
#25427 = VERTEX_POINT ( 'NONE', #3692 ) ;
#25428 = ORIENTED_EDGE ( 'NONE', *, *, #28365, .T. ) ;
#25429 = DIRECTION ( 'NONE',  ( 1.000000000000000000, 0.000000000000000000, 0.000000000000000000 ) ) ;
#25430 = CARTESIAN_POINT ( 'NONE',  ( -1.332830945733270545, 5.003992386592893915, -0.8603634151101617888 ) ) ;
#25431 = LINE ( 'NONE', #5392, #27367 ) ;
#25432 = VERTEX_POINT ( 'NONE', #15120 ) ;
#25433 = AXIS2_PLACEMENT_3D ( 'NONE', #7661, #18554, #19114 ) ;
#25434 = VECTOR ( 'NONE', #16875, 1000.000000000000114 ) ;
#25435 = ORIENTED_EDGE ( 'NONE', *, *, #1632, .F. ) ;
#25436 = ADVANCED_FACE ( 'NONE', ( #26553 ), #7251, .F. ) ;
#25437 = VECTOR ( 'NONE', #5592, 1000.000000000000000 ) ;
#25438 = DIRECTION ( 'NONE',  ( -1.000000000000000000, 0.000000000000000000, 0.000000000000000000 ) ) ;
#25439 = EDGE_LOOP ( 'NONE', ( #19003, #30937 ) ) ;
#25440 = EDGE_CURVE ( 'NONE', #2698, #6733, #11388, .T. ) ;
#25441 = DIRECTION ( 'NONE',  ( 0.000000000000000000, 0.000000000000000000, 1.000000000000000000 ) ) ;
#25442 = EDGE_LOOP ( 'NONE', ( #15731, #17641, #19258, #6742 ) ) ;
#25443 = FACE_BOUND ( 'NONE', #11492, .T. ) ;
#25444 = EDGE_CURVE ( 'NONE', #28959, #33082, #13184, .T. ) ;
#25445 = CARTESIAN_POINT ( 'NONE',  ( 11.99999662536865763, -69.28203230275519786, -9.999999999999998224 ) ) ;
#25446 = AXIS2_PLACEMENT_3D ( 'NONE', #12275, #299, #34646 ) ;
#25447 = EDGE_CURVE ( 'NONE', #11341, #7750, #8982, .T. ) ;
#25448 = VERTEX_POINT ( 'NONE', #27841 ) ;
#25449 = EDGE_CURVE ( 'NONE', #26021, #33148, #4204, .T. ) ;
#25450 = DIRECTION ( 'NONE',  ( 0.000000000000000000, 0.000000000000000000, 1.000000000000000000 ) ) ;
#25451 = STYLED_ITEM ( 'NONE', ( #16487 ), #32134 ) ;
#25452 = CYLINDRICAL_SURFACE ( 'NONE', #33843, 27.00000000000001421 ) ;
#25453 = CARTESIAN_POINT ( 'NONE',  ( -17.55872235085560007, 89.94802294027088863, 30.49999999999999289 ) ) ;
#25454 = DIRECTION ( 'NONE',  ( 1.000000000000000000, 0.000000000000000000, 0.000000000000000000 ) ) ;
#25455 = EDGE_LOOP ( 'NONE', ( #35580, #330, #25821 ) ) ;
#25456 = CARTESIAN_POINT ( 'NONE',  ( -3.374631289687624047E-06, -69.28203230275519786, -9.999999999999998224 ) ) ;
#25457 = DIRECTION ( 'NONE',  ( -0.000000000000000000, -0.000000000000000000, 1.000000000000000000 ) ) ;
#25458 = DIRECTION ( 'NONE',  ( 1.000000000000000000, 0.000000000000000000, 0.000000000000000000 ) ) ;
#25459 = EDGE_CURVE ( 'NONE', #21147, #7638, #4983, .T. ) ;
#25460 = VECTOR ( 'NONE', #15503, 1000.000000000000000 ) ;
#25461 = AXIS2_PLACEMENT_3D ( 'NONE', #28770, #33546, #18904 ) ;
#25462 = EDGE_CURVE ( 'NONE', #16077, #26898, #1980, .T. ) ;
#25463 = ORIENTED_EDGE ( 'NONE', *, *, #469, .T. ) ;
#25464 = VERTEX_POINT ( 'NONE', #4627 ) ;
#25465 = ADVANCED_FACE ( 'NONE', ( #10067 ), #21676, .T. ) ;
#25467 = EDGE_CURVE ( 'NONE', #12814, #25033, #2408, .T. ) ;
#25466 = EDGE_LOOP ( 'NONE', ( #16528, #9767 ) ) ;
#25468 = CARTESIAN_POINT ( 'NONE',  ( 79.99999662536833966, -3.469446951953614189E-15, -9.999999999999998224 ) ) ;
#25469 = CARTESIAN_POINT ( 'NONE',  ( 93.60231327712337190, 15.97563234535636134, -4.999999999999997335 ) ) ;
#25470 = DIRECTION ( 'NONE',  ( 0.000000000000000000, 0.000000000000000000, 1.000000000000000000 ) ) ;
#25471 = AXIS2_PLACEMENT_3D ( 'NONE', #7974, #11149, #10798 ) ;
#25472 = CARTESIAN_POINT ( 'NONE',  ( -0.8144415599836954955, 5.303284638000461015, -0.2680587191991145590 ) ) ;
#25473 = CARTESIAN_POINT ( 'NONE',  ( 86.78973740846132046, -72.09873635328332853, 32.50000000000000000 ) ) ;
#25474 = CARTESIAN_POINT ( 'NONE',  ( -103.8785218410652647, -60.08491969753902850, 32.50000000000000000 ) ) ;
#25475 = VECTOR ( 'NONE', #30249, 1000.000000000000000 ) ;
#25476 = CARTESIAN_POINT ( 'NONE',  ( -37.00000337463116296, 77.94228634059957983, -9.999999999999998224 ) ) ;
#25477 = CIRCLE ( 'NONE', #23681, 3.000000000000002665 ) ;
#25478 = DIRECTION ( 'NONE',  ( 0.000000000000000000, 0.000000000000000000, 1.000000000000000000 ) ) ;
#25479 = CIRCLE ( 'NONE', #8108, 2.000000000000001776 ) ;
#25480 = ORIENTED_EDGE ( 'NONE', *, *, #21748, .F. ) ;
#25481 = AXIS2_PLACEMENT_3D ( 'NONE', #4654, #27689, #12875 ) ;
#25482 = ORIENTED_EDGE ( 'NONE', *, *, #5032, .F. ) ;
#25483 = FACE_OUTER_BOUND ( 'NONE', #22624, .T. ) ;
#25484 = CARTESIAN_POINT ( 'NONE',  ( 21.99999662536862033, -69.28203230275519786, -9.999999999999998224 ) ) ;
#25485 = DIRECTION ( 'NONE',  ( -1.000000000000000000, 0.000000000000000000, 0.000000000000000000 ) ) ;
#25486 = CARTESIAN_POINT ( 'NONE',  ( -20.00000337463123756, -69.28203230275522628, -9.999999999999998224 ) ) ;
#25487 = ORIENTED_EDGE ( 'NONE', *, *, #32078, .F. ) ;
#25488 = CIRCLE ( 'NONE', #27271, 3.499999999999989342 ) ;
#25489 = AXIS2_PLACEMENT_3D ( 'NONE', #35017, #21131, #17961 ) ;
#25490 = FACE_BOUND ( 'NONE', #19154, .T. ) ;
#25491 = EDGE_LOOP ( 'NONE', ( #29429, #19801, #4236, #8045, #2389 ) ) ;
#25492 = ORIENTED_EDGE ( 'NONE', *, *, #7815, .F. ) ;
#25493 = LINE ( 'NONE', #33754, #14802 ) ;
#25494 = ORIENTED_EDGE ( 'NONE', *, *, #30481, .T. ) ;
#25495 =( LENGTH_UNIT ( ) NAMED_UNIT ( * ) SI_UNIT ( .MILLI., .METRE. ) );
#25496 = LINE ( 'NONE', #2261, #23184 ) ;
#25497 = CYLINDRICAL_SURFACE ( 'NONE', #20043, 2.000000000000001776 ) ;
#25498 = AXIS2_PLACEMENT_3D ( 'NONE', #31004, #11315, #33815 ) ;
#25499 = CARTESIAN_POINT ( 'NONE',  ( -73.00000337463097821, 8.660254037844374864, -5.000000000000000000 ) ) ;
#25500 = EDGE_LOOP ( 'NONE', ( #9880, #14303 ) ) ;
#25501 = AXIS2_PLACEMENT_3D ( 'NONE', #36598, #33968, #27955 ) ;
#25502 = VERTEX_POINT ( 'NONE', #30664 ) ;
#25503 = AXIS2_PLACEMENT_3D ( 'NONE', #20222, #11761, #23578 ) ;
#25504 = AXIS2_PLACEMENT_3D ( 'NONE', #9387, #18019, #29441 ) ;
#25505 = ORIENTED_EDGE ( 'NONE', *, *, #29918, .F. ) ;
#25506 = AXIS2_PLACEMENT_3D ( 'NONE', #24491, #19400, #5155 ) ;
#25507 = EDGE_CURVE ( 'NONE', #26995, #1512, #29938, .T. ) ;
#25508 = ORIENTED_EDGE ( 'NONE', *, *, #21686, .T. ) ;
#25509 = AXIS2_PLACEMENT_3D ( 'NONE', #6313, #2774, #8956 ) ;
#25510 = ORIENTED_EDGE ( 'NONE', *, *, #855, .F. ) ;
#25511 = EDGE_CURVE ( 'NONE', #1584, #34250, #27494, .T. ) ;
#25512 = CARTESIAN_POINT ( 'NONE',  ( -63.00000337463104927, -43.30127018922202353, -9.999999999999998224 ) ) ;
#25513 = ADVANCED_FACE ( 'NONE', ( #7813, #10247, #19249, #19069, #16251, #16420, #12669, #9861, #21301 ), #18868, .F. ) ;
#25514 = DIRECTION ( 'NONE',  ( 0.000000000000000000, 0.000000000000000000, -1.000000000000000000 ) ) ;
#25515 = CARTESIAN_POINT ( 'NONE',  ( 31.99999662536857770, -69.28203230275519786, -9.999999999999998224 ) ) ;
#25516 = FACE_OUTER_BOUND ( 'NONE', #17796, .T. ) ;
#25517 = ORIENTED_EDGE ( 'NONE', *, *, #3511, .F. ) ;
#25518 = DIRECTION ( 'NONE',  ( 0.000000000000000000, 0.000000000000000000, 1.000000000000000000 ) ) ;
#25519 = AXIS2_PLACEMENT_3D ( 'NONE', #10239, #35935, #24287 ) ;
#25520 = DIRECTION ( 'NONE',  ( 1.000000000000000000, 0.000000000000000000, 0.000000000000000000 ) ) ;
#25521 = DIRECTION ( 'NONE',  ( 0.000000000000000000, 0.000000000000000000, 1.000000000000000000 ) ) ;
#25522 = ORIENTED_EDGE ( 'NONE', *, *, #32675, .T. ) ;
#25523 = CARTESIAN_POINT ( 'NONE',  ( -3.000000000000000000, 0.000000000000000000, -5.974599999999999689 ) ) ;
#25524 = FACE_OUTER_BOUND ( 'NONE', #25949, .T. ) ;
#25525 = VERTEX_POINT ( 'NONE', #7067 ) ;
#25526 = AXIS2_PLACEMENT_3D ( 'NONE', #18076, #8907, #9649 ) ;
#25527 = ORIENTED_EDGE ( 'NONE', *, *, #27978, .T. ) ;
#25528 = DIRECTION ( 'NONE',  ( -0.7650473262243671080, -0.6439740589782688707, -0.000000000000000000 ) ) ;
#25529 = VECTOR ( 'NONE', #33600, 1000.000000000000000 ) ;
#25530 = CARTESIAN_POINT ( 'NONE',  ( 37.50000000000000000, -103.4105893997321743, 27.50000000000000000 ) ) ;
#25531 = DIRECTION ( 'NONE',  ( 0.000000000000000000, 0.000000000000000000, 1.000000000000000000 ) ) ;
#25532 = CYLINDRICAL_SURFACE ( 'NONE', #17881, 2.000000000000001776 ) ;
#25533 =( GEOMETRIC_REPRESENTATION_CONTEXT ( 3 ) GLOBAL_UNCERTAINTY_ASSIGNED_CONTEXT ( ( #8053 ) ) GLOBAL_UNIT_ASSIGNED_CONTEXT ( ( #16328, #7330, #3168 ) ) REPRESENTATION_CONTEXT ( 'NONE', 'WORKASPACE' ) );
#25534 = VERTEX_POINT ( 'NONE', #1425 ) ;
#25535 = VERTEX_POINT ( 'NONE', #30495 ) ;
#25536 = CIRCLE ( 'NONE', #9353, 1.999999999999998224 ) ;
#25537 = CIRCLE ( 'NONE', #30318, 2.000000000000001776 ) ;
#25538 = EDGE_CURVE ( 'NONE', #18383, #12647, #34743, .T. ) ;
#25539 = AXIS2_PLACEMENT_3D ( 'NONE', #4182, #35671, #32654 ) ;
#25540 = FACE_OUTER_BOUND ( 'NONE', #8265, .T. ) ;
#25541 = AXIS2_PLACEMENT_3D ( 'NONE', #23012, #28443, #14399 ) ;
#25542 = ORIENTED_EDGE ( 'NONE', *, *, #12613, .T. ) ;
#25543 = CARTESIAN_POINT ( 'NONE',  ( -5.000000000000000000, 2.886751345948137981, -5.553418012614792509 ) ) ;
#25544 = ORIENTED_EDGE ( 'NONE', *, *, #7196, .F. ) ;
#25545 = DIRECTION ( 'NONE',  ( 1.000000000000000000, 0.000000000000000000, 0.000000000000000000 ) ) ;
#25546 = AXIS2_PLACEMENT_3D ( 'NONE', #10196, #21058, #12614 ) ;
#25547 = CARTESIAN_POINT ( 'NONE',  ( 3.000000000000000000, -2.201436576420045643, -1.270999999999998575 ) ) ;
#25548 = CARTESIAN_POINT ( 'NONE',  ( 72.99999662536835388, -43.30127018922199511, 17.49999999999999645 ) ) ;
#25549 = CARTESIAN_POINT ( 'NONE',  ( 66.99999662536841072, 25.98076211353318854, -5.000000000000000000 ) ) ;
#25550 = VERTEX_POINT ( 'NONE', #35754 ) ;
#25551 = ORIENTED_EDGE ( 'NONE', *, *, #30701, .T. ) ;
#25552 = DIRECTION ( 'NONE',  ( 1.000000000000000000, 0.000000000000000000, 0.000000000000000000 ) ) ;
#25553 = CARTESIAN_POINT ( 'NONE',  ( 67.99999662536838230, 34.64101615137758472, -5.000000000000000000 ) ) ;
#25554 = AXIS2_PLACEMENT_3D ( 'NONE', #2119, #16376, #13755 ) ;
#25555 = CARTESIAN_POINT ( 'NONE',  ( 0.3000000000000016542, 0.000000000000000000, 0.000000000000000000 ) ) ;
#25556 = CARTESIAN_POINT ( 'NONE',  ( -10.00000337463128730, 69.28203230275516944, -9.999999999999998224 ) ) ;
#25557 = AXIS2_PLACEMENT_3D ( 'NONE', #22667, #34800, #22117 ) ;
#25558 = EDGE_LOOP ( 'NONE', ( #28126, #2719, #3701, #35761 ) ) ;
#25559 = CYLINDRICAL_SURFACE ( 'NONE', #25554, 95.00000000000001421 ) ;
#25560 = EDGE_CURVE ( 'NONE', #23471, #31151, #4819, .T. ) ;
#25561 = FACE_BOUND ( 'NONE', #8312, .T. ) ;
#25562 = AXIS2_PLACEMENT_3D ( 'NONE', #30142, #4470, #10279 ) ;
#25563 = DIRECTION ( 'NONE',  ( 0.000000000000000000, 0.000000000000000000, -1.000000000000000000 ) ) ;
#25564 = FACE_OUTER_BOUND ( 'NONE', #28575, .T. ) ;
#25565 = CARTESIAN_POINT ( 'NONE',  ( 0.000000000000000000, 0.000000000000000000, -5.000000000000000000 ) ) ;
#25566 = AXIS2_PLACEMENT_3D ( 'NONE', #10980, #5187, #103 ) ;
#25567 = FACE_OUTER_BOUND ( 'NONE', #19420, .T. ) ;
#25568 = AXIS2_PLACEMENT_3D ( 'NONE', #28867, #25887, #20812 ) ;
#25569 = AXIS2_PLACEMENT_3D ( 'NONE', #2380, #13411, #16257 ) ;
#25570 = CARTESIAN_POINT ( 'NONE',  ( -2.545082869045428353, 120.0000000191570990, 27.49998800000000188 ) ) ;
#25571 = CARTESIAN_POINT ( 'NONE',  ( 4.999999999999999112, -8.890457814381136359E-15, -3.620524600599876575 ) ) ;
#25572 = ORIENTED_EDGE ( 'NONE', *, *, #28591, .T. ) ;
#25573 = CYLINDRICAL_SURFACE ( 'NONE', #25043, 30.00000000000000000 ) ;
#25574 = DIRECTION ( 'NONE',  ( -0.000000000000000000, -0.000000000000000000, 1.000000000000000000 ) ) ;
#25575 = DIRECTION ( 'NONE',  ( -0.000000000000000000, -0.000000000000000000, 1.000000000000000000 ) ) ;
#25576 = ORIENTED_EDGE ( 'NONE', *, *, #28846, .T. ) ;
#25577 = CIRCLE ( 'NONE', #30355, 33.00000000000001421 ) ;
#25578 = VERTEX_POINT ( 'NONE', #24509 ) ;
#25579 = ORIENTED_EDGE ( 'NONE', *, *, #15861, .F. ) ;
#25580 = ADVANCED_FACE ( 'NONE', ( #35950 ), #13608, .F. ) ;
#25581 = CARTESIAN_POINT ( 'NONE',  ( -65.00000337463102085, 43.30127018922198801, 17.49999999999999645 ) ) ;
#25582 = DIRECTION ( 'NONE',  ( 1.000000000000000000, 0.000000000000000000, 0.000000000000000000 ) ) ;
#25583 = ORIENTED_EDGE ( 'NONE', *, *, #26774, .F. ) ;
#25584 = AXIS2_PLACEMENT_3D ( 'NONE', #24128, #24514, #35955 ) ;
#25586 = ADVANCED_FACE ( 'NONE', ( #5542 ), #33675, .F. ) ;
#25585 = AXIS2_PLACEMENT_3D ( 'NONE', #30316, #12869, #29954 ) ;
#25587 = AXIS2_PLACEMENT_3D ( 'NONE', #33025, #6963, #4729 ) ;
#25588 = LINE ( 'NONE', #34771, #524 ) ;
#25589 = CIRCLE ( 'NONE', #9407, 2.000000000000000000 ) ;
#25590 = ORIENTED_EDGE ( 'NONE', *, *, #25271, .T. ) ;
#25591 = DIRECTION ( 'NONE',  ( 0.8660254037844415942, 0.4999999999999949485, 0.000000000000000000 ) ) ;
#25592 = EDGE_CURVE ( 'NONE', #15444, #34250, #32345, .T. ) ;
#25593 = ORIENTED_EDGE ( 'NONE', *, *, #9041, .F. ) ;
#25594 = FACE_OUTER_BOUND ( 'NONE', #30270, .T. ) ;
#25595 = B_SPLINE_CURVE_WITH_KNOTS ( 'NONE', 3,
 ( #3400, #9586, #9025, #9386, #15022, #12367, #23836, #31866 ),
 .UNSPECIFIED., .F., .F.,
 ( 4, 2, 2, 4 ),
 ( 0.007260997678543244099, 0.007995810154593281649, 0.008730622630643319199, 0.01020024758274339430 ),
 .UNSPECIFIED. ) ;
#25596 = ORIENTED_EDGE ( 'NONE', *, *, #30556, .T. ) ;
#25597 = CIRCLE ( 'NONE', #22003, 2.000000000000000000 ) ;
#25598 = ORIENTED_EDGE ( 'NONE', *, *, #1873, .F. ) ;
#25599 = AXIS2_PLACEMENT_3D ( 'NONE', #20609, #35069, #3193 ) ;
#25600 = CIRCLE ( 'NONE', #27383, 3.000000000000007994 ) ;
#25601 = EDGE_CURVE ( 'NONE', #33109, #12497, #3604, .T. ) ;
#25602 = DIRECTION ( 'NONE',  ( 1.000000000000000000, 0.000000000000000000, 0.000000000000000000 ) ) ;
#25603 = CARTESIAN_POINT ( 'NONE',  ( 58.88972745734226066, 33.99999999999924682, -4.999999999999997335 ) ) ;
#25604 = EDGE_LOOP ( 'NONE', ( #22548, #216, #16546, #20288, #18813, #18048 ) ) ;
#25605 = PLANE ( 'NONE',  #26670 ) ;
#25606 = VECTOR ( 'NONE', #13969, 1000.000000000000000 ) ;
#25607 = CONTEXT_DEPENDENT_SHAPE_REPRESENTATION ( #24759, #35250 ) ;
#25608 = LINE ( 'NONE', #10800, #16494 ) ;
#25609 = CARTESIAN_POINT ( 'NONE',  ( 16.99999662536863454, -77.94228634059960825, -9.999999999999998224 ) ) ;
#25610 = ORIENTED_EDGE ( 'NONE', *, *, #15145, .T. ) ;
#25611 = DIRECTION ( 'NONE',  ( 0.000000000000000000, 0.000000000000000000, 1.000000000000000000 ) ) ;
#25613 = DIRECTION ( 'NONE',  ( 0.000000000000000000, 0.000000000000000000, 1.000000000000000000 ) ) ;
#25612 = CIRCLE ( 'NONE', #2263, 2.000000000000001776 ) ;
#25614 = EDGE_LOOP ( 'NONE', ( #15216, #22347, #18476, #34590 ) ) ;
#25615 = ADVANCED_FACE ( 'NONE', ( #19971 ), #36848, .F. ) ;
#25616 = CARTESIAN_POINT ( 'NONE',  ( -73.00000337463097821, 25.98076211353318854, -5.000000000000000000 ) ) ;
#25617 = AXIS2_PLACEMENT_3D ( 'NONE', #5944, #20177, #31605 ) ;
#25618 = VECTOR ( 'NONE', #1769, 1000.000000000000000 ) ;
#25619 = CARTESIAN_POINT ( 'NONE',  ( 0.000000000000000000, 2.935248768560057453, -3.903127820947815962E-15 ) ) ;
#25620 = DIRECTION ( 'NONE',  ( 1.000000000000000000, 0.000000000000000000, 0.000000000000000000 ) ) ;
#25622 = AXIS2_PLACEMENT_3D ( 'NONE', #5497, #2876, #23296 ) ;
#25621 = DIRECTION ( 'NONE',  ( 0.000000000000000000, 0.000000000000000000, 1.000000000000000000 ) ) ;
#25623 = VERTEX_POINT ( 'NONE', #25413 ) ;
#25624 = AXIS2_PLACEMENT_3D ( 'NONE', #24049, #23667, #34926 ) ;
#25625 = ORIENTED_EDGE ( 'NONE', *, *, #35966, .F. ) ;
#25626 = FACE_OUTER_BOUND ( 'NONE', #21245, .T. ) ;
#25627 = DIRECTION ( 'NONE',  ( 0.000000000000000000, 0.000000000000000000, 1.000000000000000000 ) ) ;
#25628 = EDGE_CURVE ( 'NONE', #25733, #20787, #5408, .T. ) ;
#25629 = CIRCLE ( 'NONE', #15419, 5.000000000000000000 ) ;
#25630 = VECTOR ( 'NONE', #26885, 1000.000000000000000 ) ;
#25631 = VERTEX_POINT ( 'NONE', #28394 ) ;
#25632 = ORIENTED_EDGE ( 'NONE', *, *, #14156, .T. ) ;
#25633 = EDGE_CURVE ( 'NONE', #30803, #14051, #10195, .T. ) ;
#25634 = FACE_OUTER_BOUND ( 'NONE', #35536, .T. ) ;
#25635 = DIRECTION ( 'NONE',  ( 1.000000000000000000, 0.000000000000000000, 0.000000000000000000 ) ) ;
#25636 = LINE ( 'NONE', #28415, #17051 ) ;
#25637 = EDGE_LOOP ( 'NONE', ( #2822, #23601 ) ) ;
#25638 = EDGE_CURVE ( 'NONE', #26476, #30547, #16810, .T. ) ;
#25639 = ORIENTED_EDGE ( 'NONE', *, *, #31286, .F. ) ;
#25640 = CARTESIAN_POINT ( 'NONE',  ( 72.99999662536836809, 25.98076211353319565, -9.999999999999998224 ) ) ;
#25641 = CIRCLE ( 'NONE', #9469, 27.00000000000001421 ) ;
#25642 = CARTESIAN_POINT ( 'NONE',  ( 47.63139720814418610, 27.49999999999988987, -10.00000000000000000 ) ) ;
#25643 = ORIENTED_EDGE ( 'NONE', *, *, #35554, .T. ) ;
#25644 = CARTESIAN_POINT ( 'NONE',  ( 0.000000000000000000, 0.000000000000000000, 27.50000000000000000 ) ) ;
#25645 = EDGE_CURVE ( 'NONE', #23444, #13165, #35954, .T. ) ;
#25646 = ORIENTED_EDGE ( 'NONE', *, *, #7594, .F. ) ;
#25647 = CIRCLE ( 'NONE', #5888, 2.000000000000000000 ) ;
#25648 = CIRCLE ( 'NONE', #26808, 2.000000000000001776 ) ;
#25649 = FACE_BOUND ( 'NONE', #5262, .T. ) ;
#25650 = AXIS2_PLACEMENT_3D ( 'NONE', #7256, #36122, #6868 ) ;
#25651 = EDGE_CURVE ( 'NONE', #34636, #22817, #34157, .T. ) ;
#25652 = AXIS2_PLACEMENT_3D ( 'NONE', #11612, #28507, #36969 ) ;
#25653 = CARTESIAN_POINT ( 'NONE',  ( 102.5304832720496080, 102.5304832720492527, 32.55002500000000509 ) ) ;
#25654 = CARTESIAN_POINT ( 'NONE',  ( -18.00000337463123046, 86.60254037844397601, -9.999999999999998224 ) ) ;
#25655 = ORIENTED_EDGE ( 'NONE', *, *, #121, .F. ) ;
#25656 = DIRECTION ( 'NONE',  ( 1.000000000000000000, 0.000000000000000000, 0.000000000000000000 ) ) ;
#25657 = CARTESIAN_POINT ( 'NONE',  ( -27.78182860042817026, -56.67878100130359087, -49.86348611802629449 ) ) ;
#25658 = VECTOR ( 'NONE', #10863, 1000.000000000000000 ) ;
#25659 = CARTESIAN_POINT ( 'NONE',  ( 0.000000000000000000, 0.000000000000000000, 12.49999999999999822 ) ) ;
#25660 = FACE_OUTER_BOUND ( 'NONE', #11657, .T. ) ;
#25661 = ORIENTED_EDGE ( 'NONE', *, *, #36488, .T. ) ;
#25662 = CYLINDRICAL_SURFACE ( 'NONE', #20849, 2.000000000000000000 ) ;
#25663 = DIRECTION ( 'NONE',  ( 1.000000000000000000, 0.000000000000000000, 0.000000000000000000 ) ) ;
#25664 = CARTESIAN_POINT ( 'NONE',  ( 81.99999662536833966, 17.32050807568879236, 17.49999999999999645 ) ) ;
#25665 = ORIENTED_EDGE ( 'NONE', *, *, #30818, .F. ) ;
#25666 = EDGE_CURVE ( 'NONE', #19051, #17303, #1560, .T. ) ;
#25667 = ORIENTED_EDGE ( 'NONE', *, *, #7377, .T. ) ;
#25668 = AXIS2_PLACEMENT_3D ( 'NONE', #28299, #22696, #34145 ) ;
#25669 = ORIENTED_EDGE ( 'NONE', *, *, #15925, .F. ) ;
#25670 = CARTESIAN_POINT ( 'NONE',  ( 51.99999662536847467, -69.28203230275519786, 17.49999999999999645 ) ) ;
#25671 = CIRCLE ( 'NONE', #36958, 2.000000000000001776 ) ;
#25672 = EDGE_CURVE ( 'NONE', #24561, #33879, #20719, .T. ) ;
#25673 = PLANE ( 'NONE',  #24617 ) ;
#25674 = AXIS2_PLACEMENT_3D ( 'NONE', #36562, #8038, #20023 ) ;
#25675 = CARTESIAN_POINT ( 'NONE',  ( -2.069940739436584298, 4.578421848775973579, -1.448426339804853087E-16 ) ) ;
#25676 = ADVANCED_FACE ( 'NONE', ( #8171 ), #31224, .F. ) ;
#25677 = CARTESIAN_POINT ( 'NONE',  ( 107.1783900501392139, -49.76387890855416885, 32.50000000000000711 ) ) ;
#25678 = CARTESIAN_POINT ( 'NONE',  ( -82.47367650156751040, -72.51972198845571427, 32.50000000000000711 ) ) ;
#25679 = EDGE_CURVE ( 'NONE', #23569, #33068, #20112, .T. ) ;
#25680 = CARTESIAN_POINT ( 'NONE',  ( 71.99999662536838230, -51.96152422706639840, -9.999999999999998224 ) ) ;
#25681 = DIRECTION ( 'NONE',  ( 3.469446951953612611E-15, 1.000000000000000000, 0.000000000000000000 ) ) ;
#25682 = ORIENTED_EDGE ( 'NONE', *, *, #10293, .F. ) ;
#25683 = ORIENTED_EDGE ( 'NONE', *, *, #27190, .F. ) ;
#25684 = AXIS2_PLACEMENT_3D ( 'NONE', #1563, #4575, #2117 ) ;
#25685 = CARTESIAN_POINT ( 'NONE',  ( 3.050000000000000711, 0.000000000000000000, 2.266666666666999674 ) ) ;
#25686 = DIRECTION ( 'NONE',  ( -1.000000000000000000, 0.000000000000000000, 0.000000000000000000 ) ) ;
#25687 = DIRECTION ( 'NONE',  ( 1.000000000000000000, 0.000000000000000000, 0.000000000000000000 ) ) ;
#25688 = DIRECTION ( 'NONE',  ( 0.000000000000000000, 0.000000000000000000, 1.000000000000000000 ) ) ;
#25689 = ORIENTED_EDGE ( 'NONE', *, *, #1840, .T. ) ;
#25690 = ADVANCED_FACE ( 'NONE', ( #25801 ), #93, .F. ) ;
#25691 = FACE_BOUND ( 'NONE', #18912, .T. ) ;
#25692 = CIRCLE ( 'NONE', #1753, 2.000000000000001776 ) ;
#25693 = EDGE_LOOP ( 'NONE', ( #19289, #13187 ) ) ;
#25694 = ORIENTED_EDGE ( 'NONE', *, *, #19768, .T. ) ;
#25695 = CARTESIAN_POINT ( 'NONE',  ( 62.19434990244977257, -52.39915983220758022, 12.49999999999999822 ) ) ;
#25696 = VERTEX_POINT ( 'NONE', #8368 ) ;
#25697 = LINE ( 'NONE', #19325, #5230 ) ;
#25698 = DIRECTION ( 'NONE',  ( 0.000000000000000000, 0.000000000000000000, 1.000000000000000000 ) ) ;
#25699 = CARTESIAN_POINT ( 'NONE',  ( 47.99999662536848177, -51.96152422706640550, -5.000000000000000000 ) ) ;
#25700 = AXIS2_PLACEMENT_3D ( 'NONE', #14509, #632, #25947 ) ;
#25701 = ORIENTED_EDGE ( 'NONE', *, *, #36244, .T. ) ;
#25702 = EDGE_LOOP ( 'NONE', ( #31879, #24511, #14091 ) ) ;
#25703 = CIRCLE ( 'NONE', #29269, 33.00000000000001421 ) ;
#25704 = ORIENTED_EDGE ( 'NONE', *, *, #25462, .T. ) ;
#25705 = VERTEX_POINT ( 'NONE', #16970 ) ;
#25706 = CIRCLE ( 'NONE', #9533, 2.000000000000001776 ) ;
#25707 = EDGE_CURVE ( 'NONE', #12497, #20479, #27307, .T. ) ;
#25708 = ORIENTED_EDGE ( 'NONE', *, *, #8399, .F. ) ;
#25709 = CARTESIAN_POINT ( 'NONE',  ( -35.83991598322101879, -56.52018970185248037, -4.999999999999997335 ) ) ;
#25710 = DIRECTION ( 'NONE',  ( 1.000000000000000000, 0.000000000000000000, 0.000000000000000000 ) ) ;
#25711 = EDGE_CURVE ( 'NONE', #6793, #14173, #15945, .T. ) ;
#25712 = DIRECTION ( 'NONE',  ( 0.000000000000000000, 0.000000000000000000, -1.000000000000000000 ) ) ;
#25713 = DIRECTION ( 'NONE',  ( 0.000000000000000000, 0.000000000000000000, 1.000000000000000000 ) ) ;
#25714 = CARTESIAN_POINT ( 'NONE',  ( 4.999999999999998224, -3.082650397928314856, -4.288940341510108389 ) ) ;
#25715 = ORIENTED_EDGE ( 'NONE', *, *, #5056, .T. ) ;
#25716 = CARTESIAN_POINT ( 'NONE',  ( 62.99999662536841072, -25.98076211353320275, -9.999999999999998224 ) ) ;
#25717 = EDGE_CURVE ( 'NONE', #8910, #8894, #29679, .T. ) ;
#25718 = CARTESIAN_POINT ( 'NONE',  ( -65.00000337463104927, -25.98076211353322051, -5.000000000000000000 ) ) ;
#25719 = AXIS2_PLACEMENT_3D ( 'NONE', #24510, #9511, #15688 ) ;
#25720 = CYLINDRICAL_SURFACE ( 'NONE', #21176, 2.000000000000001776 ) ;
#25721 = ORIENTED_EDGE ( 'NONE', *, *, #15748, .F. ) ;
#25722 = DIRECTION ( 'NONE',  ( -0.000000000000000000, -0.8660254037844414832, -0.4999999999999953371 ) ) ;
#25723 = ADVANCED_FACE ( 'NONE', ( #457 ), #25965, .F. ) ;
#25724 = DIRECTION ( 'NONE',  ( 1.000000000000000000, 0.000000000000000000, 0.000000000000000000 ) ) ;
#25725 = ADVANCED_FACE ( 'NONE', ( #3821 ), #32128, .F. ) ;
#25726 = ORIENTED_EDGE ( 'NONE', *, *, #13044, .T. ) ;
#25727 = EDGE_LOOP ( 'NONE', ( #11375, #27872 ) ) ;
#25728 = DIRECTION ( 'NONE',  ( 1.000000000000000000, 0.000000000000000000, 0.000000000000000000 ) ) ;
#25729 = DIRECTION ( 'NONE',  ( 0.000000000000000000, 0.000000000000000000, -1.000000000000000000 ) ) ;
#25730 = DIRECTION ( 'NONE',  ( -1.000000000000000000, 0.000000000000000000, 0.000000000000000000 ) ) ;
#25731 = FACE_OUTER_BOUND ( 'NONE', #5118, .T. ) ;
#25732 = ORIENTED_EDGE ( 'NONE', *, *, #22714, .F. ) ;
#25733 = VERTEX_POINT ( 'NONE', #266 ) ;
#25734 = AXIS2_PLACEMENT_3D ( 'NONE', #35392, #9498, #26181 ) ;
#25735 = EDGE_CURVE ( 'NONE', #25705, #11344, #28510, .T. ) ;
#25736 = CYLINDRICAL_SURFACE ( 'NONE', #35665, 2.000000000000001776 ) ;
#25737 = ADVANCED_FACE ( 'NONE', ( #9467 ), #6267, .F. ) ;
#25738 = CARTESIAN_POINT ( 'NONE',  ( 5.000000000000000000, -0.9724665692850895660, -5.958069561147902427 ) ) ;
#25739 = AXIS2_PLACEMENT_3D ( 'NONE', #27281, #2155, #24290 ) ;
#25740 = EDGE_CURVE ( 'NONE', #25696, #5023, #3100, .T. ) ;
#25741 = VERTEX_POINT ( 'NONE', #34606 ) ;
#25742 = EDGE_CURVE ( 'NONE', #13541, #12539, #2776, .T. ) ;
#25743 = PLANE ( 'NONE',  #32737 ) ;
#25744 = CIRCLE ( 'NONE', #14969, 95.00000000000000000 ) ;
#25745 = ORIENTED_EDGE ( 'NONE', *, *, #8694, .F. ) ;
#25746 = DIRECTION ( 'NONE',  ( 0.000000000000000000, 0.000000000000000000, 1.000000000000000000 ) ) ;
#25747 = DIRECTION ( 'NONE',  ( -1.000000000000000000, 0.000000000000000000, 0.000000000000000000 ) ) ;
#25748 = CYLINDRICAL_SURFACE ( 'NONE', #5290, 33.00000000000001421 ) ;
#25749 = CIRCLE ( 'NONE', #35338, 25.00000000000000000 ) ;
#25750 = CARTESIAN_POINT ( 'NONE',  ( 0.000000000000000000, 0.000000000000000000, 12.49999999999999822 ) ) ;
#25751 = VERTEX_POINT ( 'NONE', #20344 ) ;
#25752 = ORIENTED_EDGE ( 'NONE', *, *, #35928, .F. ) ;
#25753 = CARTESIAN_POINT ( 'NONE',  ( 71.99999662536839651, 17.32050807568879236, 17.49999999999999645 ) ) ;
#25754 = VECTOR ( 'NONE', #27889, 1000.000000000000000 ) ;
#25755 = CARTESIAN_POINT ( 'NONE',  ( 0.000000000000000000, 0.000000000000000000, -5.000000000000000000 ) ) ;
#25756 = FACE_OUTER_BOUND ( 'NONE', #26887, .T. ) ;
#25757 = LINE ( 'NONE', #2499, #32874 ) ;
#25758 = ORIENTED_EDGE ( 'NONE', *, *, #14371, .T. ) ;
#25759 = CARTESIAN_POINT ( 'NONE',  ( -89.42901512340354486, 31.83425564451495404, -49.86348611802629449 ) ) ;
#25760 = FACE_BOUND ( 'NONE', #7723, .T. ) ;
#25761 = LINE ( 'NONE', #608, #19615 ) ;
#25762 = CARTESIAN_POINT ( 'NONE',  ( 54.99999662536844625, 60.62177826491077326, 17.49999999999999645 ) ) ;
#25763 = PLANE ( 'NONE',  #28483 ) ;
#25764 = AXIS2_PLACEMENT_3D ( 'NONE', #31563, #20136, #2150 ) ;
#25765 = EDGE_CURVE ( 'NONE', #6989, #10733, #6345, .T. ) ;
#25766 = CARTESIAN_POINT ( 'NONE',  ( 5.238715782502660900, -1.018209582082221454, -4.086015505371661583 ) ) ;
#25767 = DIRECTION ( 'NONE',  ( 0.000000000000000000, 0.000000000000000000, 1.000000000000000000 ) ) ;
#25768 = AXIS2_PLACEMENT_3D ( 'NONE', #30801, #10578, #16576 ) ;
#25769 = CYLINDRICAL_SURFACE ( 'NONE', #10393, 2.000000000000001776 ) ;
#25770 = VERTEX_POINT ( 'NONE', #21072 ) ;
#25771 = DIRECTION ( 'NONE',  ( -0.000000000000000000, -0.000000000000000000, 1.000000000000000000 ) ) ;
#25772 = LINE ( 'NONE', #30805, #32060 ) ;
#25773 = AXIS2_PLACEMENT_3D ( 'NONE', #20991, #7121, #18568 ) ;
#25774 = DIRECTION ( 'NONE',  ( 0.000000000000000000, 0.000000000000000000, 1.000000000000000000 ) ) ;
#25775 = ORIENTED_EDGE ( 'NONE', *, *, #16968, .T. ) ;
#25776 = VERTEX_POINT ( 'NONE', #23909 ) ;
#25777 = VERTEX_POINT ( 'NONE', #26513 ) ;
#25778 = CARTESIAN_POINT ( 'NONE',  ( -124.4080600076929954, 12.15049814296761888, 27.50000000000000000 ) ) ;
#25779 = DIRECTION ( 'NONE',  ( 0.000000000000000000, 0.000000000000000000, 1.000000000000000000 ) ) ;
#25780 = DIRECTION ( 'NONE',  ( 0.000000000000000000, 0.000000000000000000, 1.000000000000000000 ) ) ;
#25781 = ORIENTED_EDGE ( 'NONE', *, *, #1219, .F. ) ;
#25782 = CARTESIAN_POINT ( 'NONE',  ( -35.00000337463116296, 77.94228634059957983, 12.50000000000000000 ) ) ;
#25783 = ORIENTED_EDGE ( 'NONE', *, *, #2128, .T. ) ;
#25784 = EDGE_CURVE ( 'NONE', #17257, #695, #12323, .T. ) ;
#25785 = AXIS2_PLACEMENT_3D ( 'NONE', #14667, #11661, #22774 ) ;
#25786 = LINE ( 'NONE', #25051, #31126 ) ;
#25787 = VERTEX_POINT ( 'NONE', #6092 ) ;
#25788 = CARTESIAN_POINT ( 'NONE',  ( -85.00000337463092137, 8.660254037844389075, -5.000000000000000000 ) ) ;
#25789 = ORIENTED_EDGE ( 'NONE', *, *, #32835, .F. ) ;
#25790 = ORIENTED_EDGE ( 'NONE', *, *, #30676, .F. ) ;
#25791 = CARTESIAN_POINT ( 'NONE',  ( -23.00000337463121980, -77.94228634059963667, -9.999999999999998224 ) ) ;
#25793 = CIRCLE ( 'NONE', #9614, 2.000000000000001776 ) ;
#25792 = CARTESIAN_POINT ( 'NONE',  ( 64.99999662536839651, -60.62177826491080168, -9.999999999999998224 ) ) ;
#25794 = ORIENTED_EDGE ( 'NONE', *, *, #29752, .F. ) ;
#25795 = CARTESIAN_POINT ( 'NONE',  ( -94.55012560584690107, -9.234378588653415321, 27.50000000000000000 ) ) ;
#25796 = AXIS2_PLACEMENT_3D ( 'NONE', #13209, #10383, #27633 ) ;
#25797 = ITEM_DEFINED_TRANSFORMATION ( 'NONE', 'NONE', #19568,  #21385 ) ;
#25798 = CARTESIAN_POINT ( 'NONE',  ( 64.99999662536839651, -60.62177826491080168, -9.999999999999998224 ) ) ;
#25799 = CARTESIAN_POINT ( 'NONE',  ( 2.143131898507887033E-16, 80.41276890242660613, -28.48445554337708785 ) ) ;
#25800 = ORIENTED_EDGE ( 'NONE', *, *, #9684, .T. ) ;
#25801 = FACE_OUTER_BOUND ( 'NONE', #798, .T. ) ;
#25802 = CARTESIAN_POINT ( 'NONE',  ( -13.00000337463126066, 77.94228634059957983, -5.000000000000000000 ) ) ;
#25803 = ORIENTED_EDGE ( 'NONE', *, *, #16747, .F. ) ;
#25804 = CARTESIAN_POINT ( 'NONE',  ( -15.00000337463125710, -77.94228634059960825, -9.999999999999998224 ) ) ;
#25805 = DIRECTION ( 'NONE',  ( 0.000000000000000000, 0.000000000000000000, 1.000000000000000000 ) ) ;
#25806 = FACE_OUTER_BOUND ( 'NONE', #22816, .T. ) ;
#25807 = ADVANCED_FACE ( 'NONE', ( #28778 ), #17518, .F. ) ;
#25808 = EDGE_CURVE ( 'NONE', #126, #2266, #33316, .T. ) ;
#25809 = LINE ( 'NONE', #3109, #36240 ) ;
#25810 = VERTEX_POINT ( 'NONE', #35162 ) ;
#25811 = EDGE_CURVE ( 'NONE', #520, #10163, #20901, .T. ) ;
#25812 = DIRECTION ( 'NONE',  ( 0.000000000000000000, 0.000000000000000000, 1.000000000000000000 ) ) ;
#25813 = CARTESIAN_POINT ( 'NONE',  ( 2.500000000000005773, 4.330127018922191873, -6.000000000000000000 ) ) ;
#25815 = ORIENTED_EDGE ( 'NONE', *, *, #6707, .T. ) ;
#25814 = EDGE_CURVE ( 'NONE', #21946, #32590, #23735, .T. ) ;
#25816 = ORIENTED_EDGE ( 'NONE', *, *, #20194, .F. ) ;
#25817 = VECTOR ( 'NONE', #11566, 999.9999999999998863 ) ;
#25818 = CARTESIAN_POINT ( 'NONE',  ( 89.99999662536828282, 0.000000000000000000, -9.999999999999998224 ) ) ;
#25819 = CARTESIAN_POINT ( 'NONE',  ( -57.00000337463109901, -60.62177826491083010, -9.999999999999998224 ) ) ;
#25820 = CARTESIAN_POINT ( 'NONE',  ( -87.00000337463093558, -8.660254037844422825, -9.999999999999998224 ) ) ;
#25821 = ORIENTED_EDGE ( 'NONE', *, *, #18758, .T. ) ;
#25822 = DIRECTION ( 'NONE',  ( 0.000000000000000000, 0.000000000000000000, 1.000000000000000000 ) ) ;
#25823 = VERTEX_POINT ( 'NONE', #9079 ) ;
#25824 = ADVANCED_FACE ( 'NONE', ( #20503 ), #31927, .F. ) ;
#25825 = CYLINDRICAL_SURFACE ( 'NONE', #31701, 5.000000000000000888 ) ;
#25826 = VERTEX_POINT ( 'NONE', #34962 ) ;
#25827 = FACE_OUTER_BOUND ( 'NONE', #13270, .T. ) ;
#25828 = DIRECTION ( 'NONE',  ( 0.000000000000000000, 0.000000000000000000, -1.000000000000000000 ) ) ;
#25829 = DIRECTION ( 'NONE',  ( 0.000000000000000000, 0.000000000000000000, 1.000000000000000000 ) ) ;
#25830 = AXIS2_PLACEMENT_3D ( 'NONE', #10868, #33004, #7142 ) ;
#25831 = ORIENTED_EDGE ( 'NONE', *, *, #12384, .T. ) ;
#25832 = DIRECTION ( 'NONE',  ( -0.9751893098879942379, -0.2213725590044484659, -2.706694063014921639E-17 ) ) ;
#25833 = CARTESIAN_POINT ( 'NONE',  ( 0.000000000000000000, 0.000000000000000000, 27.50000000000000000 ) ) ;
#25834 = CARTESIAN_POINT ( 'NONE',  ( 0.000000000000000000, 0.000000000000000000, 1.716666666667001406 ) ) ;
#25835 = DIRECTION ( 'NONE',  ( -1.000000000000000000, 0.000000000000000000, 0.000000000000000000 ) ) ;
#25836 = EDGE_CURVE ( 'NONE', #12353, #9125, #36320, .T. ) ;
#25837 = ORIENTED_EDGE ( 'NONE', *, *, #8035, .F. ) ;
#25838 = DIRECTION ( 'NONE',  ( 0.000000000000000000, 0.000000000000000000, 1.000000000000000000 ) ) ;
#25839 = LINE ( 'NONE', #25117, #28626 ) ;
#25840 = CARTESIAN_POINT ( 'NONE',  ( -27.78182860042817026, -56.67878100130359087, -4.999999999999997335 ) ) ;
#25841 = ORIENTED_EDGE ( 'NONE', *, *, #3045, .F. ) ;
#25842 = VERTEX_POINT ( 'NONE', #1210 ) ;
#25843 = ORIENTED_EDGE ( 'NONE', *, *, #9624, .F. ) ;
#25844 = EDGE_CURVE ( 'NONE', #35809, #34083, #10562, .T. ) ;
#25845 = DIRECTION ( 'NONE',  ( 0.000000000000000000, 0.000000000000000000, -1.000000000000000000 ) ) ;
#25846 = ADVANCED_FACE ( 'NONE', ( #18463 ), #4218, .F. ) ;
#25847 = CYLINDRICAL_SURFACE ( 'NONE', #15772, 95.00000000000001421 ) ;
#25848 = CARTESIAN_POINT ( 'NONE',  ( 107.3056136255987809, -47.85537046088835211, 32.50000000000000000 ) ) ;
#25849 = DIRECTION ( 'NONE',  ( 0.000000000000000000, 0.000000000000000000, 1.000000000000000000 ) ) ;
#25850 = VECTOR ( 'NONE', #25531, 1000.000000000000000 ) ;
#25851 = CARTESIAN_POINT ( 'NONE',  ( -68.17080498304596858, 51.15280100851584422, -5.000000000000000000 ) ) ;
#25852 = CARTESIAN_POINT ( 'NONE',  ( 7.122621931239992550E-13, 68.00000000000000000, 12.49999999999999822 ) ) ;
#25853 = VERTEX_POINT ( 'NONE', #27445 ) ;
#25854 = ORIENTED_EDGE ( 'NONE', *, *, #10709, .T. ) ;
#25855 = LINE ( 'NONE', #25685, #28435 ) ;
#25856 = DIRECTION ( 'NONE',  ( 0.000000000000000000, 0.000000000000000000, -1.000000000000000000 ) ) ;
#25857 = DIRECTION ( 'NONE',  ( -0.000000000000000000, -0.000000000000000000, 1.000000000000000000 ) ) ;
#25858 = CARTESIAN_POINT ( 'NONE',  ( 149.8799519615616020, -6.000000000000508038, 32.50000000000000000 ) ) ;
#25859 = EDGE_LOOP ( 'NONE', ( #9845, #21092, #32104, #17167 ) ) ;
#25860 = EDGE_CURVE ( 'NONE', #7230, #13311, #36259, .T. ) ;
#25861 = FACE_BOUND ( 'NONE', #22879, .T. ) ;
#25862 = ORIENTED_EDGE ( 'NONE', *, *, #7324, .F. ) ;
#25863 = ORIENTED_EDGE ( 'NONE', *, *, #24, .F. ) ;
#25864 = LINE ( 'NONE', #157, #20044 ) ;
#25865 = ORIENTED_EDGE ( 'NONE', *, *, #12245, .F. ) ;
#25866 = EDGE_CURVE ( 'NONE', #34263, #3095, #32685, .T. ) ;
#25867 = PLANE ( 'NONE',  #21220 ) ;
#25868 = CARTESIAN_POINT ( 'NONE',  ( 6.000000000000000000, -145.0000000000000568, 32.55002500000000509 ) ) ;
#25869 = EDGE_CURVE ( 'NONE', #14264, #34734, #32081, .T. ) ;
#25870 = ORIENTED_EDGE ( 'NONE', *, *, #11161, .T. ) ;
#25871 = EDGE_LOOP ( 'NONE', ( #28611, #30011, #19296, #35014 ) ) ;
#25872 = ORIENTED_EDGE ( 'NONE', *, *, #26757, .F. ) ;
#25873 = ORIENTED_EDGE ( 'NONE', *, *, #19186, .T. ) ;
#25874 = EDGE_LOOP ( 'NONE', ( #16001, #35193 ) ) ;
#25875 = DIRECTION ( 'NONE',  ( 1.000000000000000000, 0.000000000000000000, 0.000000000000000000 ) ) ;
#25876 = DIRECTION ( 'NONE',  ( 1.000000000000000000, 0.000000000000000000, 0.000000000000000000 ) ) ;
#25877 = CARTESIAN_POINT ( 'NONE',  ( 84.99999662536831124, -8.660254037844397956, 17.49999999999999645 ) ) ;
#25878 = FACE_OUTER_BOUND ( 'NONE', #36699, .T. ) ;
#25879 = CARTESIAN_POINT ( 'NONE',  ( 44.99999662536849598, -77.94228634059960825, -9.999999999999998224 ) ) ;
#25880 = VERTEX_POINT ( 'NONE', #12631 ) ;
#25881 = CYLINDRICAL_SURFACE ( 'NONE', #33886, 2.000000000000000000 ) ;
#25882 = LINE ( 'NONE', #8820, #8416 ) ;
#25883 = EDGE_CURVE ( 'NONE', #14204, #5735, #30446, .T. ) ;
#25884 = LINE ( 'NONE', #33973, #16397 ) ;
#25885 = ORIENTED_EDGE ( 'NONE', *, *, #19299, .T. ) ;
#25886 = DIRECTION ( 'NONE',  ( 1.000000000000000000, 0.000000000000000000, 0.000000000000000000 ) ) ;
#25887 = DIRECTION ( 'NONE',  ( 0.000000000000000000, 0.000000000000000000, 1.000000000000000000 ) ) ;
#25888 = VERTEX_POINT ( 'NONE', #1765 ) ;
#25889 = VERTEX_POINT ( 'NONE', #21253 ) ;
#25890 = DIRECTION ( 'NONE',  ( 0.000000000000000000, 0.000000000000000000, 1.000000000000000000 ) ) ;
#25891 = AXIS2_PLACEMENT_3D ( 'NONE', #33562, #7483, #30351 ) ;
#25892 = CARTESIAN_POINT ( 'NONE',  ( 29.99999662536857770, -69.28203230275519786, -5.000000000000000000 ) ) ;
#25893 = PLANE ( 'NONE',  #14471 ) ;
#25894 = B_SPLINE_CURVE_WITH_KNOTS ( 'NONE', 3,
 ( #13298, #7137, #12922, #18581 ),
 .UNSPECIFIED., .F., .F.,
 ( 4, 4 ),
 ( 2.380735200943099693E-07, 0.002921158011986722466 ),
 .UNSPECIFIED. ) ;
#25895 = DIRECTION ( 'NONE',  ( 0.000000000000000000, 0.000000000000000000, 1.000000000000000000 ) ) ;
#25896 = VERTEX_POINT ( 'NONE', #4774 ) ;
#25897 = ORIENTED_EDGE ( 'NONE', *, *, #14936, .T. ) ;
#25898 = DIRECTION ( 'NONE',  ( 1.000000000000000000, 0.000000000000000000, 0.000000000000000000 ) ) ;
#25899 = FACE_BOUND ( 'NONE', #6872, .T. ) ;
#25900 = DIRECTION ( 'NONE',  ( 0.000000000000000000, 0.000000000000000000, -1.000000000000000000 ) ) ;
#25901 = EDGE_CURVE ( 'NONE', #16892, #31169, #16533, .T. ) ;
#25902 = VERTEX_POINT ( 'NONE', #13199 ) ;
#25903 = EDGE_CURVE ( 'NONE', #23009, #8155, #30890, .T. ) ;
#25904 = CARTESIAN_POINT ( 'NONE',  ( -37.00000337463116296, -60.62177826491080168, -9.999999999999998224 ) ) ;
#25905 = ORIENTED_EDGE ( 'NONE', *, *, #35057, .F. ) ;
#25906 = ORIENTED_EDGE ( 'NONE', *, *, #6174, .T. ) ;
#25907 = EDGE_CURVE ( 'NONE', #26162, #36358, #35524, .T. ) ;
#25908 = AXIS2_PLACEMENT_3D ( 'NONE', #14283, #25729, #29435 ) ;
#25909 = CARTESIAN_POINT ( 'NONE',  ( -31.74999999999995737, 0.000000000000000000, 0.000000000000000000 ) ) ;
#25910 = CARTESIAN_POINT ( 'NONE',  ( 0.000000000000000000, 5.939536975864662969E-16, -4.700000000000000178 ) ) ;
#25911 = ORIENTED_EDGE ( 'NONE', *, *, #18665, .F. ) ;
#25912 = ORIENTED_EDGE ( 'NONE', *, *, #22241, .F. ) ;
#25913 = ADVANCED_FACE ( 'NONE', ( #27244 ), #4019, .F. ) ;
#25914 = DIRECTION ( 'NONE',  ( 1.000000000000000000, 0.000000000000000000, 0.000000000000000000 ) ) ;
#25915 = EDGE_CURVE ( 'NONE', #36497, #10851, #21313, .T. ) ;
#25916 = CARTESIAN_POINT ( 'NONE',  ( 0.000000000000000000, 0.000000000000000000, 27.50000000000000000 ) ) ;
#25917 = ORIENTED_EDGE ( 'NONE', *, *, #31134, .F. ) ;
#25918 = CARTESIAN_POINT ( 'NONE',  ( -3.499999999999991562, -55.00000000000000000, -5.000000000000000000 ) ) ;
#25919 = AXIS2_PLACEMENT_3D ( 'NONE', #2231, #13669, #16673 ) ;
#25920 = FACE_BOUND ( 'NONE', #25466, .T. ) ;
#25921 = AXIS2_PLACEMENT_3D ( 'NONE', #8135, #19038, #2340 ) ;
#25922 = CARTESIAN_POINT ( 'NONE',  ( -27.00000337463120914, 77.94228634059957983, 12.50000000000000000 ) ) ;
#25923 = PLANE ( 'NONE',  #18078 ) ;
#25924 = FACE_OUTER_BOUND ( 'NONE', #24822, .T. ) ;
#25925 = ADVANCED_FACE ( 'NONE', ( #21809 ), #32691, .F. ) ;
#25926 = CYLINDRICAL_SURFACE ( 'NONE', #32660, 2.000000000000000000 ) ;
#25927 = EDGE_CURVE ( 'NONE', #27221, #31238, #29091, .T. ) ;
#25928 = PRODUCT_DEFINITION_SHAPE ( 'NONE', 'NONE',  #1995 ) ;
#25929 =( LENGTH_UNIT ( ) NAMED_UNIT ( * ) SI_UNIT ( .MILLI., .METRE. ) );
#25930 = EDGE_CURVE ( 'NONE', #16096, #7521, #17181, .T. ) ;
#25931 = ADVANCED_FACE ( 'NONE', ( #15818 ), #24461, .F. ) ;
#25932 = CARTESIAN_POINT ( 'NONE',  ( 64.99999662536841072, 25.98076211353318854, 12.50000000000000000 ) ) ;
#25933 = ORIENTED_EDGE ( 'NONE', *, *, #34210, .F. ) ;
#25934 = EDGE_CURVE ( 'NONE', #20212, #32853, #29124, .T. ) ;
#25935 = DIRECTION ( 'NONE',  ( 0.000000000000000000, 0.000000000000000000, -1.000000000000000000 ) ) ;
#25936 = CARTESIAN_POINT ( 'NONE',  ( 6.999996625368676284, -77.94228634059960825, 17.49999999999999645 ) ) ;
#25937 = AXIS2_PLACEMENT_3D ( 'NONE', #6242, #34036, #2901 ) ;
#25938 = DIRECTION ( 'NONE',  ( -0.000000000000000000, -0.000000000000000000, 1.000000000000000000 ) ) ;
#25939 = ORIENTED_EDGE ( 'NONE', *, *, #26399, .F. ) ;
#25940 = VECTOR ( 'NONE', #9750, 1000.000000000000000 ) ;
#25941 = EDGE_LOOP ( 'NONE', ( #784, #24460, #19921, #20916 ) ) ;
#25942 = EDGE_LOOP ( 'NONE', ( #36693, #3719, #18005, #10150 ) ) ;
#25943 = FACE_OUTER_BOUND ( 'NONE', #35632, .T. ) ;
#25944 = DIRECTION ( 'NONE',  ( 0.000000000000000000, 0.000000000000000000, 1.000000000000000000 ) ) ;
#25945 = FACE_OUTER_BOUND ( 'NONE', #22587, .T. ) ;
#25946 = ORIENTED_EDGE ( 'NONE', *, *, #25814, .F. ) ;
#25947 = DIRECTION ( 'NONE',  ( 1.000000000000000000, 0.000000000000000000, 0.000000000000000000 ) ) ;
#25948 = AXIS2_PLACEMENT_3D ( 'NONE', #25932, #11491, #11852 ) ;
#25949 = EDGE_LOOP ( 'NONE', ( #21065, #34527, #7008, #35795 ) ) ;
#25950 = CARTESIAN_POINT ( 'NONE',  ( -23.27275137504124203, -104.1535408905101860, 32.50000000000000711 ) ) ;
#25951 = ORIENTED_EDGE ( 'NONE', *, *, #24532, .F. ) ;
#25952 = FACE_OUTER_BOUND ( 'NONE', #22845, .T. ) ;
#25953 = ORIENTED_EDGE ( 'NONE', *, *, #30883, .F. ) ;
#25954 = EDGE_LOOP ( 'NONE', ( #26424, #369 ) ) ;
#25955 = CYLINDRICAL_SURFACE ( 'NONE', #17217, 2.000000000000001776 ) ;
#25956 = LINE ( 'NONE', #25791, #36389 ) ;
#25957 = DIRECTION ( 'NONE',  ( -0.8660254037844382635, -0.5000000000000006661, 0.000000000000000000 ) ) ;
#25958 =( REPRESENTATION_RELATIONSHIP ('NONE','NONE', #15268, #34443 ) REPRESENTATION_RELATIONSHIP_WITH_TRANSFORMATION ( #14350 )SHAPE_REPRESENTATION_RELATIONSHIP( ) );
#25959 = ORIENTED_EDGE ( 'NONE', *, *, #1683, .F. ) ;
#25960 = CARTESIAN_POINT ( 'NONE',  ( 7.999996625368625658, 86.60254037844397601, 17.49999999999999645 ) ) ;
#25961 = AXIS2_PLACEMENT_3D ( 'NONE', #9626, #29655, #794 ) ;
#25962 = LINE ( 'NONE', #6089, #12062 ) ;
#25963 = DIRECTION ( 'NONE',  ( 0.000000000000000000, 0.000000000000000000, -1.000000000000000000 ) ) ;
#25964 = ORIENTED_EDGE ( 'NONE', *, *, #32671, .T. ) ;
#25965 = CYLINDRICAL_SURFACE ( 'NONE', #17149, 2.000000000000001776 ) ;
#25966 = CARTESIAN_POINT ( 'NONE',  ( 61.99999662536842493, 51.96152422706639129, -5.000000000000000000 ) ) ;
#25967 = EDGE_LOOP ( 'NONE', ( #33205, #36167, #2383, #1279 ) ) ;
#25968 = FACE_OUTER_BOUND ( 'NONE', #34478, .T. ) ;
#25969 = DIRECTION ( 'NONE',  ( 1.000000000000000000, 0.000000000000000000, 0.000000000000000000 ) ) ;
#25970 = DIRECTION ( 'NONE',  ( 0.000000000000000000, 0.000000000000000000, 1.000000000000000000 ) ) ;
#25971 = DIRECTION ( 'NONE',  ( 0.000000000000000000, 0.000000000000000000, 1.000000000000000000 ) ) ;
#25972 = CIRCLE ( 'NONE', #9796, 2.000000000000001776 ) ;
#25973 = EDGE_CURVE ( 'NONE', #5915, #23282, #34013, .T. ) ;
#25974 = DIRECTION ( 'NONE',  ( 0.000000000000000000, 0.000000000000000000, -1.000000000000000000 ) ) ;
#25975 = AXIS2_PLACEMENT_3D ( 'NONE', #11271, #5292, #19718 ) ;
#25976 = EDGE_CURVE ( 'NONE', #4621, #30710, #14309, .T. ) ;
#25977 = ORIENTED_EDGE ( 'NONE', *, *, #23838, .F. ) ;
#25978 = CARTESIAN_POINT ( 'NONE',  ( 0.000000000000000000, 0.000000000000000000, 0.000000000000000000 ) ) ;
#25979 = CARTESIAN_POINT ( 'NONE',  ( -55.00000337463109901, -60.62177826491083010, 17.49999999999999645 ) ) ;
#25980 = CIRCLE ( 'NONE', #30761, 2.000000000000001776 ) ;
#25981 = ORIENTED_EDGE ( 'NONE', *, *, #23524, .T. ) ;
#25982 = EDGE_LOOP ( 'NONE', ( #7282, #16500, #1049, #28182 ) ) ;
#25983 = ORIENTED_EDGE ( 'NONE', *, *, #6613, .F. ) ;
#25984 = DIRECTION ( 'NONE',  ( -0.000000000000000000, -0.000000000000000000, 1.000000000000000000 ) ) ;
#25985 = DIRECTION ( 'NONE',  ( 0.000000000000000000, 0.000000000000000000, 1.000000000000000000 ) ) ;
#25986 = DIRECTION ( 'NONE',  ( 0.000000000000000000, 0.000000000000000000, 1.000000000000000000 ) ) ;
#25987 = VECTOR ( 'NONE', #7268, 1000.000000000000000 ) ;
#25988 = DIRECTION ( 'NONE',  ( 0.000000000000000000, 0.000000000000000000, 1.000000000000000000 ) ) ;
#25989 = ORIENTED_EDGE ( 'NONE', *, *, #23229, .T. ) ;
#25990 = CARTESIAN_POINT ( 'NONE',  ( 43.19957991610432657, 47.04203867989531318, 12.49999999999999822 ) ) ;
#25991 = EDGE_LOOP ( 'NONE', ( #20681, #19471 ) ) ;
#25992 = FACE_BOUND ( 'NONE', #34911, .T. ) ;
#25993 = ADVANCED_FACE ( 'NONE', ( #22925 ), #8123, .T. ) ;
#25994 = CIRCLE ( 'NONE', #9824, 27.00000000000001421 ) ;
#25995 = FACE_OUTER_BOUND ( 'NONE', #21614, .T. ) ;
#25996 = CIRCLE ( 'NONE', #22408, 2.000000000000001776 ) ;
#25997 = DIRECTION ( 'NONE',  ( 1.000000000000000000, 0.000000000000000000, -0.000000000000000000 ) ) ;
#25998 = DIRECTION ( 'NONE',  ( 0.000000000000000000, 0.000000000000000000, -1.000000000000000000 ) ) ;
#25999 = CARTESIAN_POINT ( 'NONE',  ( 47.63139720814438505, -27.49999999999955946, -16.00000000000000000 ) ) ;
#26000 = DIRECTION ( 'NONE',  ( 0.000000000000000000, 0.000000000000000000, 1.000000000000000000 ) ) ;
#26001 = EDGE_CURVE ( 'NONE', #31719, #15333, #14170, .T. ) ;
#26002 = CARTESIAN_POINT ( 'NONE',  ( -12.00000337463128908, 69.28203230275516944, -5.000000000000000000 ) ) ;
#26003 = CARTESIAN_POINT ( 'NONE',  ( 44.99999662536849598, 60.62177826491077326, -5.000000000000000000 ) ) ;
#26004 = ORIENTED_EDGE ( 'NONE', *, *, #19186, .F. ) ;
#26005 = LINE ( 'NONE', #11746, #35195 ) ;
#26006 = CARTESIAN_POINT ( 'NONE',  ( -75.00000337463099243, -25.98076211353322051, -5.000000000000000000 ) ) ;
#26007 = DIRECTION ( 'NONE',  ( 0.000000000000000000, 0.000000000000000000, 1.000000000000000000 ) ) ;
#26008 = ORIENTED_EDGE ( 'NONE', *, *, #21339, .T. ) ;
#26009 = AXIS2_PLACEMENT_3D ( 'NONE', #14927, #25984, #669 ) ;
#26010 = ORIENTED_EDGE ( 'NONE', *, *, #32983, .T. ) ;
#26011 = EDGE_CURVE ( 'NONE', #32397, #27172, #29711, .T. ) ;
#26012 = EDGE_LOOP ( 'NONE', ( #17414, #12104 ) ) ;
#26013 = AXIS2_PLACEMENT_3D ( 'NONE', #14251, #25698, #6412 ) ;
#26014 = AXIS2_PLACEMENT_3D ( 'NONE', #24154, #3725, #18551 ) ;
#26015 = DIRECTION ( 'NONE',  ( 0.000000000000000000, 0.000000000000000000, 1.000000000000000000 ) ) ;
#26016 = VECTOR ( 'NONE', #30297, 1000.000000000000000 ) ;
#26017 = CARTESIAN_POINT ( 'NONE',  ( 0.000000000000000000, 0.000000000000000000, -5.000000000000000000 ) ) ;
#26018 = CARTESIAN_POINT ( 'NONE',  ( 11.99999662536865763, -86.60254037844400443, 17.49999999999999645 ) ) ;
#26019 = DIRECTION ( 'NONE',  ( 0.000000000000000000, 0.000000000000000000, 1.000000000000000000 ) ) ;
#26020 = CYLINDRICAL_SURFACE ( 'NONE', #7811, 2.000000000000001776 ) ;
#26021 = VERTEX_POINT ( 'NONE', #19922 ) ;
#26022 = ORIENTED_EDGE ( 'NONE', *, *, #5743, .F. ) ;
#26023 = CARTESIAN_POINT ( 'NONE',  ( -58.48108235278846934, -36.97203788309006711, -49.86561046011506448 ) ) ;
#26024 = CIRCLE ( 'NONE', #3888, 3.500000000000003109 ) ;
#26025 = ADVANCED_FACE ( 'NONE', ( #8495 ), #19566, .F. ) ;
#26026 = DIRECTION ( 'NONE',  ( -1.000000000000000000, 0.000000000000000000, -0.000000000000000000 ) ) ;
#26027 = AXIS2_PLACEMENT_3D ( 'NONE', #35443, #9730, #1470 ) ;
#26028 = DIRECTION ( 'NONE',  ( 0.000000000000000000, 0.000000000000000000, 1.000000000000000000 ) ) ;
#26029 = ORIENTED_EDGE ( 'NONE', *, *, #30332, .F. ) ;
#26030 = ADVANCED_FACE ( 'NONE', ( #22556 ), #25559, .F. ) ;
#26031 = CIRCLE ( 'NONE', #19458, 2.000000000000001776 ) ;
#26032 = FACE_BOUND ( 'NONE', #7631, .T. ) ;
#26033 = ORIENTED_EDGE ( 'NONE', *, *, #31808, .F. ) ;
#26034 = EDGE_LOOP ( 'NONE', ( #4324, #27766, #33691, #8850, #19558, #20520, #33744, #34425, #16226, #24407, #17613, #29622 ) ) ;
#26035 = ADVANCED_FACE ( 'NONE', ( #25207 ), #19373, .F. ) ;
#26036 = CARTESIAN_POINT ( 'NONE',  ( 79.99999662536832545, -34.64101615137759183, -9.999999999999998224 ) ) ;
#26037 = ORIENTED_EDGE ( 'NONE', *, *, #22365, .F. ) ;
#26038 = AXIS2_PLACEMENT_3D ( 'NONE', #12280, #20737, #862 ) ;
#26039 = AXIS2_PLACEMENT_3D ( 'NONE', #25106, #27883, #2919 ) ;
#26040 = CARTESIAN_POINT ( 'NONE',  ( 66.00000000000000000, 2.445500000000000007, 0.000000000000000000 ) ) ;
#26041 = ADVANCED_FACE ( 'NONE', ( #10763 ), #36452, .F. ) ;
#26042 = DIRECTION ( 'NONE',  ( 0.000000000000000000, 0.000000000000000000, 1.000000000000000000 ) ) ;
#26043 = ORIENTED_EDGE ( 'NONE', *, *, #13572, .T. ) ;
#26044 = ORIENTED_EDGE ( 'NONE', *, *, #30402, .F. ) ;
#26045 = EDGE_LOOP ( 'NONE', ( #34348, #20052 ) ) ;
#26046 = ORIENTED_EDGE ( 'NONE', *, *, #16277, .F. ) ;
#26047 = ORIENTED_EDGE ( 'NONE', *, *, #15628, .F. ) ;
#26049 = DIRECTION ( 'NONE',  ( 0.000000000000000000, 0.000000000000000000, 1.000000000000000000 ) ) ;
#26048 = AXIS2_PLACEMENT_3D ( 'NONE', #5167, #8361, #16606 ) ;
#26050 = ADVANCED_FACE ( 'NONE', ( #22367 ), #19210, .F. ) ;
#26051 =( LENGTH_UNIT ( ) NAMED_UNIT ( * ) SI_UNIT ( .MILLI., .METRE. ) );
#26052 = CIRCLE ( 'NONE', #6892, 2.000000000000001776 ) ;
#26053 = DIRECTION ( 'NONE',  ( 0.000000000000000000, 0.000000000000000000, 1.000000000000000000 ) ) ;
#26054 = DIRECTION ( 'NONE',  ( 0.000000000000000000, 0.000000000000000000, 1.000000000000000000 ) ) ;
#26055 = DIRECTION ( 'NONE',  ( -1.000000000000000000, 0.000000000000000000, 0.000000000000000000 ) ) ;
#26056 = EDGE_LOOP ( 'NONE', ( #29392, #789 ) ) ;
#26057 = AXIS2_PLACEMENT_3D ( 'NONE', #20367, #25988, #6115 ) ;
#26058 = CARTESIAN_POINT ( 'NONE',  ( 24.99999662536859546, -77.94228634059960825, -9.999999999999998224 ) ) ;
#26059 = VECTOR ( 'NONE', #21141, 1000.000000000000000 ) ;
#26060 = ADVANCED_FACE ( 'NONE', ( #30624 ), #33810, .F. ) ;
#26061 = CARTESIAN_POINT ( 'NONE',  ( 76.99999662536836809, -8.660254037844401509, 17.49999999999999645 ) ) ;
#26062 = CARTESIAN_POINT ( 'NONE',  ( 62.33939050065184517, -13.89091430021398565, 12.49999999999999822 ) ) ;
#26063 = ORIENTED_EDGE ( 'NONE', *, *, #35009, .F. ) ;
#26064 = CARTESIAN_POINT ( 'NONE',  ( -80.00000337463094979, -2.428612866367529932E-14, 17.49999999999999645 ) ) ;
#26065 = CARTESIAN_POINT ( 'NONE',  ( 83.47442710120355969, -31.09745072740822991, -49.86348611802629449 ) ) ;
#26066 = AXIS2_PLACEMENT_3D ( 'NONE', #12080, #23734, #6670 ) ;
#26067 = CIRCLE ( 'NONE', #9903, 2.000000000000001776 ) ;
#26068 = ORIENTED_EDGE ( 'NONE', *, *, #1618, .F. ) ;
#26069 = EDGE_CURVE ( 'NONE', #34910, #32311, #23140, .T. ) ;
#26070 = CONICAL_SURFACE ( 'NONE', #34483, 6.726859516510129922, 1.221730476396047038 ) ;
#26071 = ORIENTED_EDGE ( 'NONE', *, *, #18406, .T. ) ;
#26072 = CARTESIAN_POINT ( 'NONE',  ( -15.00000337463125710, -77.94228634059960825, -9.999999999999998224 ) ) ;
#26073 = EDGE_CURVE ( 'NONE', #9400, #18535, #11749, .T. ) ;
#26074 = CARTESIAN_POINT ( 'NONE',  ( 52.99999662536844625, -60.62177826491080168, 12.50000000000000000 ) ) ;
#26075 = CARTESIAN_POINT ( 'NONE',  ( 11.99999662536862566, 86.60254037844397601, 12.50000000000000000 ) ) ;
#26076 = FACE_OUTER_BOUND ( 'NONE', #31466, .T. ) ;
#26077 = EDGE_LOOP ( 'NONE', ( #35179, #16914, #29028, #14286 ) ) ;
#26078 = DIRECTION ( 'NONE',  ( -0.000000000000000000, -0.000000000000000000, 1.000000000000000000 ) ) ;
#26079 = LINE ( 'NONE', #3590, #27908 ) ;
#26080 = DIRECTION ( 'NONE',  ( -1.000000000000000000, -0.000000000000000000, -0.000000000000000000 ) ) ;
#26081 = AXIS2_PLACEMENT_3D ( 'NONE', #33072, #16026, #36083 ) ;
#26082 = VERTEX_POINT ( 'NONE', #28183 ) ;
#26083 = CIRCLE ( 'NONE', #33264, 3.000000000000006661 ) ;
#26084 = DIRECTION ( 'NONE',  ( 0.000000000000000000, -0.4999999999999996114, 0.8660254037844388186 ) ) ;
#26085 = ORIENTED_EDGE ( 'NONE', *, *, #28453, .T. ) ;
#26086 = AXIS2_PLACEMENT_3D ( 'NONE', #28825, #3150, #14578 ) ;
#26087 = TOROIDAL_SURFACE ( 'NONE', #7517, 3.866666666667000651, 1.133333333332999793 ) ;
#26088 = AXIS2_PLACEMENT_3D ( 'NONE', #37076, #674, #23544 ) ;
#26089 = CARTESIAN_POINT ( 'NONE',  ( 52.99999662536844625, -60.62177826491080168, 17.49999999999999645 ) ) ;
#26090 = AXIS2_PLACEMENT_3D ( 'NONE', #36527, #13991, #33533 ) ;
#26091 = CARTESIAN_POINT ( 'NONE',  ( -87.00000337463093558, 8.660254037844389075, -9.999999999999998224 ) ) ;
#26092 = EDGE_CURVE ( 'NONE', #200, #21374, #30336, .T. ) ;
#26093 = DIRECTION ( 'NONE',  ( -1.000000000000000000, 0.000000000000000000, 0.000000000000000000 ) ) ;
#26094 = ORIENTED_EDGE ( 'NONE', *, *, #5333, .T. ) ;
#26095 = EDGE_LOOP ( 'NONE', ( #4283, #17732 ) ) ;
#26096 = CARTESIAN_POINT ( 'NONE',  ( 22.99999662536859901, -77.94228634059960825, -9.999999999999998224 ) ) ;
#26097 = DIRECTION ( 'NONE',  ( -1.000000000000000000, 0.000000000000000000, 0.000000000000000000 ) ) ;
#26098 = AXIS2_PLACEMENT_3D ( 'NONE', #27480, #10601, #4248 ) ;
#26099 = CARTESIAN_POINT ( 'NONE',  ( -20.00000337463123756, -86.60254037844400443, -9.999999999999998224 ) ) ;
#26100 = ORIENTED_EDGE ( 'NONE', *, *, #5786, .F. ) ;
#26101 = CARTESIAN_POINT ( 'NONE',  ( -70.00000337463099243, 17.32050807568877460, -9.999999999999998224 ) ) ;
#26102 = FACE_BOUND ( 'NONE', #1967, .T. ) ;
#26103 = CARTESIAN_POINT ( 'NONE',  ( 21.99999662536857770, 86.60254037844397601, -9.999999999999998224 ) ) ;
#26104 = DIRECTION ( 'NONE',  ( 0.000000000000000000, 0.000000000000000000, 1.000000000000000000 ) ) ;
#26105 = CARTESIAN_POINT ( 'NONE',  ( -75.00000337463097821, 8.660254037844374864, 12.50000000000000000 ) ) ;
#26106 = FACE_OUTER_BOUND ( 'NONE', #34593, .T. ) ;
#26107 = EDGE_CURVE ( 'NONE', #15570, #13632, #27338, .T. ) ;
#26108 = CYLINDRICAL_SURFACE ( 'NONE', #12572, 2.000000000000001776 ) ;
#26109 = CARTESIAN_POINT ( 'NONE',  ( 62.99999662536839651, 60.62177826491078747, 12.50000000000000000 ) ) ;
#26110 = VERTEX_POINT ( 'NONE', #5500 ) ;
#26111 = ADVANCED_FACE ( 'NONE', ( #14107 ), #37003, .F. ) ;
#26112 = DIRECTION ( 'NONE',  ( 0.000000000000000000, 0.000000000000000000, -1.000000000000000000 ) ) ;
#26113 = CARTESIAN_POINT ( 'NONE',  ( 5.000000000000007994, -2.886751345948139758, -0.5999999999999998668 ) ) ;
#26114 = DIRECTION ( 'NONE',  ( 1.000000000000000000, 0.000000000000000000, 0.000000000000000000 ) ) ;
#26115 = AXIS2_PLACEMENT_3D ( 'NONE', #26448, #15023, #23639 ) ;
#26116 = ORIENTED_EDGE ( 'NONE', *, *, #18830, .T. ) ;
#26117 = EDGE_CURVE ( 'NONE', #18742, #27467, #8858, .T. ) ;
#26118 = CIRCLE ( 'NONE', #28491, 1.999999999999998224 ) ;
#26119 = VERTEX_POINT ( 'NONE', #771 ) ;
#26120 = AXIS2_PLACEMENT_3D ( 'NONE', #22842, #34278, #28987 ) ;
#26121 = ORIENTED_EDGE ( 'NONE', *, *, #35783, .T. ) ;
#26122 = EDGE_CURVE ( 'NONE', #21182, #17038, #20170, .T. ) ;
#26123 = DIRECTION ( 'NONE',  ( 0.000000000000000000, 0.000000000000000000, 1.000000000000000000 ) ) ;
#26124 = CARTESIAN_POINT ( 'NONE',  ( -50.00000337463109190, 51.96152422706637708, 12.50000000000000000 ) ) ;
#26125 = EDGE_CURVE ( 'NONE', #21598, #14210, #1003, .T. ) ;
#26126 = DIRECTION ( 'NONE',  ( 0.000000000000000000, 0.000000000000000000, -1.000000000000000000 ) ) ;
#26127 = ORIENTED_EDGE ( 'NONE', *, *, #12948, .F. ) ;
#26128 = CIRCLE ( 'NONE', #5797, 2.000000000000001776 ) ;
#26129 = DIRECTION ( 'NONE',  ( 0.000000000000000000, 0.000000000000000000, 1.000000000000000000 ) ) ;
#26130 = ORIENTED_EDGE ( 'NONE', *, *, #27457, .F. ) ;
#26131 = DIRECTION ( 'NONE',  ( -1.000000000000000000, 0.000000000000000000, 0.000000000000000000 ) ) ;
#26132 = ORIENTED_EDGE ( 'NONE', *, *, #14774, .F. ) ;
#26133 = CARTESIAN_POINT ( 'NONE',  ( 81.99999662536832545, -34.64101615137759183, -9.999999999999998224 ) ) ;
#26134 = ORIENTED_EDGE ( 'NONE', *, *, #32921, .T. ) ;
#26135 = EDGE_CURVE ( 'NONE', #31600, #1195, #19562, .T. ) ;
#26136 = AXIS2_PLACEMENT_3D ( 'NONE', #407, #26651, #11842 ) ;
#26137 = VERTEX_POINT ( 'NONE', #23657 ) ;
#26138 = CARTESIAN_POINT ( 'NONE',  ( 70.80619744049005249, 84.18124734178236679, 32.50000000000000000 ) ) ;
#26139 = CARTESIAN_POINT ( 'NONE',  ( 0.9154378789997317245, -5.244974386029391589, -1.156968425231173381 ) ) ;
#26140 = EDGE_CURVE ( 'NONE', #35478, #5493, #22551, .T. ) ;
#26141 = AXIS2_PLACEMENT_3D ( 'NONE', #35269, #32237, #23443 ) ;
#26142 = CARTESIAN_POINT ( 'NONE',  ( -47.00000337463111322, 77.94228634059959404, -9.999999999999998224 ) ) ;
#26143 = ORIENTED_EDGE ( 'NONE', *, *, #1750, .T. ) ;
#26144 = DIRECTION ( 'NONE',  ( 0.000000000000000000, 0.000000000000000000, 1.000000000000000000 ) ) ;
#26145 = CIRCLE ( 'NONE', #29132, 2.000000000000000000 ) ;
#26146 = AXIS2_PLACEMENT_3D ( 'NONE', #2735, #25812, #11530 ) ;
#26147 = AXIS2_PLACEMENT_3D ( 'NONE', #36050, #33212, #24050 ) ;
#26148 = DIRECTION ( 'NONE',  ( 0.000000000000000000, -1.224646799147353207E-16, 1.000000000000000000 ) ) ;
#26149 = CARTESIAN_POINT ( 'NONE',  ( -101.7384897088158766, -110.2237710830526112, 32.55002500000000509 ) ) ;
#26150 = AXIS2_PLACEMENT_3D ( 'NONE', #5730, #8913, #31932 ) ;
#26151 = EDGE_LOOP ( 'NONE', ( #10266, #25983, #17263, #28095 ) ) ;
#26152 = DIRECTION ( 'NONE',  ( 1.000000000000000000, 0.000000000000000000, 0.000000000000000000 ) ) ;
#26153 = DIRECTION ( 'NONE',  ( 0.000000000000000000, 0.000000000000000000, 1.000000000000000000 ) ) ;
#26154 = ORIENTED_EDGE ( 'NONE', *, *, #30932, .T. ) ;
#26155 = DIRECTION ( 'NONE',  ( 0.000000000000000000, 0.000000000000000000, 1.000000000000000000 ) ) ;
#26156 = DIRECTION ( 'NONE',  ( 0.000000000000000000, 0.000000000000000000, -1.000000000000000000 ) ) ;
#26157 = CARTESIAN_POINT ( 'NONE',  ( -72.72667006428976322, 101.6652913307188868, 27.50000000000000000 ) ) ;
#26158 = DIRECTION ( 'NONE',  ( 1.000000000000000000, 0.000000000000000000, 0.000000000000000000 ) ) ;
#26159 = VECTOR ( 'NONE', #26084, 1000.000000000000000 ) ;
#26160 = ADVANCED_FACE ( 'NONE', ( #8666 ), #17651, .F. ) ;
#26161 = CARTESIAN_POINT ( 'NONE',  ( 77.99999662536832545, -17.32050807568879591, 12.50000000000000000 ) ) ;
#26162 = VERTEX_POINT ( 'NONE', #18032 ) ;
#26163 = EDGE_CURVE ( 'NONE', #22787, #3559, #20105, .T. ) ;
#26164 = DIRECTION ( 'NONE',  ( 1.000000000000000000, 0.000000000000000000, 0.000000000000000000 ) ) ;
#26165 = LINE ( 'NONE', #32144, #3956 ) ;
#26166 = CARTESIAN_POINT ( 'NONE',  ( 1.648146632868999539, 4.821944789745367110, -6.000000000000003553 ) ) ;
#26167 = CIRCLE ( 'NONE', #3415, 2.000000000000000000 ) ;
#26168 = ORIENTED_EDGE ( 'NONE', *, *, #32768, .T. ) ;
#26169 = ORIENTED_EDGE ( 'NONE', *, *, #34773, .F. ) ;
#26170 = VERTEX_POINT ( 'NONE', #25918 ) ;
#26171 = AXIS2_PLACEMENT_3D ( 'NONE', #7778, #21468, #1581 ) ;
#26172 = PLANE ( 'NONE',  #463 ) ;
#26173 = ADVANCED_FACE ( 'NONE', ( #17309 ), #32278, .F. ) ;
#26174 = CARTESIAN_POINT ( 'NONE',  ( 106.7731239591682026, -98.28784258493070070, 32.55002500000000509 ) ) ;
#26175 = CIRCLE ( 'NONE', #5839, 2.000000000000001776 ) ;
#26176 = VECTOR ( 'NONE', #15934, 1000.000000000000000 ) ;
#26177 = CIRCLE ( 'NONE', #416, 2.000000000000001776 ) ;
#26178 = AXIS2_PLACEMENT_3D ( 'NONE', #27630, #33458, #7771 ) ;
#26179 = CARTESIAN_POINT ( 'NONE',  ( -15.00000337463126066, 77.94228634059957983, 17.49999999999999645 ) ) ;
#26180 = EDGE_LOOP ( 'NONE', ( #33954, #27741, #18669, #3721, #21270, #20421 ) ) ;
#26181 = DIRECTION ( 'NONE',  ( 1.000000000000000000, 0.000000000000000000, 0.000000000000000000 ) ) ;
#26182 = ORIENTED_EDGE ( 'NONE', *, *, #8787, .T. ) ;
#26183 = FACE_BOUND ( 'NONE', #32715, .T. ) ;
#26184 = CIRCLE ( 'NONE', #12404, 3.000000000000002665 ) ;
#26185 = ADVANCED_FACE ( 'NONE', ( #34553 ), #3609, .F. ) ;
#26186 = AXIS2_PLACEMENT_3D ( 'NONE', #35843, #12573, #35295 ) ;
#26187 = EDGE_CURVE ( 'NONE', #26782, #18020, #10593, .T. ) ;
#26188 = DIRECTION ( 'NONE',  ( 0.000000000000000000, 0.000000000000000000, 1.000000000000000000 ) ) ;
#26189 = EDGE_CURVE ( 'NONE', #30229, #33896, #15379, .T. ) ;
#26190 = EDGE_CURVE ( 'NONE', #30372, #30464, #31884, .T. ) ;
#26191 = FACE_OUTER_BOUND ( 'NONE', #314, .T. ) ;
#26192 = ORIENTED_EDGE ( 'NONE', *, *, #35996, .T. ) ;
#26193 = DIRECTION ( 'NONE',  ( 0.000000000000000000, 0.000000000000000000, 1.000000000000000000 ) ) ;
#26194 = AXIS2_PLACEMENT_3D ( 'NONE', #26702, #6822, #29891 ) ;
#26195 = VECTOR ( 'NONE', #34913, 1000.000000000000000 ) ;
#26196 = LINE ( 'NONE', #28980, #31444 ) ;
#26197 = VECTOR ( 'NONE', #24656, 1000.000000000000000 ) ;
#26198 = DIRECTION ( 'NONE',  ( 1.000000000000000000, 0.000000000000000000, 0.000000000000000000 ) ) ;
#26199 = CARTESIAN_POINT ( 'NONE',  ( -42.97377950131527058, 96.90768712682508124, 27.49999999999999645 ) ) ;
#26200 = ORIENTED_EDGE ( 'NONE', *, *, #20100, .T. ) ;
#26201 = CARTESIAN_POINT ( 'NONE',  ( -35.00000337463116296, -60.62177826491080168, -9.999999999999998224 ) ) ;
#26202 = CARTESIAN_POINT ( 'NONE',  ( 12.99999662536863632, -77.94228634059960825, -9.999999999999998224 ) ) ;
#26203 = CARTESIAN_POINT ( 'NONE',  ( 32.16008401677996886, 61.25926521283068382, -4.999999999999997335 ) ) ;
#26204 = VECTOR ( 'NONE', #20398, 1000.000000000000000 ) ;
#26205 = ORIENTED_EDGE ( 'NONE', *, *, #26843, .F. ) ;
#26206 = AXIS2_PLACEMENT_3D ( 'NONE', #19912, #11096, #14094 ) ;
#26207 = ORIENTED_EDGE ( 'NONE', *, *, #7435, .F. ) ;
#26208 = ORIENTED_EDGE ( 'NONE', *, *, #26474, .T. ) ;
#26209 = DIRECTION ( 'NONE',  ( 0.000000000000000000, 0.000000000000000000, 1.000000000000000000 ) ) ;
#26210 = VECTOR ( 'NONE', #29145, 1000.000000000000000 ) ;
#26211 = EDGE_CURVE ( 'NONE', #8583, #13323, #3386, .T. ) ;
#26212 = LINE ( 'NONE', #319, #25817 ) ;
#26213 = AXIS2_PLACEMENT_3D ( 'NONE', #32661, #6791, #9628 ) ;
#26214 = DIRECTION ( 'NONE',  ( 0.000000000000000000, 0.000000000000000000, -1.000000000000000000 ) ) ;
#26215 = LINE ( 'NONE', #2986, #8136 ) ;
#26216 = DIRECTION ( 'NONE',  ( 1.000000000000000000, 0.000000000000000000, 0.000000000000000000 ) ) ;
#26217 = CIRCLE ( 'NONE', #22023, 65.00000000000000000 ) ;
#26218 = CIRCLE ( 'NONE', #23221, 2.000000000000001776 ) ;
#26219 = DIRECTION ( 'NONE',  ( 1.000000000000000000, 0.000000000000000000, 0.000000000000000000 ) ) ;
#26220 = EDGE_LOOP ( 'NONE', ( #13538, #36933 ) ) ;
#26221 = CIRCLE ( 'NONE', #25064, 2.000000000000001776 ) ;
#26222 = ORIENTED_EDGE ( 'NONE', *, *, #1553, .T. ) ;
#26223 = CARTESIAN_POINT ( 'NONE',  ( 84.99999662536831124, -25.98076211353319565, -9.999999999999998224 ) ) ;
#26224 = AXIS2_PLACEMENT_3D ( 'NONE', #227, #34375, #37015 ) ;
#26225 = CARTESIAN_POINT ( 'NONE',  ( 0.000000000000000000, 0.000000000000000000, 27.50000000000000000 ) ) ;
#26226 = B_SPLINE_CURVE_WITH_KNOTS ( 'NONE', 3,
 ( #9413, #20646, #6222, #14858, #32076 ),
 .UNSPECIFIED., .F., .F.,
 ( 4, 1, 4 ),
 ( 0.000000000000000000, 0.002886751345948134623, 0.005773502691896269245 ),
 .UNSPECIFIED. ) ;
#26227 = DIRECTION ( 'NONE',  ( 0.000000000000000000, 0.000000000000000000, 1.000000000000000000 ) ) ;
#26228 = EDGE_LOOP ( 'NONE', ( #25323, #15851, #35681, #25841 ) ) ;
#26229 = VECTOR ( 'NONE', #4883, 1000.000000000000000 ) ;
#26230 = FACE_BOUND ( 'NONE', #1921, .T. ) ;
#26231 = ORIENTED_EDGE ( 'NONE', *, *, #31637, .T. ) ;
#26232 = ORIENTED_EDGE ( 'NONE', *, *, #20583, .T. ) ;
#26233 = EDGE_CURVE ( 'NONE', #34990, #20996, #8185, .T. ) ;
#26234 = LINE ( 'NONE', #28675, #3853 ) ;
#26235 = ORIENTED_EDGE ( 'NONE', *, *, #27990, .T. ) ;
#26236 = AXIS2_PLACEMENT_3D ( 'NONE', #19119, #35805, #30541 ) ;
#26237 = CARTESIAN_POINT ( 'NONE',  ( 14.99999662536863632, -77.94228634059960825, -9.999999999999998224 ) ) ;
#26238 = LINE ( 'NONE', #23599, #35252 ) ;
#26239 = ORIENTED_EDGE ( 'NONE', *, *, #11005, .F. ) ;
#26240 = VERTEX_POINT ( 'NONE', #14855 ) ;
#26241 = EDGE_LOOP ( 'NONE', ( #33473, #17298, #3540, #31947, #27322 ) ) ;
#26242 = AXIS2_PLACEMENT_3D ( 'NONE', #31589, #3105, #6271 ) ;
#26243 = ORIENTED_EDGE ( 'NONE', *, *, #18531, .T. ) ;
#26244 = VECTOR ( 'NONE', #19530, 1000.000000000000000 ) ;
#26245 = VERTEX_POINT ( 'NONE', #968 ) ;
#26246 = CARTESIAN_POINT ( 'NONE',  ( -37.50000000000000000, -103.4105893997321743, 32.50000000000000000 ) ) ;
#26247 = FILL_AREA_STYLE ('',( #173 ) ) ;
#26248 = ORIENTED_EDGE ( 'NONE', *, *, #15595, .T. ) ;
#26249 = CARTESIAN_POINT ( 'NONE',  ( 9.999996625368655856, -69.28203230275519786, -9.999999999999998224 ) ) ;
#26250 = CARTESIAN_POINT ( 'NONE',  ( 106.4067350097334099, 40.94759250334365674, 32.50000000000000000 ) ) ;
#26251 = DIRECTION ( 'NONE',  ( 1.000000000000000000, 0.000000000000000000, 0.000000000000000000 ) ) ;
#26252 = EDGE_CURVE ( 'NONE', #14264, #29027, #26294, .T. ) ;
#26253 = AXIS2_PLACEMENT_3D ( 'NONE', #34176, #11083, #33986 ) ;
#26254 = VERTEX_POINT ( 'NONE', #34916 ) ;
#26255 = DIRECTION ( 'NONE',  ( 0.000000000000000000, 0.000000000000000000, 1.000000000000000000 ) ) ;
#26256 = VECTOR ( 'NONE', #34787, 1000.000000000000000 ) ;
#26257 = CARTESIAN_POINT ( 'NONE',  ( 31.09745072740910388, 83.47442710120324705, -5.000000000000011546 ) ) ;
#26258 = CARTESIAN_POINT ( 'NONE',  ( 3.000000000000000000, -1.467624384280027172, 2.542000000000001592 ) ) ;
#26259 = ORIENTED_EDGE ( 'NONE', *, *, #20342, .T. ) ;
#26260 = DIRECTION ( 'NONE',  ( -0.000000000000000000, -0.000000000000000000, -1.000000000000000000 ) ) ;
#26261 = ADVANCED_FACE ( 'NONE', ( #9211 ), #11198, .F. ) ;
#26262 = DIRECTION ( 'NONE',  ( 0.000000000000000000, 0.000000000000000000, 1.000000000000000000 ) ) ;
#26263 = AXIS2_PLACEMENT_3D ( 'NONE', #308, #28814, #35213 ) ;
#26264 = ORIENTED_EDGE ( 'NONE', *, *, #32534, .F. ) ;
#26265 = VERTEX_POINT ( 'NONE', #1901 ) ;
#26266 = EDGE_CURVE ( 'NONE', #6635, #7505, #6404, .T. ) ;
#26267 = DIRECTION ( 'NONE',  ( 0.000000000000000000, 0.000000000000000000, -1.000000000000000000 ) ) ;
#26268 = AXIS2_PLACEMENT_3D ( 'NONE', #27189, #1506, #30192 ) ;
#26269 = DIRECTION ( 'NONE',  ( 0.8660254037844337116, -0.5000000000000084377, 0.000000000000000000 ) ) ;
#26270 = CARTESIAN_POINT ( 'NONE',  ( 52.39915983220795681, 35.19434990244919703, -4.999999999999997335 ) ) ;
#26271 = DIRECTION ( 'NONE',  ( 1.000000000000000000, 0.000000000000000000, 0.000000000000000000 ) ) ;
#26272 = ORIENTED_EDGE ( 'NONE', *, *, #30255, .F. ) ;
#26273 = VECTOR ( 'NONE', #15640, 1000.000000000000000 ) ;
#26274 = FACE_OUTER_BOUND ( 'NONE', #17003, .T. ) ;
#26275 = FACE_OUTER_BOUND ( 'NONE', #33794, .T. ) ;
#26276 = DIRECTION ( 'NONE',  ( 0.000000000000000000, 0.000000000000000000, 1.000000000000000000 ) ) ;
#26277 = ORIENTED_EDGE ( 'NONE', *, *, #12263, .F. ) ;
#26278 = CIRCLE ( 'NONE', #31072, 25.00000000000000000 ) ;
#26279 = ADVANCED_FACE ( 'NONE', ( #27195 ), #5831, .F. ) ;
#26280 = CARTESIAN_POINT ( 'NONE',  ( -60.00000337463108480, -51.96152422706641971, 17.49999999999999645 ) ) ;
#26281 = ORIENTED_EDGE ( 'NONE', *, *, #14400, .T. ) ;
#26282 = CIRCLE ( 'NONE', #19703, 6.000000000000005329 ) ;
#26283 = DIRECTION ( 'NONE',  ( 0.000000000000000000, 0.000000000000000000, 1.000000000000000000 ) ) ;
#26284 = FACE_OUTER_BOUND ( 'NONE', #2740, .T. ) ;
#26285 = CIRCLE ( 'NONE', #28081, 2.000000000000001776 ) ;
#26286 = LINE ( 'NONE', #12011, #28618 ) ;
#26287 = ORIENTED_EDGE ( 'NONE', *, *, #29972, .T. ) ;
#26288 = EDGE_LOOP ( 'NONE', ( #14006, #12676, #7598, #21467 ) ) ;
#26289 = FACE_OUTER_BOUND ( 'NONE', #13627, .T. ) ;
#26290 = EDGE_CURVE ( 'NONE', #26576, #9227, #7166, .T. ) ;
#26291 = DIRECTION ( 'NONE',  ( 0.000000000000000000, 0.000000000000000000, 1.000000000000000000 ) ) ;
#26292 = DIRECTION ( 'NONE',  ( 1.000000000000000000, 0.000000000000000000, 0.000000000000000000 ) ) ;
#26293 = VERTEX_POINT ( 'NONE', #23857 ) ;
#26294 = LINE ( 'NONE', #12019, #33936 ) ;
#26295 = CIRCLE ( 'NONE', #24517, 2.000000000000001776 ) ;
#26296 = EDGE_CURVE ( 'NONE', #27651, #23728, #10625, .T. ) ;
#26297 = FACE_BOUND ( 'NONE', #8985, .T. ) ;
#26298 = AXIS2_PLACEMENT_3D ( 'NONE', #22276, #33349, #24352 ) ;
#26299 = DIRECTION ( 'NONE',  ( 1.000000000000000000, 0.000000000000000000, 0.000000000000000000 ) ) ;
#26300 = FACE_OUTER_BOUND ( 'NONE', #30414, .T. ) ;
#26301 = CARTESIAN_POINT ( 'NONE',  ( 44.99999662536851019, 77.94228634059959404, -5.000000000000000000 ) ) ;
#26302 = ORIENTED_EDGE ( 'NONE', *, *, #25267, .T. ) ;
#26303 = DIRECTION ( 'NONE',  ( -1.000000000000000000, 0.000000000000000000, 0.000000000000000000 ) ) ;
#26304 = CARTESIAN_POINT ( 'NONE',  ( 76.99999662536836809, -8.660254037844401509, -9.999999999999998224 ) ) ;
#26305 = DIRECTION ( 'NONE',  ( 0.000000000000000000, 0.000000000000000000, 1.000000000000000000 ) ) ;
#26306 = ORIENTED_EDGE ( 'NONE', *, *, #21242, .T. ) ;
#26307 = LINE ( 'NONE', #619, #28605 ) ;
#26308 = EDGE_CURVE ( 'NONE', #29824, #26391, #2838, .T. ) ;
#26309 = CARTESIAN_POINT ( 'NONE',  ( -3.499999647538295289, 4.028415724610438176, -4.085927688751829656 ) ) ;
#26310 = CARTESIAN_POINT ( 'NONE',  ( -8.000003374631278419, -69.28203230275519786, -5.000000000000000000 ) ) ;
#26311 = AXIS2_PLACEMENT_3D ( 'NONE', #25644, #14550, #16834 ) ;
#26312 = EDGE_LOOP ( 'NONE', ( #5549, #18455, #3024, #12736 ) ) ;
#26313 = ORIENTED_EDGE ( 'NONE', *, *, #16201, .T. ) ;
#26314 = CIRCLE ( 'NONE', #3563, 2.445500000000000007 ) ;
#26315 = EDGE_LOOP ( 'NONE', ( #18484, #28517, #12205, #948 ) ) ;
#26316 = ADVANCED_FACE ( 'NONE', ( #35854 ), #18605, .F. ) ;
#26317 = CARTESIAN_POINT ( 'NONE',  ( -73.00000337463097821, -8.660254037844422825, -9.999999999999998224 ) ) ;
#26318 = LINE ( 'NONE', #14878, #33734 ) ;
#26319 = CIRCLE ( 'NONE', #31105, 2.000000000000001776 ) ;
#26320 = CARTESIAN_POINT ( 'NONE',  ( -92.00000337463090716, -1.016341149603137227E-14, 17.49999999999999645 ) ) ;
#26321 = ORIENTED_EDGE ( 'NONE', *, *, #32534, .T. ) ;
#26322 = VERTEX_POINT ( 'NONE', #21765 ) ;
#26323 = DIRECTION ( 'NONE',  ( -1.000000000000000000, 0.000000000000000000, 0.000000000000000000 ) ) ;
#26324 = CIRCLE ( 'NONE', #23331, 2.000000000000001776 ) ;
#26325 = EDGE_LOOP ( 'NONE', ( #36234, #31365, #27243, #18254 ) ) ;
#26326 = CYLINDRICAL_SURFACE ( 'NONE', #6001, 2.000000000000000000 ) ;
#26327 = ORIENTED_EDGE ( 'NONE', *, *, #29661, .F. ) ;
#26328 = DIRECTION ( 'NONE',  ( 0.000000000000000000, 0.000000000000000000, 1.000000000000000000 ) ) ;
#26329 = VERTEX_POINT ( 'NONE', #26848 ) ;
#26330 = ORIENTED_EDGE ( 'NONE', *, *, #25173, .F. ) ;
#26331 = EDGE_CURVE ( 'NONE', #29105, #29077, #35760, .T. ) ;
#26332 = DIRECTION ( 'NONE',  ( 1.000000000000000000, 0.000000000000000000, 0.000000000000000000 ) ) ;
#26333 = CARTESIAN_POINT ( 'NONE',  ( 4.999999999999999112, -2.886751345948144198, -5.700000000000000178 ) ) ;
#26334 = DIRECTION ( 'NONE',  ( 0.000000000000000000, 0.000000000000000000, 1.000000000000000000 ) ) ;
#26335 = ORIENTED_EDGE ( 'NONE', *, *, #26338, .T. ) ;
#26336 = FACE_OUTER_BOUND ( 'NONE', #2643, .T. ) ;
#26337 = CIRCLE ( 'NONE', #14963, 2.000000000000001776 ) ;
#26338 = EDGE_CURVE ( 'NONE', #8840, #30504, #19590, .T. ) ;
#26339 = LINE ( 'NONE', #11346, #22849 ) ;
#26340 = DIRECTION ( 'NONE',  ( 0.000000000000000000, 0.000000000000000000, 1.000000000000000000 ) ) ;
#26341 = VECTOR ( 'NONE', #9753, 1000.000000000000000 ) ;
#26342 = EDGE_LOOP ( 'NONE', ( #31706, #26420 ) ) ;
#26343 = DIRECTION ( 'NONE',  ( 0.000000000000000000, 0.000000000000000000, 1.000000000000000000 ) ) ;
#26344 = CARTESIAN_POINT ( 'NONE',  ( 67.99999662536836809, -51.96152422706639840, 17.49999999999999645 ) ) ;
#26346 = ORIENTED_EDGE ( 'NONE', *, *, #31640, .T. ) ;
#26345 = EDGE_CURVE ( 'NONE', #15626, #17730, #27022, .T. ) ;
#26347 = CARTESIAN_POINT ( 'NONE',  ( -47.00000337463112743, -60.62177826491080168, 17.49999999999999645 ) ) ;
#26348 = CYLINDRICAL_SURFACE ( 'NONE', #16095, 25.00000000000000711 ) ;
#26349 = CARTESIAN_POINT ( 'NONE',  ( -83.00000337463092137, 8.660254037844389075, -9.999999999999998224 ) ) ;
#26350 = DIRECTION ( 'NONE',  ( -1.000000000000000000, 0.000000000000000000, 0.000000000000000000 ) ) ;
#26351 = CARTESIAN_POINT ( 'NONE',  ( 2.778182860042563540, -69.13212189986967360, -49.86348611802629449 ) ) ;
#26352 = DIRECTION ( 'NONE',  ( 1.000000000000000000, 0.000000000000000000, 0.000000000000000000 ) ) ;
#26353 = ORIENTED_EDGE ( 'NONE', *, *, #20843, .T. ) ;
#26354 = DIRECTION ( 'NONE',  ( -1.000000000000000000, 0.000000000000000000, 0.000000000000000000 ) ) ;
#26355 = AXIS2_PLACEMENT_3D ( 'NONE', #2541, #31582, #30837 ) ;
#26356 = DIRECTION ( 'NONE',  ( -1.000000000000000000, 0.000000000000000000, 0.000000000000000000 ) ) ;
#26357 = DIRECTION ( 'NONE',  ( 1.000000000000000000, 0.000000000000000000, 0.000000000000000000 ) ) ;
#26358 = ORIENTED_EDGE ( 'NONE', *, *, #19700, .F. ) ;
#26359 = ORIENTED_EDGE ( 'NONE', *, *, #30184, .F. ) ;
#26360 = ORIENTED_EDGE ( 'NONE', *, *, #9239, .F. ) ;
#26361 = ADVANCED_FACE ( 'NONE', ( #7522 ), #10167, .F. ) ;
#26362 = DIRECTION ( 'NONE',  ( 0.000000000000000000, 0.000000000000000000, 1.000000000000000000 ) ) ;
#26363 = FACE_OUTER_BOUND ( 'NONE', #715, .T. ) ;
#26364 = AXIS2_PLACEMENT_3D ( 'NONE', #29468, #24745, #3788 ) ;
#26365 = FACE_OUTER_BOUND ( 'NONE', #21549, .T. ) ;
#26366 = AXIS2_PLACEMENT_3D ( 'NONE', #19498, #23233, #19864 ) ;
#26367 = DIRECTION ( 'NONE',  ( 0.000000000000000000, 0.000000000000000000, -1.000000000000000000 ) ) ;
#26368 = ORIENTED_EDGE ( 'NONE', *, *, #12627, .F. ) ;
#26369 = AXIS2_PLACEMENT_3D ( 'NONE', #36769, #33776, #22332 ) ;
#26370 = CARTESIAN_POINT ( 'NONE',  ( 24.99999662536859546, -77.94228634059960825, 17.49999999999999645 ) ) ;
#26371 = ORIENTED_EDGE ( 'NONE', *, *, #1567, .F. ) ;
#26373 = AXIS2_PLACEMENT_3D ( 'NONE', #15001, #26426, #35054 ) ;
#26372 = FACE_BOUND ( 'NONE', #30032, .T. ) ;
#26374 = EDGE_CURVE ( 'NONE', #34855, #30183, #26167, .T. ) ;
#26375 = LINE ( 'NONE', #3302, #32299 ) ;
#26376 = LINE ( 'NONE', #3096, #20277 ) ;
#26377 = EDGE_CURVE ( 'NONE', #911, #10350, #25005, .T. ) ;
#26378 = VERTEX_POINT ( 'NONE', #24037 ) ;
#26379 = DIRECTION ( 'NONE',  ( -1.000000000000000000, -0.000000000000000000, -0.000000000000000000 ) ) ;
#26380 = SHAPE_DEFINITION_REPRESENTATION ( #25928, #22738 ) ;
#26381 = ADVANCED_FACE ( 'NONE', ( #15774 ), #35655, .F. ) ;
#26382 = DIRECTION ( 'NONE',  ( 1.000000000000000000, 0.000000000000000000, 0.000000000000000000 ) ) ;
#26383 = CARTESIAN_POINT ( 'NONE',  ( 21.99999662536859191, 69.28203230275516944, -9.999999999999998224 ) ) ;
#26384 = DIRECTION ( 'NONE',  ( 0.000000000000000000, -0.000000000000000000, -1.000000000000000000 ) ) ;
#26385 = EDGE_LOOP ( 'NONE', ( #1741, #33403, #22952, #1616 ) ) ;
#26386 = CARTESIAN_POINT ( 'NONE',  ( 16.99999662536863454, -77.94228634059960825, -9.999999999999998224 ) ) ;
#26387 = EDGE_CURVE ( 'NONE', #9129, #35778, #15411, .T. ) ;
#26388 = LINE ( 'NONE', #26202, #5279 ) ;
#26389 = FACE_OUTER_BOUND ( 'NONE', #1834, .T. ) ;
#26390 = EDGE_CURVE ( 'NONE', #3002, #1135, #12382, .T. ) ;
#26391 = VERTEX_POINT ( 'NONE', #32639 ) ;
#26392 = EDGE_LOOP ( 'NONE', ( #35420, #14146, #14182, #17220, #9714 ) ) ;
#26393 = VECTOR ( 'NONE', #28648, 1000.000000000000000 ) ;
#26394 = ORIENTED_EDGE ( 'NONE', *, *, #3901, .T. ) ;
#26395 = DIRECTION ( 'NONE',  ( -1.000000000000000000, -0.000000000000000000, -0.000000000000000000 ) ) ;
#26396 = ADVANCED_FACE ( 'NONE', ( #30022 ), #30196, .T. ) ;
#26397 = EDGE_CURVE ( 'NONE', #3085, #6951, #19333, .T. ) ;
#26398 = DIRECTION ( 'NONE',  ( 0.000000000000000000, 0.000000000000000000, -1.000000000000000000 ) ) ;
#26399 = EDGE_CURVE ( 'NONE', #5530, #35823, #24382, .T. ) ;
#26400 = EDGE_CURVE ( 'NONE', #28159, #27693, #33969, .T. ) ;
#26401 = CARTESIAN_POINT ( 'NONE',  ( -75.00000337463097821, -8.660254037844422825, 17.49999999999999645 ) ) ;
#26402 = CARTESIAN_POINT ( 'NONE',  ( 6.999996625368676284, -77.94228634059960825, -9.999999999999998224 ) ) ;
#26403 = DIRECTION ( 'NONE',  ( 0.000000000000000000, 0.000000000000000000, 1.000000000000000000 ) ) ;
#26404 = CYLINDRICAL_SURFACE ( 'NONE', #11386, 2.000000000000000000 ) ;
#26405 = EDGE_LOOP ( 'NONE', ( #5985, #21231, #29906, #7705 ) ) ;
#26406 = VERTEX_POINT ( 'NONE', #2274 ) ;
#26407 = CYLINDRICAL_SURFACE ( 'NONE', #2699, 5.000000000000000000 ) ;
#26408 = DIRECTION ( 'NONE',  ( 1.000000000000000000, 0.000000000000000000, 0.000000000000000000 ) ) ;
#26409 = DIRECTION ( 'NONE',  ( 1.000000000000000000, 0.000000000000000000, 0.000000000000000000 ) ) ;
#26410 = EDGE_LOOP ( 'NONE', ( #19129, #17338, #12492, #32865 ) ) ;
#26411 = FACE_BOUND ( 'NONE', #28424, .T. ) ;
#26412 = ORIENTED_EDGE ( 'NONE', *, *, #11014, .F. ) ;
#26413 = EDGE_LOOP ( 'NONE', ( #36901, #34057 ) ) ;
#26414 = DIRECTION ( 'NONE',  ( 0.000000000000000000, 0.000000000000000000, -1.000000000000000000 ) ) ;
#26415 = VERTEX_POINT ( 'NONE', #33404 ) ;
#26416 =( LENGTH_UNIT ( ) NAMED_UNIT ( * ) SI_UNIT ( .MILLI., .METRE. ) );
#26417 = DIRECTION ( 'NONE',  ( 0.000000000000000000, 0.000000000000000000, -1.000000000000000000 ) ) ;
#26418 = CARTESIAN_POINT ( 'NONE',  ( -55.00000337463107059, 60.62177826491078747, -9.999999999999998224 ) ) ;
#26419 = CARTESIAN_POINT ( 'NONE',  ( 3.000000000000000000, 1.467624384280024730, -2.542000000000001592 ) ) ;
#26420 = ORIENTED_EDGE ( 'NONE', *, *, #1683, .T. ) ;
#26421 = ORIENTED_EDGE ( 'NONE', *, *, #21004, .T. ) ;
#26422 = VERTEX_POINT ( 'NONE', #5283 ) ;
#26423 = VERTEX_POINT ( 'NONE', #30587 ) ;
#26424 = ORIENTED_EDGE ( 'NONE', *, *, #34442, .T. ) ;
#26425 = CARTESIAN_POINT ( 'NONE',  ( 0.000000000000000000, 89.94802294027088863, -19.99999999999999645 ) ) ;
#26426 = DIRECTION ( 'NONE',  ( 0.000000000000000000, 0.000000000000000000, 1.000000000000000000 ) ) ;
#26427 = ORIENTED_EDGE ( 'NONE', *, *, #23362, .T. ) ;
#26428 = CIRCLE ( 'NONE', #16255, 2.000000000000001776 ) ;
#26429 = DIRECTION ( 'NONE',  ( 0.000000000000000000, 0.000000000000000000, 1.000000000000000000 ) ) ;
#26430 = CARTESIAN_POINT ( 'NONE',  ( 106.3598707460134989, 54.82082426949677512, 32.50000000000000000 ) ) ;
#26431 = DIRECTION ( 'NONE',  ( -1.000000000000000000, -0.000000000000000000, -0.000000000000000000 ) ) ;
#26432 = EDGE_LOOP ( 'NONE', ( #36981, #26868, #14615, #11403 ) ) ;
#26433 = CARTESIAN_POINT ( 'NONE',  ( -22.00000337463124112, -86.60254037844400443, -9.999999999999998224 ) ) ;
#26434 = DIRECTION ( 'NONE',  ( 1.000000000000000000, 0.000000000000000000, 0.000000000000000000 ) ) ;
#26435 = EDGE_CURVE ( 'NONE', #1584, #23264, #30364, .T. ) ;
#26436 = CARTESIAN_POINT ( 'NONE',  ( 69.99999662536839651, 34.64101615137758472, -9.999999999999998224 ) ) ;
#26437 = VERTEX_POINT ( 'NONE', #19518 ) ;
#26438 = DIRECTION ( 'NONE',  ( 0.000000000000000000, 0.000000000000000000, 1.000000000000000000 ) ) ;
#26439 = DIRECTION ( 'NONE',  ( 1.000000000000000000, 0.000000000000000000, 0.000000000000000000 ) ) ;
#26440 = ORIENTED_EDGE ( 'NONE', *, *, #15595, .F. ) ;
#26441 = ORIENTED_EDGE ( 'NONE', *, *, #1313, .T. ) ;
#26442 = CARTESIAN_POINT ( 'NONE',  ( 62.97617850287784336, 4.279621169095339184, -4.999999999999997335 ) ) ;
#26443 = DIRECTION ( 'NONE',  ( 0.000000000000000000, 0.000000000000000000, -1.000000000000000000 ) ) ;
#26444 = DIRECTION ( 'NONE',  ( -0.000000000000000000, 0.000000000000000000, -1.000000000000000000 ) ) ;
#26445 = CARTESIAN_POINT ( 'NONE',  ( -101.4249800177817207, -31.43204461043823272, 32.50002500000000083 ) ) ;
#26446 = ORIENTED_EDGE ( 'NONE', *, *, #31527, .T. ) ;
#26447 = DIRECTION ( 'NONE',  ( 0.000000000000000000, 0.000000000000000000, 1.000000000000000000 ) ) ;
#26448 = CARTESIAN_POINT ( 'NONE',  ( 74.99999662536836809, -8.660254037844401509, -9.999999999999998224 ) ) ;
#26449 = ORIENTED_EDGE ( 'NONE', *, *, #15537, .F. ) ;
#26450 = VECTOR ( 'NONE', #18645, 1000.000000000000000 ) ;
#26451 = LINE ( 'NONE', #14640, #26159 ) ;
#26452 = ORIENTED_EDGE ( 'NONE', *, *, #32497, .F. ) ;
#26453 = EDGE_CURVE ( 'NONE', #28884, #7742, #29766, .T. ) ;
#26454 = EDGE_CURVE ( 'NONE', #32590, #35393, #28569, .T. ) ;
#26455 = LINE ( 'NONE', #6395, #22302 ) ;
#26456 = DIRECTION ( 'NONE',  ( 0.000000000000000000, 0.000000000000000000, 1.000000000000000000 ) ) ;
#26457 = DIRECTION ( 'NONE',  ( -0.000000000000000000, -0.000000000000000000, 1.000000000000000000 ) ) ;
#26458 = VERTEX_POINT ( 'NONE', #33767 ) ;
#26459 = ORIENTED_EDGE ( 'NONE', *, *, #4433, .T. ) ;
#26460 = CARTESIAN_POINT ( 'NONE',  ( -57.00000337463107059, 60.62177826491078747, 12.50000000000000000 ) ) ;
#26461 = CARTESIAN_POINT ( 'NONE',  ( -106.0139304841753329, 39.63070125058630566, 32.50000000000000000 ) ) ;
#26462 = DIRECTION ( 'NONE',  ( 0.000000000000000000, 0.000000000000000000, -1.000000000000000000 ) ) ;
#26463 = ADVANCED_FACE ( 'NONE', ( #5624 ), #5076, .F. ) ;
#26464 = ORIENTED_EDGE ( 'NONE', *, *, #11445, .F. ) ;
#26465 = DIRECTION ( 'NONE',  ( 0.000000000000000000, 0.000000000000000000, 1.000000000000000000 ) ) ;
#26466 = FACE_BOUND ( 'NONE', #32703, .T. ) ;
#26467 = CARTESIAN_POINT ( 'NONE',  ( 2.500000000000000444, 0.000000000000000000, -5.324496230895142901 ) ) ;
#26468 = CARTESIAN_POINT ( 'NONE',  ( 51.13139720814417899, 27.49999999999988987, -10.00000000000000178 ) ) ;
#26469 = LINE ( 'NONE', #3777, #36296 ) ;
#26470 = VERTEX_POINT ( 'NONE', #19880 ) ;
#26471 = DIRECTION ( 'NONE',  ( -1.000000000000000000, 0.000000000000000000, 0.000000000000000000 ) ) ;
#26472 = CYLINDRICAL_SURFACE ( 'NONE', #9589, 2.000000000000001776 ) ;
#26473 = VECTOR ( 'NONE', #28548, 1000.000000000000000 ) ;
#26474 = EDGE_CURVE ( 'NONE', #27967, #5647, #29738, .T. ) ;
#26475 =( NAMED_UNIT ( * ) PLANE_ANGLE_UNIT ( ) SI_UNIT ( $, .RADIAN. ) );
#26476 = VERTEX_POINT ( 'NONE', #33960 ) ;
#26477 = DIRECTION ( 'NONE',  ( 0.000000000000000000, 0.000000000000000000, 1.000000000000000000 ) ) ;
#26478 = CARTESIAN_POINT ( 'NONE',  ( -90.60231327712325822, -15.97563234535699017, -4.999999999999997335 ) ) ;
#26479 = CARTESIAN_POINT ( 'NONE',  ( -62.33939050065184517, 13.89091430021398565, 12.49999999999999822 ) ) ;
#26480 = ORIENTED_EDGE ( 'NONE', *, *, #24863, .F. ) ;
#26481 = VERTEX_POINT ( 'NONE', #25327 ) ;
#26482 = ORIENTED_EDGE ( 'NONE', *, *, #13643, .T. ) ;
#26483 = CARTESIAN_POINT ( 'NONE',  ( 4.598786737361995947, -3.118391931134647077, -0.4203182062997404822 ) ) ;
#26484 = DIRECTION ( 'NONE',  ( 1.000000000000000000, 0.000000000000000000, 0.000000000000000000 ) ) ;
#26485 = DIRECTION ( 'NONE',  ( 1.000000000000000000, 0.000000000000000000, 0.000000000000000000 ) ) ;
#26486 = ORIENTED_EDGE ( 'NONE', *, *, #13539, .F. ) ;
#26487 = ORIENTED_EDGE ( 'NONE', *, *, #28214, .F. ) ;
#26488 = EDGE_LOOP ( 'NONE', ( #7857, #19123, #19623, #10276 ) ) ;
#26489 = DIRECTION ( 'NONE',  ( -1.000000000000000000, 0.000000000000000000, 0.000000000000000000 ) ) ;
#26490 = AXIS2_PLACEMENT_3D ( 'NONE', #3080, #9056, #32099 ) ;
#26491 = ORIENTED_EDGE ( 'NONE', *, *, #33875, .F. ) ;
#26492 = EDGE_CURVE ( 'NONE', #4407, #24647, #15408, .T. ) ;
#26493 = CARTESIAN_POINT ( 'NONE',  ( 10.49241169935725537, -117.7011479744511746, 32.50000000000000000 ) ) ;
#26494 = VERTEX_POINT ( 'NONE', #8276 ) ;
#26495 = CARTESIAN_POINT ( 'NONE',  ( -94.55012560584668790, 9.234378588655390629, 27.50000000000000000 ) ) ;
#26496 = ORIENTED_EDGE ( 'NONE', *, *, #36239, .F. ) ;
#26497 = EDGE_CURVE ( 'NONE', #31244, #16882, #27754, .T. ) ;
#26498 = ORIENTED_EDGE ( 'NONE', *, *, #6322, .T. ) ;
#26499 = DIRECTION ( 'NONE',  ( 1.000000000000000000, 0.000000000000000000, 0.000000000000000000 ) ) ;
#26500 = FACE_BOUND ( 'NONE', #6610, .T. ) ;
#26501 = AXIS2_PLACEMENT_3D ( 'NONE', #35449, #6366, #23442 ) ;
#26502 = DIRECTION ( 'NONE',  ( -1.000000000000000000, 0.000000000000000000, 0.000000000000000000 ) ) ;
#26503 = ORIENTED_EDGE ( 'NONE', *, *, #1109, .T. ) ;
#26504 = VECTOR ( 'NONE', #25220, 1000.000000000000000 ) ;
#26505 = ADVANCED_FACE ( 'NONE', ( #16887 ), #13324, .F. ) ;
#26506 = EDGE_LOOP ( 'NONE', ( #504, #1525 ) ) ;
#26507 = CARTESIAN_POINT ( 'NONE',  ( 0.000000000000000000, 0.000000000000000000, -5.674599999999998090 ) ) ;
#26508 = CONTEXT_DEPENDENT_SHAPE_REPRESENTATION ( #20931, #15782 ) ;
#26509 = DIRECTION ( 'NONE',  ( -1.000000000000000000, 0.000000000000000000, 0.000000000000000000 ) ) ;
#26510 = LINE ( 'NONE', #9256, #26256 ) ;
#26511 = EDGE_CURVE ( 'NONE', #22230, #7750, #18382, .T. ) ;
#26512 = ORIENTED_EDGE ( 'NONE', *, *, #25228, .T. ) ;
#26513 = CARTESIAN_POINT ( 'NONE',  ( -55.27226924886021919, 77.26562141134635908, 32.50000000000000000 ) ) ;
#26514 = CARTESIAN_POINT ( 'NONE',  ( 0.000000000000000000, 0.000000000000000000, -10.00000000000000000 ) ) ;
#26515 = VERTEX_POINT ( 'NONE', #14057 ) ;
#26516 = DIRECTION ( 'NONE',  ( 0.000000000000000000, 0.000000000000000000, 1.000000000000000000 ) ) ;
#26517 = CARTESIAN_POINT ( 'NONE',  ( 74.99999662536836809, 43.30127018922198801, -9.999999999999998224 ) ) ;
#26518 = FACE_OUTER_BOUND ( 'NONE', #21759, .T. ) ;
#26519 = DIRECTION ( 'NONE',  ( 0.000000000000000000, 0.000000000000000000, -1.000000000000000000 ) ) ;
#26520 = CIRCLE ( 'NONE', #27106, 2.000000000000001776 ) ;
#26521 = DIRECTION ( 'NONE',  ( 0.000000000000000000, 0.000000000000000000, 1.000000000000000000 ) ) ;
#26522 = CARTESIAN_POINT ( 'NONE',  ( -37.50000000000000000, 103.4105893997321886, 27.49999999999999645 ) ) ;
#26523 = EDGE_LOOP ( 'NONE', ( #19748, #34937 ) ) ;
#26524 = DIRECTION ( 'NONE',  ( 0.000000000000000000, 0.000000000000000000, 1.000000000000000000 ) ) ;
#26525 = CARTESIAN_POINT ( 'NONE',  ( 3.500188911486798560, 4.028306647601576529, -4.085926550512734678 ) ) ;
#26526 = DIRECTION ( 'NONE',  ( 1.000000000000000000, 0.000000000000000000, 0.000000000000000000 ) ) ;
#26527 = VERTEX_POINT ( 'NONE', #8452 ) ;
#26528 = EDGE_CURVE ( 'NONE', #12167, #3559, #13508, .T. ) ;
#26529 = VERTEX_POINT ( 'NONE', #24971 ) ;
#26530 = VERTEX_POINT ( 'NONE', #11062 ) ;
#26531 = AXIS2_PLACEMENT_3D ( 'NONE', #32341, #24089, #32702 ) ;
#26532 = DIRECTION ( 'NONE',  ( 1.000000000000000000, 0.000000000000000000, 0.000000000000000000 ) ) ;
#26533 = DIRECTION ( 'NONE',  ( 1.000000000000000000, 0.000000000000000000, 0.000000000000000000 ) ) ;
#26534 = LINE ( 'NONE', #34985, #27855 ) ;
#26535 = EDGE_CURVE ( 'NONE', #15669, #30855, #22581, .T. ) ;
#26536 = CARTESIAN_POINT ( 'NONE',  ( -13.00000337463125710, -77.94228634059960825, -9.999999999999998224 ) ) ;
#26537 = DIRECTION ( 'NONE',  ( 0.000000000000000000, 0.000000000000000000, 1.000000000000000000 ) ) ;
#26538 = ORIENTED_EDGE ( 'NONE', *, *, #879, .T. ) ;
#26539 = EDGE_CURVE ( 'NONE', #22136, #25902, #23788, .T. ) ;
#26540 = DIRECTION ( 'NONE',  ( 1.000000000000000000, 0.000000000000000000, 0.000000000000000000 ) ) ;
#26541 = EDGE_LOOP ( 'NONE', ( #4207, #24630 ) ) ;
#26542 = FACE_BOUND ( 'NONE', #30234, .T. ) ;
#26543 = VECTOR ( 'NONE', #12603, 1000.000000000000000 ) ;
#26544 = AXIS2_PLACEMENT_3D ( 'NONE', #31994, #25856, #20767 ) ;
#26545 = DIRECTION ( 'NONE',  ( 1.000000000000000000, 0.000000000000000000, 0.000000000000000000 ) ) ;
#26546 =( NAMED_UNIT ( * ) PLANE_ANGLE_UNIT ( ) SI_UNIT ( $, .RADIAN. ) );
#26547 = ORIENTED_EDGE ( 'NONE', *, *, #1951, .T. ) ;
#26548 = CARTESIAN_POINT ( 'NONE',  ( -77.00000337463099243, -25.98076211353322051, -9.999999999999998224 ) ) ;
#26549 = DIRECTION ( 'NONE',  ( 1.000000000000000000, 0.000000000000000000, 0.000000000000000000 ) ) ;
#26550 = VECTOR ( 'NONE', #23020, 1000.000000000000000 ) ;
#26551 = CYLINDRICAL_SURFACE ( 'NONE', #17077, 2.000000000000001776 ) ;
#26552 = EDGE_CURVE ( 'NONE', #34764, #12419, #9404, .T. ) ;
#26553 = FACE_OUTER_BOUND ( 'NONE', #1341, .T. ) ;
#26554 = DIRECTION ( 'NONE',  ( 1.000000000000000000, 0.000000000000000000, 0.000000000000000000 ) ) ;
#26555 = VERTEX_POINT ( 'NONE', #20593 ) ;
#26556 = CARTESIAN_POINT ( 'NONE',  ( 69.99999662536839651, 34.64101615137758472, -9.999999999999998224 ) ) ;
#26557 = LINE ( 'NONE', #12855, #3480 ) ;
#26558 = DIRECTION ( 'NONE',  ( 1.000000000000000000, 0.000000000000000000, 0.000000000000000000 ) ) ;
#26559 = CIRCLE ( 'NONE', #9181, 33.00000000000002132 ) ;
#26560 = ORIENTED_EDGE ( 'NONE', *, *, #36802, .F. ) ;
#26561 = ORIENTED_EDGE ( 'NONE', *, *, #24704, .F. ) ;
#26562 = ORIENTED_EDGE ( 'NONE', *, *, #26528, .T. ) ;
#26563 = LINE ( 'NONE', #12503, #6357 ) ;
#26564 = FACE_OUTER_BOUND ( 'NONE', #4281, .T. ) ;
#26565 = AXIS2_PLACEMENT_3D ( 'NONE', #2391, #19264, #19632 ) ;
#26566 = DIRECTION ( 'NONE',  ( -0.000000000000000000, 0.000000000000000000, -1.000000000000000000 ) ) ;
#26567 = EDGE_CURVE ( 'NONE', #32112, #27460, #33376, .T. ) ;
#26568 = ORIENTED_EDGE ( 'NONE', *, *, #26593, .T. ) ;
#26569 = CARTESIAN_POINT ( 'NONE',  ( -52.00000337463109190, 51.96152422706637708, -5.000000000000000000 ) ) ;
#26570 = CARTESIAN_POINT ( 'NONE',  ( -35.00000337463116296, 60.62177826491077326, -5.000000000000000000 ) ) ;
#26571 = EDGE_CURVE ( 'NONE', #25853, #2100, #1034, .T. ) ;
#26572 = DIRECTION ( 'NONE',  ( 0.000000000000000000, 0.000000000000000000, 1.000000000000000000 ) ) ;
#26573 = ORIENTED_EDGE ( 'NONE', *, *, #19299, .F. ) ;
#26574 = STYLED_ITEM ( 'NONE', ( #1419 ), #20313 ) ;
#26575 = ADVANCED_FACE ( 'NONE', ( #11792 ), #29032, .F. ) ;
#26576 = VERTEX_POINT ( 'NONE', #20054 ) ;
#26577 = CARTESIAN_POINT ( 'NONE',  ( 82.99999662536831124, -8.660254037844397956, -5.000000000000000000 ) ) ;
#26578 = CYLINDRICAL_SURFACE ( 'NONE', #9787, 30.00000000000000000 ) ;
#26579 = ORIENTED_EDGE ( 'NONE', *, *, #25447, .F. ) ;
#26580 = CARTESIAN_POINT ( 'NONE',  ( -5.211749180171792339, -2.764497899775295586, -4.027903350935058135 ) ) ;
#26581 = EDGE_CURVE ( 'NONE', #20688, #24345, #32611, .T. ) ;
#26582 = ORIENTED_EDGE ( 'NONE', *, *, #30935, .T. ) ;
#26583 = EDGE_CURVE ( 'NONE', #4105, #23009, #14265, .T. ) ;
#26584 = FACE_BOUND ( 'NONE', #32794, .T. ) ;
#26585 = ORIENTED_EDGE ( 'NONE', *, *, #3508, .F. ) ;
#26586 = ORIENTED_EDGE ( 'NONE', *, *, #26069, .F. ) ;
#26587 = DIRECTION ( 'NONE',  ( 0.000000000000000000, 0.000000000000000000, 1.000000000000000000 ) ) ;
#26588 = ORIENTED_EDGE ( 'NONE', *, *, #22761, .T. ) ;
#26589 = EDGE_CURVE ( 'NONE', #32244, #538, #14609, .T. ) ;
#26590 = SURFACE_STYLE_USAGE ( .BOTH. , #23987 ) ;
#26591 = ADVANCED_FACE ( 'NONE', ( #5824 ), #11436, .T. ) ;
#26592 = DIRECTION ( 'NONE',  ( -0.000000000000000000, -0.000000000000000000, 1.000000000000000000 ) ) ;
#26593 = EDGE_CURVE ( 'NONE', #10050, #34413, #23032, .T. ) ;
#26594 = CYLINDRICAL_SURFACE ( 'NONE', #4149, 3.000000000000000000 ) ;
#26595 = CARTESIAN_POINT ( 'NONE',  ( -2.499999999999996891, -4.330127018922233617, -3.620524600599889453 ) ) ;
#26596 = EDGE_LOOP ( 'NONE', ( #29575, #20844 ) ) ;
#26597 = EDGE_CURVE ( 'NONE', #10948, #28579, #1456, .T. ) ;
#26598 = EDGE_LOOP ( 'NONE', ( #4374, #36165, #25989, #26877 ) ) ;
#26599 = ORIENTED_EDGE ( 'NONE', *, *, #14653, .F. ) ;
#26600 = ORIENTED_EDGE ( 'NONE', *, *, #34929, .T. ) ;
#26601 = ORIENTED_EDGE ( 'NONE', *, *, #1024, .F. ) ;
#26602 = DIRECTION ( 'NONE',  ( 0.000000000000000000, 0.000000000000000000, 1.000000000000000000 ) ) ;
#26603 = AXIS2_PLACEMENT_3D ( 'NONE', #15009, #9741, #17612 ) ;
#26604 = CARTESIAN_POINT ( 'NONE',  ( 37.99999662536853151, -69.28203230275519786, -5.000000000000000000 ) ) ;
#26605 = ORIENTED_EDGE ( 'NONE', *, *, #11258, .T. ) ;
#26606 = DIRECTION ( 'NONE',  ( 1.000000000000000000, 0.000000000000000000, 0.000000000000000000 ) ) ;
#26607 = DIRECTION ( 'NONE',  ( 0.000000000000000000, 0.000000000000000000, 1.000000000000000000 ) ) ;
#26608 = DIRECTION ( 'NONE',  ( 0.000000000000000000, 0.000000000000000000, 1.000000000000000000 ) ) ;
#26609 = ORIENTED_EDGE ( 'NONE', *, *, #11713, .T. ) ;
#26610 = DIRECTION ( 'NONE',  ( 1.000000000000000000, 0.000000000000000000, 0.000000000000000000 ) ) ;
#26611 = DIRECTION ( 'NONE',  ( -0.000000000000000000, -0.000000000000000000, 1.000000000000000000 ) ) ;
#26612 = EDGE_CURVE ( 'NONE', #12595, #29485, #34422, .T. ) ;
#26613 = VECTOR ( 'NONE', #7528, 1000.000000000000000 ) ;
#26614 = DIRECTION ( 'NONE',  ( 1.000000000000000000, 0.000000000000000000, 0.000000000000000000 ) ) ;
#26615 = ORIENTED_EDGE ( 'NONE', *, *, #28174, .F. ) ;
#26616 = CARTESIAN_POINT ( 'NONE',  ( 34.99999662536855283, -77.94228634059960825, 17.49999999999999645 ) ) ;
#26617 = AXIS2_PLACEMENT_3D ( 'NONE', #19619, #28051, #14363 ) ;
#26618 = LINE ( 'NONE', #9574, #29748 ) ;
#26619 = EDGE_LOOP ( 'NONE', ( #31305, #35142, #7000 ) ) ;
#26620 = AXIS2_PLACEMENT_3D ( 'NONE', #10690, #1312, #9936 ) ;
#26621 = EDGE_LOOP ( 'NONE', ( #6284, #30115 ) ) ;
#26622 = DIRECTION ( 'NONE',  ( 1.000000000000000000, 0.000000000000000000, 0.000000000000000000 ) ) ;
#26623 = FACE_OUTER_BOUND ( 'NONE', #28113, .T. ) ;
#26624 = DIRECTION ( 'NONE',  ( -1.000000000000000000, 0.000000000000000000, 0.000000000000000000 ) ) ;
#26625 = DIRECTION ( 'NONE',  ( 0.000000000000000000, 0.000000000000000000, -1.000000000000000000 ) ) ;
#26626 = EDGE_CURVE ( 'NONE', #6836, #23569, #17036, .T. ) ;
#26627 = EDGE_LOOP ( 'NONE', ( #916, #428, #25837, #32989, #6310, #27582 ) ) ;
#26628 = VECTOR ( 'NONE', #35041, 1000.000000000000000 ) ;
#26629 = FACE_BOUND ( 'NONE', #6168, .T. ) ;
#26630 = CIRCLE ( 'NONE', #8065, 2.000000000000001776 ) ;
#26631 = DIRECTION ( 'NONE',  ( 0.000000000000000000, 0.000000000000000000, 1.000000000000000000 ) ) ;
#26632 = CIRCLE ( 'NONE', #6879, 2.000000000000001776 ) ;
#26633 = VECTOR ( 'NONE', #20022, 1000.000000000000000 ) ;
#26634 = ORIENTED_EDGE ( 'NONE', *, *, #15630, .F. ) ;
#26635 = LINE ( 'NONE', #1325, #18997 ) ;
#26636 = ORIENTED_EDGE ( 'NONE', *, *, #27190, .T. ) ;
#26637 = CARTESIAN_POINT ( 'NONE',  ( -30.00000337463118427, 69.28203230275516944, -5.000000000000000000 ) ) ;
#26638 = ADVANCED_FACE ( 'NONE', ( #34873 ), #6014, .F. ) ;
#26639 = DIRECTION ( 'NONE',  ( 1.000000000000000000, 0.000000000000000000, 0.000000000000000000 ) ) ;
#26640 = EDGE_CURVE ( 'NONE', #4245, #25195, #12825, .T. ) ;
#26641 = VECTOR ( 'NONE', #26991, 1000.000000000000000 ) ;
#26642 = CARTESIAN_POINT ( 'NONE',  ( 64.99999662536839651, -43.30127018922199511, -9.999999999999998224 ) ) ;
#26643 = EDGE_CURVE ( 'NONE', #29480, #33530, #3867, .T. ) ;
#26644 = ORIENTED_EDGE ( 'NONE', *, *, #11407, .F. ) ;
#26645 = AXIS2_PLACEMENT_3D ( 'NONE', #15267, #14717, #23360 ) ;
#26646 = EDGE_LOOP ( 'NONE', ( #26609, #8295, #35894, #29950, #22444 ) ) ;
#26647 = AXIS2_PLACEMENT_3D ( 'NONE', #15892, #29959, #21527 ) ;
#26648 = DIRECTION ( 'NONE',  ( 0.000000000000000000, 0.000000000000000000, 1.000000000000000000 ) ) ;
#26649 = VECTOR ( 'NONE', #8429, 1000.000000000000000 ) ;
#26650 = ORIENTED_EDGE ( 'NONE', *, *, #27860, .F. ) ;
#26651 = DIRECTION ( 'NONE',  ( 0.000000000000000000, 0.000000000000000000, -1.000000000000000000 ) ) ;
#26652 = DIRECTION ( 'NONE',  ( 0.000000000000000000, 0.000000000000000000, 1.000000000000000000 ) ) ;
#26653 = DIRECTION ( 'NONE',  ( 0.000000000000000000, 0.000000000000000000, 1.000000000000000000 ) ) ;
#26654 = CARTESIAN_POINT ( 'NONE',  ( 76.99999662536835388, -43.30127018922199511, 12.50000000000000000 ) ) ;
#26655 = DIRECTION ( 'NONE',  ( 1.000000000000000000, 0.000000000000000000, 0.000000000000000000 ) ) ;
#26656 = EDGE_LOOP ( 'NONE', ( #20930, #9449, #1551, #6081, #22260, #24130 ) ) ;
#26657 = DIRECTION ( 'NONE',  ( 0.000000000000000000, 0.000000000000000000, -1.000000000000000000 ) ) ;
#26658 = CIRCLE ( 'NONE', #26038, 2.000000000000001776 ) ;
#26659 = VECTOR ( 'NONE', #13271, 1000.000000000000000 ) ;
#26660 = CARTESIAN_POINT ( 'NONE',  ( 0.000000000000000000, 0.000000000000000000, 27.50000000000000000 ) ) ;
#26661 = B_SPLINE_CURVE_WITH_KNOTS ( 'NONE', 3,
 ( #19402, #5526, #30821, #34227, #16597, #8352, #31027, #16792, #13950, #25398, #34042, #19788, #26493, #35340, #11679, #23136, #3255, #805, #6632, #14684, #3637, #11873, #10149, #34589, #15065, #18060, #29481, #440, #8889, #3803, #3454, #14512, #31748, #25950, #23333 ),
 .UNSPECIFIED., .F., .F.,
 ( 4, 2, 1, 1, 2, 2, 1, 2, 2, 2, 2, 1, 2, 2, 1, 2, 2, 1, 1, 2, 4 ),
 ( 0.05563282717588803605, 0.06778080578339820694, 0.07992878439090839171, 0.1042247416059285114, 0.1163727202134385852, 0.1285206988209486867, 0.1528166560359688342, 0.1771126132509889817, 0.1892605918584991387, 0.2014085704660092402, 0.2500004848960496462, 0.2985923993260899412, 0.3107403779336000427, 0.3228883565411101442, 0.3471843137561303472, 0.3714802709711505502, 0.3836282495786607072, 0.3957762281861708642, 0.4200721854011910117, 0.4322201640087010577, 0.4443681426162111037 ),
 .UNSPECIFIED. ) ;
#26662 = DIRECTION ( 'NONE',  ( 0.000000000000000000, 0.000000000000000000, 1.000000000000000000 ) ) ;
#26663 = ORIENTED_EDGE ( 'NONE', *, *, #33811, .T. ) ;
#26664 = LINE ( 'NONE', #17666, #11832 ) ;
#26665 = FACE_BOUND ( 'NONE', #29230, .T. ) ;
#26666 = CARTESIAN_POINT ( 'NONE',  ( -65.00000337463106348, -60.62177826491083010, -9.999999999999998224 ) ) ;
#26667 = EDGE_CURVE ( 'NONE', #807, #21781, #28406, .T. ) ;
#26668 = ORIENTED_EDGE ( 'NONE', *, *, #23077, .T. ) ;
#26669 = ORIENTED_EDGE ( 'NONE', *, *, #35368, .F. ) ;
#26670 = AXIS2_PLACEMENT_3D ( 'NONE', #30830, #2715, #16414 ) ;
#26671 = CARTESIAN_POINT ( 'NONE',  ( -33.00000337463116296, 60.62177826491077326, -9.999999999999998224 ) ) ;
#26672 = FACE_OUTER_BOUND ( 'NONE', #34342, .T. ) ;
#26673 = DIRECTION ( 'NONE',  ( 1.000000000000000000, 0.000000000000000000, 0.000000000000000000 ) ) ;
#26674 = VERTEX_POINT ( 'NONE', #558 ) ;
#26675 = ORIENTED_EDGE ( 'NONE', *, *, #9061, .F. ) ;
#26676 = VERTEX_POINT ( 'NONE', #25709 ) ;
#26677 = CIRCLE ( 'NONE', #29662, 95.00000000000001421 ) ;
#26678 = VECTOR ( 'NONE', #30819, 1000.000000000000000 ) ;
#26679 = AXIS2_PLACEMENT_3D ( 'NONE', #3113, #3834, #3666 ) ;
#26680 = AXIS2_PLACEMENT_3D ( 'NONE', #14844, #12373, #14642 ) ;
#26681 = ORIENTED_EDGE ( 'NONE', *, *, #34659, .F. ) ;
#26682 = CARTESIAN_POINT ( 'NONE',  ( -70.00000337463100664, -17.32050807568882078, -5.000000000000000000 ) ) ;
#26683 = EDGE_LOOP ( 'NONE', ( #24594, #31110 ) ) ;
#26684 = DIRECTION ( 'NONE',  ( 0.000000000000000000, 0.000000000000000000, -1.000000000000000000 ) ) ;
#26685 = ORIENTED_EDGE ( 'NONE', *, *, #5523, .F. ) ;
#26686 = ORIENTED_EDGE ( 'NONE', *, *, #23643, .T. ) ;
#26687 = CYLINDRICAL_SURFACE ( 'NONE', #9454, 2.000000000000001776 ) ;
#26688 = DIRECTION ( 'NONE',  ( -0.5000000000000006661, 0.8660254037844382635, 0.000000000000000000 ) ) ;
#26689 = EDGE_CURVE ( 'NONE', #34742, #18010, #6363, .T. ) ;
#26690 = EDGE_LOOP ( 'NONE', ( #11242, #5401 ) ) ;
#26691 = ORIENTED_EDGE ( 'NONE', *, *, #26689, .T. ) ;
#26692 = DIRECTION ( 'NONE',  ( 0.000000000000000000, 0.000000000000000000, 1.000000000000000000 ) ) ;
#26693 = CARTESIAN_POINT ( 'NONE',  ( 5.029396762153803380, 2.903723574490927994, -4.151008977024205571 ) ) ;
#26694 = CARTESIAN_POINT ( 'NONE',  ( 5.999999999999985789, 149.8799519615616305, 32.55002500000000509 ) ) ;
#26695 = CARTESIAN_POINT ( 'NONE',  ( -23.49154088336464241, 103.5526315789473699, 32.50000000000000000 ) ) ;
#26696 = VERTEX_POINT ( 'NONE', #20795 ) ;
#26697 = DIRECTION ( 'NONE',  ( 0.000000000000000000, 0.000000000000000000, 1.000000000000000000 ) ) ;
#26698 = DIRECTION ( 'NONE',  ( 0.000000000000000000, 0.000000000000000000, -1.000000000000000000 ) ) ;
#26699 = ORIENTED_EDGE ( 'NONE', *, *, #28441, .T. ) ;
#26700 = CYLINDRICAL_SURFACE ( 'NONE', #22631, 2.000000000000001776 ) ;
#26701 = CIRCLE ( 'NONE', #32052, 1.999999999999998224 ) ;
#26702 = CARTESIAN_POINT ( 'NONE',  ( -70.00000337463099243, 51.96152422706637708, 17.49999999999999645 ) ) ;
#26703 = CARTESIAN_POINT ( 'NONE',  ( 29.99999662536857770, -69.28203230275519786, -9.999999999999998224 ) ) ;
#26704 = CIRCLE ( 'NONE', #23121, 1.999999999999998224 ) ;
#26705 = AXIS2_PLACEMENT_3D ( 'NONE', #6675, #35190, #10046 ) ;
#26706 = DIRECTION ( 'NONE',  ( 0.000000000000000000, 0.000000000000000000, 1.000000000000000000 ) ) ;
#26707 = AXIS2_PLACEMENT_3D ( 'NONE', #36646, #10940, #22380 ) ;
#26708 = CIRCLE ( 'NONE', #6360, 2.000000000000001776 ) ;
#26709 = DIRECTION ( 'NONE',  ( -1.000000000000000000, 0.000000000000000000, 0.000000000000000000 ) ) ;
#26710 = DIRECTION ( 'NONE',  ( 1.000000000000000000, 0.000000000000000000, 0.000000000000000000 ) ) ;
#26711 = VERTEX_POINT ( 'NONE', #32231 ) ;
#26712 = CARTESIAN_POINT ( 'NONE',  ( 76.99999662536836809, -8.660254037844401509, 12.50000000000000000 ) ) ;
#26713 = CARTESIAN_POINT ( 'NONE',  ( 54.99999662536844625, -60.62177826491080168, -9.999999999999998224 ) ) ;
#26714 = DIRECTION ( 'NONE',  ( 0.000000000000000000, 0.000000000000000000, 1.000000000000000000 ) ) ;
#26715 = EDGE_CURVE ( 'NONE', #36483, #32323, #2828, .T. ) ;
#26716 = EDGE_LOOP ( 'NONE', ( #1404, #32652, #3942, #6768 ) ) ;
#26717 = AXIS2_PLACEMENT_3D ( 'NONE', #16051, #1968, #24497 ) ;
#26718 = ORIENTED_EDGE ( 'NONE', *, *, #6209, .T. ) ;
#26719 = EDGE_LOOP ( 'NONE', ( #29889, #12501, #34495, #18124 ) ) ;
#26720 = DIRECTION ( 'NONE',  ( 0.000000000000000000, 0.000000000000000000, -1.000000000000000000 ) ) ;
#26721 = CARTESIAN_POINT ( 'NONE',  ( -10.00000337463128197, 86.60254037844397601, -5.000000000000000000 ) ) ;
#26722 = ADVANCED_FACE ( 'NONE', ( #12906 ), #35998, .T. ) ;
#26723 = DIRECTION ( 'NONE',  ( 1.000000000000000000, 0.000000000000000000, 0.000000000000000000 ) ) ;
#26724 = AXIS2_PLACEMENT_3D ( 'NONE', #29501, #15260, #29887 ) ;
#26725 = DIRECTION ( 'NONE',  ( 0.000000000000000000, 0.000000000000000000, 1.000000000000000000 ) ) ;
#26726 = EDGE_CURVE ( 'NONE', #7613, #1450, #36212, .T. ) ;
#26727 = AXIS2_PLACEMENT_3D ( 'NONE', #12392, #4347, #1725 ) ;
#26728 = LINE ( 'NONE', #36482, #33892 ) ;
#26729 = ORIENTED_EDGE ( 'NONE', *, *, #7083, .F. ) ;
#26730 = CARTESIAN_POINT ( 'NONE',  ( -4.242640687119340726, -4.242640687119236809, 27.50000000000000000 ) ) ;
#26731 = VERTEX_POINT ( 'NONE', #21553 ) ;
#26732 =( GEOMETRIC_REPRESENTATION_CONTEXT ( 3 ) GLOBAL_UNCERTAINTY_ASSIGNED_CONTEXT ( ( #15581 ) ) GLOBAL_UNIT_ASSIGNED_CONTEXT ( ( #26744, #9115, #14747 ) ) REPRESENTATION_CONTEXT ( 'NONE', 'WORKASPACE' ) );
#26733 = FACE_BOUND ( 'NONE', #18975, .T. ) ;
#26734 = AXIS2_PLACEMENT_3D ( 'NONE', #16041, #27818, #18846 ) ;
#26735 = CIRCLE ( 'NONE', #22534, 2.000000000000001776 ) ;
#26736 = AXIS2_PLACEMENT_3D ( 'NONE', #8963, #23213, #14962 ) ;
#26737 = AXIS2_PLACEMENT_3D ( 'NONE', #14870, #3786, #8680 ) ;
#26738 = CIRCLE ( 'NONE', #20155, 2.000000000000000000 ) ;
#26739 = CARTESIAN_POINT ( 'NONE',  ( -55.00000337463107059, 43.30127018922197379, 12.50000000000000000 ) ) ;
#26740 = CARTESIAN_POINT ( 'NONE',  ( -75.00000337463097821, 8.660254037844374864, 12.50000000000000000 ) ) ;
#26741 = EDGE_CURVE ( 'NONE', #19312, #2698, #12543, .T. ) ;
#26742 = ORIENTED_EDGE ( 'NONE', *, *, #34852, .F. ) ;
#26743 = CARTESIAN_POINT ( 'NONE',  ( 5.253368672218635460, 3.033033817057773529, -4.359491423763652840 ) ) ;
#26744 =( LENGTH_UNIT ( ) NAMED_UNIT ( * ) SI_UNIT ( .MILLI., .METRE. ) );
#26745 = VECTOR ( 'NONE', #15067, 1000.000000000000000 ) ;
#26746 = LINE ( 'NONE', #10245, #25460 ) ;
#26747 = DIRECTION ( 'NONE',  ( 0.000000000000000000, 0.000000000000000000, -1.000000000000000000 ) ) ;
#26748 = LINE ( 'NONE', #7252, #16142 ) ;
#26749 = EDGE_LOOP ( 'NONE', ( #1793, #29734, #661, #29986 ) ) ;
#26750 = DIRECTION ( 'NONE',  ( 0.000000000000000000, 0.000000000000000000, -1.000000000000000000 ) ) ;
#26751 = CARTESIAN_POINT ( 'NONE',  ( -44.13139720814380240, 27.50000000000055422, 5.000000000000000888 ) ) ;
#26752 = CARTESIAN_POINT ( 'NONE',  ( -60.00000337463108480, -51.96152422706641971, 17.49999999999999645 ) ) ;
#26753 = EDGE_CURVE ( 'NONE', #29492, #2026, #21834, .T. ) ;
#26754 = ORIENTED_EDGE ( 'NONE', *, *, #25638, .T. ) ;
#26755 = VERTEX_POINT ( 'NONE', #10812 ) ;
#26756 = AXIS2_PLACEMENT_3D ( 'NONE', #4691, #1680, #15366 ) ;
#26757 = EDGE_CURVE ( 'NONE', #34308, #24231, #24365, .T. ) ;
#26758 = EDGE_LOOP ( 'NONE', ( #992, #9399, #15166, #10356, #32014 ) ) ;
#26759 = PRODUCT_DEFINITION_FORMATION_WITH_SPECIFIED_SOURCE ( 'ANY', '', #5881, .NOT_KNOWN. ) ;
#26760 = DIRECTION ( 'NONE',  ( 1.000000000000000000, 0.000000000000000000, 0.000000000000000000 ) ) ;
#26761 = DIRECTION ( 'NONE',  ( 0.000000000000000000, 0.000000000000000000, 1.000000000000000000 ) ) ;
#26762 = CIRCLE ( 'NONE', #24360, 30.00000000000001421 ) ;
#26763 = EDGE_CURVE ( 'NONE', #27222, #4461, #17615, .T. ) ;
#26764 = CIRCLE ( 'NONE', #10603, 2.000000000000000000 ) ;
#26765 = DIRECTION ( 'NONE',  ( 0.000000000000000000, 0.000000000000000000, 1.000000000000000000 ) ) ;
#26766 = DIRECTION ( 'NONE',  ( 1.000000000000000000, 0.000000000000000000, 0.000000000000000000 ) ) ;
#26767 = DIRECTION ( 'NONE',  ( -0.5000000000000101030, -0.8660254037844329345, 0.000000000000000000 ) ) ;
#26768 = EDGE_CURVE ( 'NONE', #19268, #28791, #35006, .T. ) ;
#26769 = CARTESIAN_POINT ( 'NONE',  ( -5.000003374631307729, 77.94228634059957983, -9.999999999999998224 ) ) ;
#26770 = ORIENTED_EDGE ( 'NONE', *, *, #22748, .T. ) ;
#26771 = SHAPE_REPRESENTATION ( 'ventilated rotor', ( #21385 ), #23118 ) ;
#26772 = ORIENTED_EDGE ( 'NONE', *, *, #1387, .F. ) ;
#26773 = LINE ( 'NONE', #32395, #23655 ) ;
#26774 = EDGE_CURVE ( 'NONE', #545, #29294, #6249, .T. ) ;
#26775 = DIRECTION ( 'NONE',  ( 1.000000000000000000, 0.000000000000000000, 0.000000000000000000 ) ) ;
#26776 = ORIENTED_EDGE ( 'NONE', *, *, #28385, .F. ) ;
#26777 = CYLINDRICAL_SURFACE ( 'NONE', #7744, 27.00000000000001066 ) ;
#26778 = VERTEX_POINT ( 'NONE', #32416 ) ;
#26779 = AXIS2_PLACEMENT_3D ( 'NONE', #8328, #25563, #22558 ) ;
#26780 = VECTOR ( 'NONE', #30634, 1000.000000000000000 ) ;
#26781 = CARTESIAN_POINT ( 'NONE',  ( 0.000000000000000000, 89.94802294027094547, -24.99999999999999645 ) ) ;
#26782 = VERTEX_POINT ( 'NONE', #7119 ) ;
#26783 = EDGE_LOOP ( 'NONE', ( #24788, #8730, #12542, #14455 ) ) ;
#26784 = CARTESIAN_POINT ( 'NONE',  ( -9.974659986866640793E-15, -5.773502691896262640, -5.553418012614792509 ) ) ;
#26785 = ORIENTED_EDGE ( 'NONE', *, *, #11619, .F. ) ;
#26786 = FILL_AREA_STYLE ('',( #20781 ) ) ;
#26787 = AXIS2_PLACEMENT_3D ( 'NONE', #11955, #29201, #31815 ) ;
#26788 = DIRECTION ( 'NONE',  ( 0.000000000000000000, 0.000000000000000000, 1.000000000000000000 ) ) ;
#26789 = VECTOR ( 'NONE', #21241, 1000.000000000000000 ) ;
#26790 = ADVANCED_FACE ( 'NONE', ( #32595 ), #4122, .F. ) ;
#26791 = CARTESIAN_POINT ( 'NONE',  ( -58.00000337463108480, -51.96152422706641971, -9.999999999999998224 ) ) ;
#26792 = DIRECTION ( 'NONE',  ( 1.000000000000000000, 0.000000000000000000, 0.000000000000000000 ) ) ;
#26793 = ORIENTED_EDGE ( 'NONE', *, *, #23024, .T. ) ;
#26794 = ORIENTED_EDGE ( 'NONE', *, *, #812, .T. ) ;
#26795 = AXIS2_PLACEMENT_3D ( 'NONE', #20548, #18118, #29544 ) ;
#26796 = ORIENTED_EDGE ( 'NONE', *, *, #9758, .F. ) ;
#26797 = EDGE_CURVE ( 'NONE', #15626, #9129, #1673, .T. ) ;
#26798 = ORIENTED_EDGE ( 'NONE', *, *, #29393, .F. ) ;
#26799 = ORIENTED_EDGE ( 'NONE', *, *, #306, .F. ) ;
#26800 = CARTESIAN_POINT ( 'NONE',  ( -45.00000337463112743, -60.62177826491080168, 12.50000000000000000 ) ) ;
#26801 = AXIS2_PLACEMENT_3D ( 'NONE', #30683, #21878, #16093 ) ;
#26802 = EDGE_CURVE ( 'NONE', #32886, #24047, #27197, .T. ) ;
#26803 = DIRECTION ( 'NONE',  ( 0.000000000000000000, 0.000000000000000000, 1.000000000000000000 ) ) ;
#26804 = ORIENTED_EDGE ( 'NONE', *, *, #8537, .T. ) ;
#26805 = EDGE_CURVE ( 'NONE', #10468, #23471, #20608, .T. ) ;
#26806 = VECTOR ( 'NONE', #33525, 1000.000000000000000 ) ;
#26808 = AXIS2_PLACEMENT_3D ( 'NONE', #15969, #26653, #9963 ) ;
#26807 = DIRECTION ( 'NONE',  ( -0.000000000000000000, -0.000000000000000000, 1.000000000000000000 ) ) ;
#26809 = CARTESIAN_POINT ( 'NONE',  ( 21.99999662536862033, -69.28203230275519786, 17.49999999999999645 ) ) ;
#26810 = LINE ( 'NONE', #32805, #23767 ) ;
#26811 = ORIENTED_EDGE ( 'NONE', *, *, #20106, .T. ) ;
#26812 = CARTESIAN_POINT ( 'NONE',  ( 58.88972745734179171, -34.00000000000007105, -49.22241343995298024 ) ) ;
#26813 = AXIS2_PLACEMENT_3D ( 'NONE', #11476, #22921, #14650 ) ;
#26814 = DIRECTION ( 'NONE',  ( 0.000000000000000000, 0.000000000000000000, 1.000000000000000000 ) ) ;
#26815 = AXIS2_PLACEMENT_3D ( 'NONE', #1178, #9050, #21041 ) ;
#26816 = FACE_OUTER_BOUND ( 'NONE', #186, .T. ) ;
#26817 = EDGE_LOOP ( 'NONE', ( #9989, #24442, #24635, #23751 ) ) ;
#26818 = DIRECTION ( 'NONE',  ( 1.000000000000000000, 0.000000000000000000, 0.000000000000000000 ) ) ;
#26819 = LINE ( 'NONE', #12558, #30963 ) ;
#26820 = EDGE_LOOP ( 'NONE', ( #3179, #13585, #4885, #11614 ) ) ;
#26821 = ORIENTED_EDGE ( 'NONE', *, *, #14229, .T. ) ;
#26822 = AXIS2_PLACEMENT_3D ( 'NONE', #35159, #15643, #27064 ) ;
#26823 = LINE ( 'NONE', #9017, #30816 ) ;
#26824 = EDGE_CURVE ( 'NONE', #3385, #32894, #14647, .T. ) ;
#26825 = CARTESIAN_POINT ( 'NONE',  ( 67.30619744048945563, -84.18124734178287838, 32.50000000000000000 ) ) ;
#26826 = CARTESIAN_POINT ( 'NONE',  ( -72.00000337463102085, -34.64101615137762025, -9.999999999999998224 ) ) ;
#26827 = CARTESIAN_POINT ( 'NONE',  ( 69.99999662536839651, -17.32050807568879947, -9.999999999999998224 ) ) ;
#26828 = ORIENTED_EDGE ( 'NONE', *, *, #25213, .F. ) ;
#26829 = CIRCLE ( 'NONE', #19635, 2.000000000000001776 ) ;
#26830 = DIRECTION ( 'NONE',  ( 1.000000000000000000, 0.000000000000000000, 0.000000000000000000 ) ) ;
#26831 = DIRECTION ( 'NONE',  ( -0.4999999999999980571, 0.8660254037844399289, 0.000000000000000000 ) ) ;
#26832 = CIRCLE ( 'NONE', #10672, 2.000000000000000000 ) ;
#26833 = VERTEX_POINT ( 'NONE', #18737 ) ;
#26834 = AXIS2_PLACEMENT_3D ( 'NONE', #14267, #34704, #34321 ) ;
#26835 = CYLINDRICAL_SURFACE ( 'NONE', #26186, 150.0000000000000284 ) ;
#26836 = VERTEX_POINT ( 'NONE', #6731 ) ;
#26837 = CARTESIAN_POINT ( 'NONE',  ( -85.00000337463092137, 25.98076211353317433, 12.50000000000000000 ) ) ;
#26838 = CARTESIAN_POINT ( 'NONE',  ( -53.00000337463106348, 43.30127018922197379, -5.000000000000000000 ) ) ;
#26839 = EDGE_CURVE ( 'NONE', #35776, #1755, #3284, .T. ) ;
#26840 = AXIS2_PLACEMENT_3D ( 'NONE', #12965, #10728, #36049 ) ;
#26841 = DIRECTION ( 'NONE',  ( 0.000000000000000000, 0.000000000000000000, 1.000000000000000000 ) ) ;
#26842 = VERTEX_POINT ( 'NONE', #4303 ) ;
#26843 = EDGE_CURVE ( 'NONE', #16830, #11964, #19429, .T. ) ;
#26844 = ORIENTED_EDGE ( 'NONE', *, *, #34447, .T. ) ;
#26845 = EDGE_CURVE ( 'NONE', #13964, #16940, #15842, .T. ) ;
#26846 = CIRCLE ( 'NONE', #5318, 2.000000000000001776 ) ;
#26847 = ORIENTED_EDGE ( 'NONE', *, *, #26757, .T. ) ;
#26848 = CARTESIAN_POINT ( 'NONE',  ( -7.000003374631307729, 77.94228634059957983, -9.999999999999998224 ) ) ;
#26849 = CARTESIAN_POINT ( 'NONE',  ( -68.00000337463102085, -34.64101615137762025, 12.50000000000000000 ) ) ;
#26850 = EDGE_CURVE ( 'NONE', #7710, #8936, #2664, .T. ) ;
#26851 = DIRECTION ( 'NONE',  ( -1.000000000000000000, 0.000000000000000000, 0.000000000000000000 ) ) ;
#26852 = CARTESIAN_POINT ( 'NONE',  ( -5.000003374631307729, 77.94228634059957983, 12.50000000000000000 ) ) ;
#26853 = AXIS2_PLACEMENT_3D ( 'NONE', #14205, #17013, #14397 ) ;
#26854 = CARTESIAN_POINT ( 'NONE',  ( -48.00000337463112032, -51.96152422706641971, -9.999999999999998224 ) ) ;
#26855 = EDGE_CURVE ( 'NONE', #10938, #33601, #7460, .T. ) ;
#26856 = ORIENTED_EDGE ( 'NONE', *, *, #14187, .T. ) ;
#26857 = DIRECTION ( 'NONE',  ( 0.000000000000000000, -1.000000000000000000, 0.000000000000000000 ) ) ;
#26858 = CARTESIAN_POINT ( 'NONE',  ( -20.00000337463123756, -69.28203230275522628, -9.999999999999998224 ) ) ;
#26859 = AXIS2_PLACEMENT_3D ( 'NONE', #36947, #19874, #5070 ) ;
#26860 = CARTESIAN_POINT ( 'NONE',  ( -63.00000337463106348, -60.62177826491083010, -5.000000000000000000 ) ) ;
#26861 = VERTEX_POINT ( 'NONE', #8722 ) ;
#26862 = CARTESIAN_POINT ( 'NONE',  ( 42.99999662536848888, -77.94228634059960825, -9.999999999999998224 ) ) ;
#26863 = CIRCLE ( 'NONE', #10702, 2.000000000000001776 ) ;
#26864 = FACE_BOUND ( 'NONE', #35296, .T. ) ;
#26865 = DIRECTION ( 'NONE',  ( -1.000000000000000000, 0.000000000000000000, 0.000000000000000000 ) ) ;
#26866 = ADVANCED_FACE ( 'NONE', ( #11708 ), #19808, .F. ) ;
#26867 = AXIS2_PLACEMENT_3D ( 'NONE', #33111, #26942, #33309 ) ;
#26868 = ORIENTED_EDGE ( 'NONE', *, *, #32065, .T. ) ;
#26869 = EDGE_CURVE ( 'NONE', #22692, #8483, #5663, .T. ) ;
#26870 = EDGE_LOOP ( 'NONE', ( #16535, #8697, #26200, #1238, #29659, #5670, #23699, #19778, #25196, #22812, #28167, #18456, #15068, #34489, #3138, #28083, #2782, #14881, #13287, #16498, #5510, #9633, #16163, #12988, #20081, #24354, #16763, #9636, #25572 ) ) ;
#26871 = EDGE_CURVE ( 'NONE', #7462, #34182, #5931, .T. ) ;
#26872 = EDGE_CURVE ( 'NONE', #8683, #15938, #15240, .T. ) ;
#26873 = DIRECTION ( 'NONE',  ( 0.000000000000000000, 0.000000000000000000, 1.000000000000000000 ) ) ;
#26874 = LINE ( 'NONE', #3630, #25351 ) ;
#26875 = CARTESIAN_POINT ( 'NONE',  ( -0.3476802294499993229, -5.572769417831399785, -1.687189089856318880 ) ) ;
#26876 = ORIENTED_EDGE ( 'NONE', *, *, #33907, .F. ) ;
#26877 = ORIENTED_EDGE ( 'NONE', *, *, #897, .T. ) ;
#26878 = ORIENTED_EDGE ( 'NONE', *, *, #4058, .T. ) ;
#26879 = CARTESIAN_POINT ( 'NONE',  ( -3.374631327851540519E-06, 86.60254037844397601, 17.49999999999999645 ) ) ;
#26880 = ORIENTED_EDGE ( 'NONE', *, *, #6664, .F. ) ;
#26881 = ORIENTED_EDGE ( 'NONE', *, *, #36239, .T. ) ;
#26882 = CARTESIAN_POINT ( 'NONE',  ( 37.99999662536853151, -69.28203230275519786, -9.999999999999998224 ) ) ;
#26883 = EDGE_LOOP ( 'NONE', ( #29629, #18672, #21085, #23520 ) ) ;
#26884 = ORIENTED_EDGE ( 'NONE', *, *, #34804, .F. ) ;
#26885 = DIRECTION ( 'NONE',  ( 0.000000000000000000, 0.000000000000000000, 1.000000000000000000 ) ) ;
#26886 = DIRECTION ( 'NONE',  ( 0.000000000000000000, 0.000000000000000000, 1.000000000000000000 ) ) ;
#26887 = EDGE_LOOP ( 'NONE', ( #3004, #14940 ) ) ;
#26888 = VERTEX_POINT ( 'NONE', #8546 ) ;
#26889 = DIRECTION ( 'NONE',  ( 0.000000000000000000, 0.000000000000000000, 1.000000000000000000 ) ) ;
#26890 = AXIS2_PLACEMENT_3D ( 'NONE', #26507, #11885, #34600 ) ;
#26891 = CARTESIAN_POINT ( 'NONE',  ( 44.13139720814418610, 27.49999999999988987, 5.000000000000000888 ) ) ;
#26892 = CARTESIAN_POINT ( 'NONE',  ( -82.00000337463094979, 34.64101615137757051, 17.49999999999999645 ) ) ;
#26893 = CARTESIAN_POINT ( 'NONE',  ( -5.236872748402766398, -8.269757189038523917E-14, -4.057689166958448723 ) ) ;
#26894 = EDGE_LOOP ( 'NONE', ( #3636, #31642 ) ) ;
#26895 = CARTESIAN_POINT ( 'NONE',  ( -70.00000337463102085, -51.96152422706641971, -9.999999999999998224 ) ) ;
#26896 = CARTESIAN_POINT ( 'NONE',  ( -28.00000337463119493, -69.28203230275522628, -9.999999999999998224 ) ) ;
#26897 = AXIS2_PLACEMENT_3D ( 'NONE', #2524, #36480, #19785 ) ;
#26898 = VERTEX_POINT ( 'NONE', #34417 ) ;
#26899 = APPLICATION_CONTEXT ( 'automotive_design' ) ;
#26900 = DIRECTION ( 'NONE',  ( 1.000000000000000000, 0.000000000000000000, 0.000000000000000000 ) ) ;
#26901 = DIRECTION ( 'NONE',  ( 0.000000000000000000, 0.000000000000000000, 1.000000000000000000 ) ) ;
#26902 = DIRECTION ( 'NONE',  ( -0.8660254037844383745, 0.5000000000000005551, 0.000000000000000000 ) ) ;
#26903 = CIRCLE ( 'NONE', #16129, 8.500000000000003553 ) ;
#26904 = DIRECTION ( 'NONE',  ( -1.000000000000000000, 0.000000000000000000, 0.000000000000000000 ) ) ;
#26905 = DIRECTION ( 'NONE',  ( -1.000000000000000000, 0.000000000000000000, 0.000000000000000000 ) ) ;
#26906 = LINE ( 'NONE', #9827, #10366 ) ;
#26907 = ORIENTED_EDGE ( 'NONE', *, *, #4073, .F. ) ;
#26908 = DIRECTION ( 'NONE',  ( 0.000000000000000000, -0.000000000000000000, 1.000000000000000000 ) ) ;
#26909 = DIRECTION ( 'NONE',  ( 0.000000000000000000, 0.000000000000000000, 1.000000000000000000 ) ) ;
#26910 = CARTESIAN_POINT ( 'NONE',  ( -5.999999999999947597, 2.132877728683645235E-15, 27.50000000000000000 ) ) ;
#26911 = ORIENTED_EDGE ( 'NONE', *, *, #30205, .T. ) ;
#26912 = VERTEX_POINT ( 'NONE', #2935 ) ;
#26913 = AXIS2_PLACEMENT_3D ( 'NONE', #36397, #6954, #18768 ) ;
#26914 = ORIENTED_EDGE ( 'NONE', *, *, #3706, .F. ) ;
#26915 = AXIS2_PLACEMENT_3D ( 'NONE', #21302, #24305, #6511 ) ;
#26916 = ADVANCED_FACE ( 'NONE', ( #31398 ), #34248, .F. ) ;
#26917 = FACE_OUTER_BOUND ( 'NONE', #30753, .T. ) ;
#26918 = CARTESIAN_POINT ( 'NONE',  ( 0.000000000000000000, 0.000000000000000000, 27.50000000000000000 ) ) ;
#26919 = FACE_OUTER_BOUND ( 'NONE', #5234, .T. ) ;
#26920 = CARTESIAN_POINT ( 'NONE',  ( -30.00000337463118427, 69.28203230275516944, -9.999999999999998224 ) ) ;
#26921 = CARTESIAN_POINT ( 'NONE',  ( 41.99999662536853151, 69.28203230275518365, 12.50000000000000000 ) ) ;
#26922 = EDGE_LOOP ( 'NONE', ( #29404, #29219, #33420, #17650, #27437 ) ) ;
#26923 = CARTESIAN_POINT ( 'NONE',  ( -80.00000337463094979, 17.32050807568878525, 17.49999999999999645 ) ) ;
#26924 = ORIENTED_EDGE ( 'NONE', *, *, #34868, .T. ) ;
#26925 = FACE_OUTER_BOUND ( 'NONE', #31185, .T. ) ;
#26926 = AXIS2_PLACEMENT_3D ( 'NONE', #25057, #30483, #15679 ) ;
#26927 = DIRECTION ( 'NONE',  ( -0.000000000000000000, -0.000000000000000000, 1.000000000000000000 ) ) ;
#26928 = DIRECTION ( 'NONE',  ( 0.000000000000000000, 0.000000000000000000, 1.000000000000000000 ) ) ;
#26929 = FILL_AREA_STYLE ('',( #24119 ) ) ;
#26930 = ORIENTED_EDGE ( 'NONE', *, *, #1561, .T. ) ;
#26931 = CARTESIAN_POINT ( 'NONE',  ( 98.28784258492957804, -106.7731239591692116, 32.55002500000000509 ) ) ;
#26932 = AXIS2_PLACEMENT_3D ( 'NONE', #1381, #12803, #24257 ) ;
#26933 = ADVANCED_FACE ( 'NONE', ( #31232 ), #10975, .F. ) ;
#26934 = EDGE_CURVE ( 'NONE', #22366, #14606, #12854, .T. ) ;
#26935 = CARTESIAN_POINT ( 'NONE',  ( -33.00000337463116296, 60.62177826491077326, 17.49999999999999645 ) ) ;
#26936 = CIRCLE ( 'NONE', #7786, 2.000000000000001776 ) ;
#26937 = CARTESIAN_POINT ( 'NONE',  ( -18.00000337463123756, -86.60254037844400443, -9.999999999999998224 ) ) ;
#26938 = DIRECTION ( 'NONE',  ( 0.000000000000000000, 0.000000000000000000, 1.000000000000000000 ) ) ;
#26939 = ORIENTED_EDGE ( 'NONE', *, *, #15153, .F. ) ;
#26940 = DIRECTION ( 'NONE',  ( 0.000000000000000000, 0.000000000000000000, 1.000000000000000000 ) ) ;
#26941 = CIRCLE ( 'NONE', #12557, 3.000000000000002665 ) ;
#26942 = DIRECTION ( 'NONE',  ( -0.000000000000000000, -0.000000000000000000, 1.000000000000000000 ) ) ;
#26943 = CYLINDRICAL_SURFACE ( 'NONE', #9981, 2.000000000000001776 ) ;
#26944 = ORIENTED_EDGE ( 'NONE', *, *, #13769, .F. ) ;
#26945 = EDGE_CURVE ( 'NONE', #28371, #26995, #24872, .T. ) ;
#26946 = ORIENTED_EDGE ( 'NONE', *, *, #28654, .T. ) ;
#26947 = EDGE_LOOP ( 'NONE', ( #6787, #33344 ) ) ;
#26948 = DIRECTION ( 'NONE',  ( -0.000000000000000000, -0.000000000000000000, 1.000000000000000000 ) ) ;
#26949 = DIRECTION ( 'NONE',  ( 1.000000000000000000, 0.000000000000000000, 0.000000000000000000 ) ) ;
#26950 = VECTOR ( 'NONE', #1597, 1000.000000000000000 ) ;
#26951 = CARTESIAN_POINT ( 'NONE',  ( 59.99999662536842493, 51.96152422706639129, -9.999999999999998224 ) ) ;
#26952 = AXIS2_PLACEMENT_3D ( 'NONE', #20305, #224, #28744 ) ;
#26953 = EDGE_CURVE ( 'NONE', #12647, #23824, #30225, .T. ) ;
#26954 = DIRECTION ( 'NONE',  ( 1.000000000000000000, 0.000000000000000000, 0.000000000000000000 ) ) ;
#26955 = DIRECTION ( 'NONE',  ( -3.554796214472773777E-16, -1.000000000000000000, 0.000000000000000000 ) ) ;
#26956 = CIRCLE ( 'NONE', #14995, 2.000000000000000000 ) ;
#26957 = CARTESIAN_POINT ( 'NONE',  ( 91.99999662536828282, 0.000000000000000000, -5.000000000000000000 ) ) ;
#26958 = ORIENTED_EDGE ( 'NONE', *, *, #16234, .F. ) ;
#26959 = ORIENTED_EDGE ( 'NONE', *, *, #35404, .F. ) ;
#26960 = PRESENTATION_STYLE_ASSIGNMENT (( #27518 ) ) ;
#26961 = AXIS2_PLACEMENT_3D ( 'NONE', #29003, #26572, #328 ) ;
#26962 = DIRECTION ( 'NONE',  ( 0.000000000000000000, 0.000000000000000000, -1.000000000000000000 ) ) ;
#26963 = ORIENTED_EDGE ( 'NONE', *, *, #6688, .T. ) ;
#26964 = CARTESIAN_POINT ( 'NONE',  ( -50.00000337463109190, 69.28203230275518365, -9.999999999999998224 ) ) ;
#26965 = ORIENTED_EDGE ( 'NONE', *, *, #6588, .F. ) ;
#26966 = DIRECTION ( 'NONE',  ( 1.000000000000000000, 0.000000000000000000, 0.000000000000000000 ) ) ;
#26967 = CARTESIAN_POINT ( 'NONE',  ( 71.99999662536839651, -3.469446951953614189E-15, 12.50000000000000000 ) ) ;
#26968 = ORIENTED_EDGE ( 'NONE', *, *, #10333, .F. ) ;
#26969 = ORIENTED_EDGE ( 'NONE', *, *, #27274, .F. ) ;
#26970 = EDGE_CURVE ( 'NONE', #14832, #25364, #20056, .T. ) ;
#26971 = VECTOR ( 'NONE', #25575, 1000.000000000000000 ) ;
#26972 = DIRECTION ( 'NONE',  ( 0.000000000000000000, 0.000000000000000000, 1.000000000000000000 ) ) ;
#26973 = VERTEX_POINT ( 'NONE', #25250 ) ;
#26974 = CARTESIAN_POINT ( 'NONE',  ( -40.98360655737705116, 111.1639425680974398, 18.49999999999999645 ) ) ;
#26975 = FACE_OUTER_BOUND ( 'NONE', #23421, .T. ) ;
#26976 = CARTESIAN_POINT ( 'NONE',  ( -3.000003374631269981, -77.94228634059960825, -5.000000000000000000 ) ) ;
#26977 = CIRCLE ( 'NONE', #17403, 95.00000000000001421 ) ;
#26978 = ORIENTED_EDGE ( 'NONE', *, *, #34311, .F. ) ;
#26979 = EDGE_CURVE ( 'NONE', #21341, #11639, #25809, .T. ) ;
#26980 = ORIENTED_EDGE ( 'NONE', *, *, #36892, .F. ) ;
#26981 = ORIENTED_EDGE ( 'NONE', *, *, #18812, .F. ) ;
#26982 = EDGE_CURVE ( 'NONE', #1442, #30601, #32633, .T. ) ;
#26983 = ORIENTED_EDGE ( 'NONE', *, *, #9391, .F. ) ;
#26984 = CARTESIAN_POINT ( 'NONE',  ( -98.28784258492883907, 106.7731239591698937, 32.55002500000000509 ) ) ;
#26985 = DIRECTION ( 'NONE',  ( 1.000000000000000000, 0.000000000000000000, 0.000000000000000000 ) ) ;
#26986 = ORIENTED_EDGE ( 'NONE', *, *, #11000, .F. ) ;
#26987 = FACE_OUTER_BOUND ( 'NONE', #32781, .T. ) ;
#26988 = CARTESIAN_POINT ( 'NONE',  ( -5.000000000000000000, -0.9645339558193164464, -0.6919071587033235327 ) ) ;
#26989 = DIRECTION ( 'NONE',  ( -0.4999999999999980571, 0.8660254037844399289, 0.000000000000000000 ) ) ;
#26990 = ORIENTED_EDGE ( 'NONE', *, *, #16806, .F. ) ;
#26991 = DIRECTION ( 'NONE',  ( -0.000000000000000000, -0.000000000000000000, 1.000000000000000000 ) ) ;
#26992 =( BOUNDED_CURVE ( )  B_SPLINE_CURVE ( 3, ( #22114, #10673, #24567, #19300 ),
 .UNSPECIFIED., .F., .F. ) 
 B_SPLINE_CURVE_WITH_KNOTS ( ( 4, 4 ),
 ( 3.141592653589793116, 4.712388980384689674 ),
 .UNSPECIFIED. ) 
 CURVE ( )  GEOMETRIC_REPRESENTATION_ITEM ( )  RATIONAL_B_SPLINE_CURVE ( ( 1.000000000000000000, 0.8047378541243649375, 0.8047378541243649375, 1.000000000000000000 ) ) 
 REPRESENTATION_ITEM ( '' )  );
#26993 = DIRECTION ( 'NONE',  ( -0.000000000000000000, -0.000000000000000000, -1.000000000000000000 ) ) ;
#26994 = DIRECTION ( 'NONE',  ( 1.000000000000000000, 0.000000000000000000, 0.000000000000000000 ) ) ;
#26995 = VERTEX_POINT ( 'NONE', #30844 ) ;
#26996 = CARTESIAN_POINT ( 'NONE',  ( 81.99999662536833966, 34.64101615137759183, 12.50000000000000000 ) ) ;
#26997 = DIRECTION ( 'NONE',  ( 1.000000000000000000, 0.000000000000000000, 0.000000000000000000 ) ) ;
#26998 = ORIENTED_EDGE ( 'NONE', *, *, #7290, .T. ) ;
#26999 = ORIENTED_EDGE ( 'NONE', *, *, #26453, .T. ) ;
#27000 = ADVANCED_FACE ( 'NONE', ( #8375 ), #2101, .T. ) ;
#27001 = DIRECTION ( 'NONE',  ( -0.000000000000000000, -0.000000000000000000, 1.000000000000000000 ) ) ;
#27002 = CARTESIAN_POINT ( 'NONE',  ( -85.00000337463092137, 25.98076211353317433, 17.49999999999999645 ) ) ;
#27003 = CIRCLE ( 'NONE', #3646, 27.00000000000001066 ) ;
#27004 = FACE_OUTER_BOUND ( 'NONE', #21358, .T. ) ;
#27005 = DIRECTION ( 'NONE',  ( 0.000000000000000000, 0.000000000000000000, 1.000000000000000000 ) ) ;
#27006 = EDGE_LOOP ( 'NONE', ( #9757, #6170 ) ) ;
#27007 = ADVANCED_FACE ( 'NONE', ( #33863 ), #31050, .T. ) ;
#27008 = DIRECTION ( 'NONE',  ( 1.000000000000000000, 0.000000000000000000, 0.000000000000000000 ) ) ;
#27009 = DIRECTION ( 'NONE',  ( 0.000000000000000000, 0.000000000000000000, 1.000000000000000000 ) ) ;
#27010 = ORIENTED_EDGE ( 'NONE', *, *, #26187, .F. ) ;
#27011 = EDGE_CURVE ( 'NONE', #22792, #14280, #28403, .T. ) ;
#27012 = DIRECTION ( 'NONE',  ( 0.000000000000000000, 0.000000000000000000, -1.000000000000000000 ) ) ;
#27013 = ORIENTED_EDGE ( 'NONE', *, *, #24796, .F. ) ;
#27014 = DIRECTION ( 'NONE',  ( 1.000000000000000000, 0.000000000000000000, 0.000000000000000000 ) ) ;
#27015 = CARTESIAN_POINT ( 'NONE',  ( -56.67878100130369035, 27.78182860042797131, 12.49999999999999822 ) ) ;
#27016 = DIRECTION ( 'NONE',  ( -1.000000000000000000, 0.000000000000000000, 0.000000000000000000 ) ) ;
#27017 = VERTEX_POINT ( 'NONE', #37057 ) ;
#27018 = VERTEX_POINT ( 'NONE', #11359 ) ;
#27019 = VECTOR ( 'NONE', #34130, 1000.000000000000000 ) ;
#27020 = ADVANCED_FACE ( 'NONE', ( #35372 ), #31935, .F. ) ;
#27021 = ORIENTED_EDGE ( 'NONE', *, *, #18408, .T. ) ;
#27022 = LINE ( 'NONE', #24413, #30951 ) ;
#27023 = FACE_OUTER_BOUND ( 'NONE', #10434, .T. ) ;
#27024 = DIRECTION ( 'NONE',  ( 1.000000000000000000, 0.000000000000000000, 0.000000000000000000 ) ) ;
#27025 = DIRECTION ( 'NONE',  ( 0.000000000000000000, 0.000000000000000000, 1.000000000000000000 ) ) ;
#27026 = CARTESIAN_POINT ( 'NONE',  ( 72.99999662536836809, 43.30127018922198801, -9.999999999999998224 ) ) ;
#27027 = ORIENTED_EDGE ( 'NONE', *, *, #24056, .T. ) ;
#27028 = CARTESIAN_POINT ( 'NONE',  ( -45.00000337463111322, -77.94228634059960825, -9.999999999999998224 ) ) ;
#27029 = B_SPLINE_CURVE_WITH_KNOTS ( 'NONE', 3,
 ( #10355, #13731, #25187, #27776, #36612, #28165, #10906, #13342 ),
 .UNSPECIFIED., .F., .F.,
 ( 4, 2, 2, 4 ),
 ( 2.451332857604987150E-07, 0.001475502392055724754, 0.002213131021440706107, 0.002950759650825688762 ),
 .UNSPECIFIED. ) ;
#27030 = CARTESIAN_POINT ( 'NONE',  ( -3.000000000000000888, 0.000000000000000000, -5.674599999999998090 ) ) ;
#27031 = ORIENTED_EDGE ( 'NONE', *, *, #30960, .F. ) ;
#27032 = DIRECTION ( 'NONE',  ( 0.000000000000000000, 0.000000000000000000, 1.000000000000000000 ) ) ;
#27033 = DIRECTION ( 'NONE',  ( 1.000000000000000000, 0.000000000000000000, -0.000000000000000000 ) ) ;
#27034 = ORIENTED_EDGE ( 'NONE', *, *, #26753, .F. ) ;
#27035 = ORIENTED_EDGE ( 'NONE', *, *, #20218, .F. ) ;
#27036 = EDGE_CURVE ( 'NONE', #245, #20452, #26052, .T. ) ;
#27037 = AXIS2_PLACEMENT_3D ( 'NONE', #4574, #30060, #27062 ) ;
#27038 = DIRECTION ( 'NONE',  ( 0.000000000000000000, 0.000000000000000000, 1.000000000000000000 ) ) ;
#27039 = CARTESIAN_POINT ( 'NONE',  ( -94.55012560584690107, -9.234378588653417097, 27.50000000000000000 ) ) ;
#27040 = EDGE_CURVE ( 'NONE', #19680, #13964, #29508, .T. ) ;
#27041 = CYLINDRICAL_SURFACE ( 'NONE', #13015, 2.000000000000001776 ) ;
#27042 = ORIENTED_EDGE ( 'NONE', *, *, #30807, .T. ) ;
#27043 = AXIS2_PLACEMENT_3D ( 'NONE', #17454, #31323, #14078 ) ;
#27044 = ORIENTED_EDGE ( 'NONE', *, *, #35489, .T. ) ;
#27045 = ORIENTED_EDGE ( 'NONE', *, *, #14136, .T. ) ;
#27046 = EDGE_CURVE ( 'NONE', #21830, #19005, #3891, .T. ) ;
#27047 = CARTESIAN_POINT ( 'NONE',  ( -35.00000337463117717, -77.94228634059963667, -5.000000000000000000 ) ) ;
#27048 = ORIENTED_EDGE ( 'NONE', *, *, #22448, .T. ) ;
#27050 = EDGE_CURVE ( 'NONE', #33855, #4682, #20509, .T. ) ;
#27049 = VERTEX_POINT ( 'NONE', #23718 ) ;
#27051 = CARTESIAN_POINT ( 'NONE',  ( 34.99999662536853862, 77.94228634059959404, -5.000000000000000000 ) ) ;
#27052 = VERTEX_POINT ( 'NONE', #32509 ) ;
#27053 = EDGE_CURVE ( 'NONE', #22919, #4653, #22443, .T. ) ;
#27054 = ORIENTED_EDGE ( 'NONE', *, *, #26979, .T. ) ;
#27055 = CARTESIAN_POINT ( 'NONE',  ( -80.00000337463096400, -34.64101615137762025, -5.000000000000000000 ) ) ;
#27056 = CARTESIAN_POINT ( 'NONE',  ( 89.99999662536828282, 0.000000000000000000, -9.999999999999998224 ) ) ;
#27057 = VERTEX_POINT ( 'NONE', #4025 ) ;
#27058 = ORIENTED_EDGE ( 'NONE', *, *, #26117, .F. ) ;
#27059 = FACE_OUTER_BOUND ( 'NONE', #2435, .T. ) ;
#27060 = LINE ( 'NONE', #21247, #6355 ) ;
#27061 = EDGE_CURVE ( 'NONE', #32911, #35959, #12249, .T. ) ;
#27062 = DIRECTION ( 'NONE',  ( 0.000000000000000000, 0.000000000000000000, -1.000000000000000000 ) ) ;
#27063 = EDGE_CURVE ( 'NONE', #27148, #16244, #29630, .T. ) ;
#27064 = DIRECTION ( 'NONE',  ( 1.000000000000000000, 0.000000000000000000, 0.000000000000000000 ) ) ;
#27065 = EDGE_CURVE ( 'NONE', #10178, #7273, #8080, .T. ) ;
#27066 = VERTEX_POINT ( 'NONE', #12638 ) ;
#27067 = DIRECTION ( 'NONE',  ( 0.000000000000000000, 0.000000000000000000, 1.000000000000000000 ) ) ;
#27068 = AXIS2_PLACEMENT_3D ( 'NONE', #5503, #31724, #14658 ) ;
#27069 = EDGE_CURVE ( 'NONE', #30871, #18239, #28207, .T. ) ;
#27070 = VERTEX_POINT ( 'NONE', #3277 ) ;
#27071 = CARTESIAN_POINT ( 'NONE',  ( -4.279621169095561228, 62.97617850287782915, -4.999999999999997335 ) ) ;
#27072 = EDGE_CURVE ( 'NONE', #18793, #18742, #8688, .T. ) ;
#27073 = CYLINDRICAL_SURFACE ( 'NONE', #10622, 2.000000000000001776 ) ;
#27074 = FACE_OUTER_BOUND ( 'NONE', #26716, .T. ) ;
#27075 = DIRECTION ( 'NONE',  ( 0.000000000000000000, 0.000000000000000000, -1.000000000000000000 ) ) ;
#27076 = CARTESIAN_POINT ( 'NONE',  ( -34.00000000000000000, -103.4105893997321743, 27.50000000000000000 ) ) ;
#27077 = CARTESIAN_POINT ( 'NONE',  ( -47.00000337463111322, 77.94228634059959404, -5.000000000000000000 ) ) ;
#27078 = CARTESIAN_POINT ( 'NONE',  ( 5.000000000000000000, 1.831554690317580780, -1.158389257021584795 ) ) ;
#27079 = ORIENTED_EDGE ( 'NONE', *, *, #29524, .T. ) ;
#27080 = DIRECTION ( 'NONE',  ( 0.000000000000000000, 0.000000000000000000, -1.000000000000000000 ) ) ;
#27081 = DIRECTION ( 'NONE',  ( -0.000000000000000000, -0.000000000000000000, -1.000000000000000000 ) ) ;
#27082 = DIRECTION ( 'NONE',  ( 1.000000000000000000, 0.000000000000000000, 0.000000000000000000 ) ) ;
#27083 = ORIENTED_EDGE ( 'NONE', *, *, #20715, .F. ) ;
#27084 = CIRCLE ( 'NONE', #34882, 25.00000000000000000 ) ;
#27085 = EDGE_LOOP ( 'NONE', ( #32348, #3897 ) ) ;
#27086 = ORIENTED_EDGE ( 'NONE', *, *, #35281, .T. ) ;
#27087 = CYLINDRICAL_SURFACE ( 'NONE', #29720, 6.000000000000005329 ) ;
#27088 = CARTESIAN_POINT ( 'NONE',  ( 86.45172111230354517, -31.46585318596159553, -4.999999999999997335 ) ) ;
#27089 = DIRECTION ( 'NONE',  ( -0.000000000000000000, 1.000000000000000000, 0.000000000000000000 ) ) ;
#27090 = ORIENTED_EDGE ( 'NONE', *, *, #29576, .F. ) ;
#27091 = CARTESIAN_POINT ( 'NONE',  ( 51.99999662536847467, -69.28203230275519786, -9.999999999999998224 ) ) ;
#27092 = VECTOR ( 'NONE', #15778, 1000.000000000000000 ) ;
#27093 = CYLINDRICAL_SURFACE ( 'NONE', #21920, 2.000000000000001776 ) ;
#27094 = EDGE_LOOP ( 'NONE', ( #15059, #16070, #33766, #23268 ) ) ;
#27095 = FACE_BOUND ( 'NONE', #4687, .T. ) ;
#27096 = ORIENTED_EDGE ( 'NONE', *, *, #23077, .F. ) ;
#27097 = CARTESIAN_POINT ( 'NONE',  ( 62.99999662536841072, -25.98076211353320275, -5.000000000000000000 ) ) ;
#27098 = FACE_OUTER_BOUND ( 'NONE', #23928, .T. ) ;
#27099 = DIRECTION ( 'NONE',  ( 0.000000000000000000, 0.000000000000000000, 1.000000000000000000 ) ) ;
#27100 = FACE_OUTER_BOUND ( 'NONE', #31568, .T. ) ;
#27101 = EDGE_LOOP ( 'NONE', ( #35324, #29308, #13338, #17281 ) ) ;
#27102 = CYLINDRICAL_SURFACE ( 'NONE', #27870, 2.000000000000001776 ) ;
#27103 = ITEM_DEFINED_TRANSFORMATION ( 'NONE', 'NONE', #27345,  #21385 ) ;
#27104 = DIRECTION ( 'NONE',  ( 0.000000000000000000, 0.000000000000000000, 1.000000000000000000 ) ) ;
#27105 = ADVANCED_FACE ( 'NONE', ( #32135, #34968 ), #34796, .T. ) ;
#27106 = AXIS2_PLACEMENT_3D ( 'NONE', #18940, #27174, #24187 ) ;
#27107 = DIRECTION ( 'NONE',  ( 0.000000000000000000, 0.000000000000000000, 1.000000000000000000 ) ) ;
#27108 = CARTESIAN_POINT ( 'NONE',  ( -78.38502691089041718, -33.46124879229190441, 12.50000000000000000 ) ) ;
#27109 = EDGE_CURVE ( 'NONE', #24647, #8725, #298, .T. ) ;
#27110 = ORIENTED_EDGE ( 'NONE', *, *, #26593, .F. ) ;
#27111 = CARTESIAN_POINT ( 'NONE',  ( 9.999996625368625658, 86.60254037844397601, -9.999999999999998224 ) ) ;
#27112 = FACE_OUTER_BOUND ( 'NONE', #29249, .T. ) ;
#27113 = CARTESIAN_POINT ( 'NONE',  ( -75.00000337463099243, -25.98076211353322051, 17.49999999999999645 ) ) ;
#27114 = VERTEX_POINT ( 'NONE', #657 ) ;
#27115 = AXIS2_PLACEMENT_3D ( 'NONE', #26522, #4229, #9483 ) ;
#27116 = ORIENTED_EDGE ( 'NONE', *, *, #35459, .T. ) ;
#27117 = AXIS2_PLACEMENT_3D ( 'NONE', #10583, #30637, #18842 ) ;
#27118 = LINE ( 'NONE', #27305, #27350 ) ;
#27119 = LINE ( 'NONE', #4269, #34496 ) ;
#27120 = DIRECTION ( 'NONE',  ( 0.000000000000000000, 0.000000000000000000, -1.000000000000000000 ) ) ;
#27121 = ORIENTED_EDGE ( 'NONE', *, *, #729, .T. ) ;
#27122 = DIRECTION ( 'NONE',  ( 1.000000000000000000, 0.000000000000000000, 0.000000000000000000 ) ) ;
#27123 = CARTESIAN_POINT ( 'NONE',  ( -5.999999999999998224, -145.0000000000000568, 32.55002500000000509 ) ) ;
#27124 = CARTESIAN_POINT ( 'NONE',  ( 7.999996625368618552, 69.28203230275516944, -5.000000000000000000 ) ) ;
#27125 = AXIS2_PLACEMENT_3D ( 'NONE', #5151, #16786, #2348 ) ;
#27126 = CARTESIAN_POINT ( 'NONE',  ( -107.2242716242193836, 49.31285668773285380, 32.49999999999999289 ) ) ;
#27127 = EDGE_CURVE ( 'NONE', #36648, #31059, #12067, .T. ) ;
#27128 = ORIENTED_EDGE ( 'NONE', *, *, #35788, .F. ) ;
#27129 = EDGE_LOOP ( 'NONE', ( #28724, #30728 ) ) ;
#27130 = AXIS2_PLACEMENT_3D ( 'NONE', #12515, #35976, #3718 ) ;
#27131 = CARTESIAN_POINT ( 'NONE',  ( 4.242640687119310527, 4.242640687119267007, 27.50000000000000000 ) ) ;
#27132 = CARTESIAN_POINT ( 'NONE',  ( 0.000000000000000000, 89.94802294027088863, 32.49999999999999289 ) ) ;
#27133 = ORIENTED_EDGE ( 'NONE', *, *, #33811, .F. ) ;
#27134 = DIRECTION ( 'NONE',  ( 1.000000000000000000, 0.000000000000000000, 0.000000000000000000 ) ) ;
#27135 = ORIENTED_EDGE ( 'NONE', *, *, #3837, .T. ) ;
#27136 = CARTESIAN_POINT ( 'NONE',  ( 0.000000000000000000, 0.000000000000000000, 12.49999999999999822 ) ) ;
#27137 = EDGE_CURVE ( 'NONE', #35523, #30112, #23650, .T. ) ;
#27138 = FACE_BOUND ( 'NONE', #13575, .T. ) ;
#27139 = EDGE_LOOP ( 'NONE', ( #23269, #23532 ) ) ;
#27140 = ORIENTED_EDGE ( 'NONE', *, *, #19948, .F. ) ;
#27141 = CARTESIAN_POINT ( 'NONE',  ( -3.374631289687624047E-06, -69.28203230275519786, 12.50000000000000000 ) ) ;
#27142 = VERTEX_POINT ( 'NONE', #3661 ) ;
#27143 =( NAMED_UNIT ( * ) PLANE_ANGLE_UNIT ( ) SI_UNIT ( $, .RADIAN. ) );
#27144 = DIRECTION ( 'NONE',  ( 1.000000000000000000, 0.000000000000000000, 0.000000000000000000 ) ) ;
#27145 = FACE_OUTER_BOUND ( 'NONE', #11209, .T. ) ;
#27146 = LINE ( 'NONE', #24353, #19717 ) ;
#27147 = EDGE_CURVE ( 'NONE', #20281, #35451, #33231, .T. ) ;
#27148 = VERTEX_POINT ( 'NONE', #830 ) ;
#27149 = DIRECTION ( 'NONE',  ( 0.000000000000000000, 0.000000000000000000, -1.000000000000000000 ) ) ;
#27150 = CIRCLE ( 'NONE', #12168, 2.000000000000000000 ) ;
#27151 = CARTESIAN_POINT ( 'NONE',  ( 67.99999662536838230, 17.32050807568879236, -9.999999999999998224 ) ) ;
#27152 = VERTEX_POINT ( 'NONE', #1025 ) ;
#27153 = ORIENTED_EDGE ( 'NONE', *, *, #10819, .T. ) ;
#27154 = ORIENTED_EDGE ( 'NONE', *, *, #14862, .T. ) ;
#27155 = DIRECTION ( 'NONE',  ( 1.000000000000000000, 0.000000000000000000, 0.000000000000000000 ) ) ;
#27156 = DIRECTION ( 'NONE',  ( 0.000000000000000000, 0.000000000000000000, 1.000000000000000000 ) ) ;
#27157 = VERTEX_POINT ( 'NONE', #30629 ) ;
#27158 = DIRECTION ( 'NONE',  ( -1.000000000000000000, 0.000000000000000000, 0.000000000000000000 ) ) ;
#27159 = DIRECTION ( 'NONE',  ( 1.000000000000000000, 0.000000000000000000, 0.000000000000000000 ) ) ;
#27160 = ORIENTED_EDGE ( 'NONE', *, *, #15790, .T. ) ;
#27161 = DIRECTION ( 'NONE',  ( 0.000000000000000000, 0.000000000000000000, 1.000000000000000000 ) ) ;
#27162 = AXIS2_PLACEMENT_3D ( 'NONE', #6762, #12010, #29271 ) ;
#27163 = DIRECTION ( 'NONE',  ( 1.000000000000000000, 0.000000000000000000, 0.000000000000000000 ) ) ;
#27164 = CIRCLE ( 'NONE', #32544, 3.000000000000000000 ) ;
#27165 = ADVANCED_FACE ( 'NONE', ( #21462 ), #21816, .F. ) ;
#27166 = DIRECTION ( 'NONE',  ( -0.8660254037844379305, 0.5000000000000011102, 0.000000000000000000 ) ) ;
#27167 = CYLINDRICAL_SURFACE ( 'NONE', #22670, 2.000000000000001776 ) ;
#27168 = FACE_OUTER_BOUND ( 'NONE', #15138, .T. ) ;
#27169 = EDGE_CURVE ( 'NONE', #36755, #31731, #21266, .T. ) ;
#27170 = CARTESIAN_POINT ( 'NONE',  ( 0.000000000000000000, 0.000000000000000000, -5.000000000000000000 ) ) ;
#27171 = ORIENTED_EDGE ( 'NONE', *, *, #14432, .T. ) ;
#27172 = VERTEX_POINT ( 'NONE', #16383 ) ;
#27173 = DIRECTION ( 'NONE',  ( -1.000000000000000000, -0.000000000000000000, -0.000000000000000000 ) ) ;
#27174 = DIRECTION ( 'NONE',  ( 0.000000000000000000, 0.000000000000000000, 1.000000000000000000 ) ) ;
#27175 = CARTESIAN_POINT ( 'NONE',  ( -50.00000337463109190, 51.96152422706637708, 12.50000000000000000 ) ) ;
#27176 = DIRECTION ( 'NONE',  ( 0.000000000000000000, 0.000000000000000000, 1.000000000000000000 ) ) ;
#27177 = ADVANCED_FACE ( 'NONE', ( #10021 ), #19026, .F. ) ;
#27178 = ORIENTED_EDGE ( 'NONE', *, *, #19769, .F. ) ;
#27179 = CARTESIAN_POINT ( 'NONE',  ( -93.55673653615987462, -16.49657687835775377, 12.49999999999999822 ) ) ;
#27180 = CARTESIAN_POINT ( 'NONE',  ( 0.000000000000000000, 0.000000000000000000, 0.000000000000000000 ) ) ;
#27181 = EDGE_CURVE ( 'NONE', #6052, #17563, #28431, .T. ) ;
#27182 = ORIENTED_EDGE ( 'NONE', *, *, #30847, .F. ) ;
#27183 = DIRECTION ( 'NONE',  ( 0.000000000000000000, 0.000000000000000000, 1.000000000000000000 ) ) ;
#27184 = ORIENTED_EDGE ( 'NONE', *, *, #6583, .T. ) ;
#27185 = DIRECTION ( 'NONE',  ( 1.000000000000000000, 0.000000000000000000, 0.000000000000000000 ) ) ;
#27186 = AXIS2_PLACEMENT_3D ( 'NONE', #23468, #6208, #11831 ) ;
#27187 = CARTESIAN_POINT ( 'NONE',  ( -20.00000337463123756, -86.60254037844400443, 12.50000000000000000 ) ) ;
#27188 = CIRCLE ( 'NONE', #5039, 2.000000000000001776 ) ;
#27189 = CARTESIAN_POINT ( 'NONE',  ( 62.97617850287784336, 4.279621169095339184, 12.49999999999999822 ) ) ;
#27190 = EDGE_CURVE ( 'NONE', #21193, #19879, #4226, .T. ) ;
#27191 = ORIENTED_EDGE ( 'NONE', *, *, #21355, .F. ) ;
#27192 = ORIENTED_EDGE ( 'NONE', *, *, #4561, .F. ) ;
#27193 = EDGE_CURVE ( 'NONE', #719, #29785, #16027, .T. ) ;
#27194 = VERTEX_POINT ( 'NONE', #7774 ) ;
#27195 = FACE_OUTER_BOUND ( 'NONE', #15423, .T. ) ;
#27196 = FACE_BOUND ( 'NONE', #5376, .T. ) ;
#27197 = CIRCLE ( 'NONE', #11640, 30.00000000000000000 ) ;
#27198 = CARTESIAN_POINT ( 'NONE',  ( -2.374207310413330682E-13, -68.00000000000000000, -49.86348611802629449 ) ) ;
#27199 = CARTESIAN_POINT ( 'NONE',  ( -52.00000337463109190, 51.96152422706637708, 12.50000000000000000 ) ) ;
#27200 = CARTESIAN_POINT ( 'NONE',  ( 26.99999662536859546, -77.94228634059960825, -9.999999999999998224 ) ) ;
#27201 = ORIENTED_EDGE ( 'NONE', *, *, #24493, .F. ) ;
#27202 = DIRECTION ( 'NONE',  ( 1.000000000000000000, 0.000000000000000000, 0.000000000000000000 ) ) ;
#27203 = EDGE_CURVE ( 'NONE', #34980, #14875, #5697, .T. ) ;
#27204 = AXIS2_PLACEMENT_3D ( 'NONE', #28709, #5643, #17081 ) ;
#27205 = LINE ( 'NONE', #13163, #32931 ) ;
#27206 = EDGE_CURVE ( 'NONE', #35276, #34186, #30841, .T. ) ;
#27207 = LINE ( 'NONE', #33777, #25391 ) ;
#27208 = ORIENTED_EDGE ( 'NONE', *, *, #15512, .F. ) ;
#27209 = DIRECTION ( 'NONE',  ( 0.000000000000000000, 0.000000000000000000, 1.000000000000000000 ) ) ;
#27210 = CARTESIAN_POINT ( 'NONE',  ( 2.500000000000000444, 0.000000000000000000, -5.700000000000000178 ) ) ;
#27211 = AXIS2_PLACEMENT_3D ( 'NONE', #32974, #7465, #16457 ) ;
#27212 = ORIENTED_EDGE ( 'NONE', *, *, #20527, .T. ) ;
#27213 = EDGE_CURVE ( 'NONE', #15428, #25705, #31432, .T. ) ;
#27214 = VECTOR ( 'NONE', #35430, 1000.000000000000000 ) ;
#27215 = EDGE_LOOP ( 'NONE', ( #27925, #21932 ) ) ;
#27216 = AXIS2_PLACEMENT_3D ( 'NONE', #14155, #3268, #28392 ) ;
#27217 = CYLINDRICAL_SURFACE ( 'NONE', #24716, 2.000000000000001776 ) ;
#27218 = LINE ( 'NONE', #30419, #28356 ) ;
#27219 = DIRECTION ( 'NONE',  ( 0.000000000000000000, 0.000000000000000000, 1.000000000000000000 ) ) ;
#27220 = ADVANCED_FACE ( 'NONE', ( #29896 ), #18654, .F. ) ;
#27221 = VERTEX_POINT ( 'NONE', #15824 ) ;
#27222 = VERTEX_POINT ( 'NONE', #27076 ) ;
#27223 = ORIENTED_EDGE ( 'NONE', *, *, #9869, .T. ) ;
#27224 = DIRECTION ( 'NONE',  ( 1.000000000000000000, 0.000000000000000000, 0.000000000000000000 ) ) ;
#27225 = EDGE_CURVE ( 'NONE', #2344, #10755, #4495, .T. ) ;
#27226 = CIRCLE ( 'NONE', #11061, 2.500000000000000444 ) ;
#27227 = ORIENTED_EDGE ( 'NONE', *, *, #29247, .T. ) ;
#27228 = VERTEX_POINT ( 'NONE', #18834 ) ;
#27229 = DIRECTION ( 'NONE',  ( 1.000000000000000000, 0.000000000000000000, 0.000000000000000000 ) ) ;
#27230 = ORIENTED_EDGE ( 'NONE', *, *, #16666, .T. ) ;
#27231 = ORIENTED_EDGE ( 'NONE', *, *, #2301, .T. ) ;
#27232 = DIRECTION ( 'NONE',  ( 1.000000000000000000, 0.000000000000000000, 0.000000000000000000 ) ) ;
#27233 = CARTESIAN_POINT ( 'NONE',  ( -77.00000337463097821, 43.30127018922197379, 17.49999999999999645 ) ) ;
#27234 = ORIENTED_EDGE ( 'NONE', *, *, #20870, .T. ) ;
#27235 = EDGE_LOOP ( 'NONE', ( #14999, #28323, #19517, #32656 ) ) ;
#27236 = FACE_OUTER_BOUND ( 'NONE', #9438, .T. ) ;
#27237 = CARTESIAN_POINT ( 'NONE',  ( 56.67878100130369035, -27.78182860042797131, 12.49999999999999822 ) ) ;
#27238 = CIRCLE ( 'NONE', #2707, 5.750000000000002665 ) ;
#27239 = FACE_OUTER_BOUND ( 'NONE', #16920, .T. ) ;
#27240 = AXIS2_PLACEMENT_3D ( 'NONE', #9073, #17894, #11691 ) ;
#27241 = CARTESIAN_POINT ( 'NONE',  ( -85.00000337463092137, 25.98076211353317433, 12.50000000000000000 ) ) ;
#27242 = EDGE_CURVE ( 'NONE', #11718, #5095, #27632, .T. ) ;
#27243 = ORIENTED_EDGE ( 'NONE', *, *, #11667, .T. ) ;
#27244 = FACE_OUTER_BOUND ( 'NONE', #18772, .T. ) ;
#27245 = ORIENTED_EDGE ( 'NONE', *, *, #14044, .T. ) ;
#27246 = DIRECTION ( 'NONE',  ( 1.000000000000000000, 0.000000000000000000, 0.000000000000000000 ) ) ;
#27247 = DIRECTION ( 'NONE',  ( 1.000000000000000000, 0.000000000000000000, 0.000000000000000000 ) ) ;
#27248 = CARTESIAN_POINT ( 'NONE',  ( -101.7384897088135887, 110.2237710830547286, 32.50000000000000000 ) ) ;
#27249 = DIRECTION ( 'NONE',  ( 0.000000000000000000, 0.000000000000000000, 1.000000000000000000 ) ) ;
#27250 = CARTESIAN_POINT ( 'NONE',  ( -55.00000337463110611, -43.30127018922202353, -9.999999999999998224 ) ) ;
#27251 = EDGE_CURVE ( 'NONE', #32864, #29787, #12273, .T. ) ;
#27252 = FACE_OUTER_BOUND ( 'NONE', #35181, .T. ) ;
#27253 = CIRCLE ( 'NONE', #32018, 2.000000000000001776 ) ;
#27254 = EDGE_CURVE ( 'NONE', #24009, #13023, #17675, .T. ) ;
#27255 = DIRECTION ( 'NONE',  ( -0.7650473262243671080, -0.6439740589782688707, 0.000000000000000000 ) ) ;
#27256 = ORIENTED_EDGE ( 'NONE', *, *, #16020, .T. ) ;
#27258 = CIRCLE ( 'NONE', #21293, 2.000000000000000000 ) ;
#27257 = CYLINDRICAL_SURFACE ( 'NONE', #1625, 2.000000000000001776 ) ;
#27259 = EDGE_CURVE ( 'NONE', #20619, #21307, #21885, .T. ) ;
#27260 = DIRECTION ( 'NONE',  ( -1.000000000000000000, 0.000000000000000000, 0.000000000000000000 ) ) ;
#27261 = LINE ( 'NONE', #10224, #26504 ) ;
#27262 = CIRCLE ( 'NONE', #28461, 33.00000000000001421 ) ;
#27263 = CIRCLE ( 'NONE', #16483, 2.000000000000000000 ) ;
#27264 = VERTEX_POINT ( 'NONE', #10218 ) ;
#27265 = VECTOR ( 'NONE', #8200, 1000.000000000000000 ) ;
#27266 = ORIENTED_EDGE ( 'NONE', *, *, #20040, .F. ) ;
#27267 = VERTEX_POINT ( 'NONE', #21646 ) ;
#27268 = DIRECTION ( 'NONE',  ( 0.000000000000000000, 0.000000000000000000, 1.000000000000000000 ) ) ;
#27269 = CARTESIAN_POINT ( 'NONE',  ( -75.00000337463097821, -8.660254037844422825, -9.999999999999998224 ) ) ;
#27270 = EDGE_LOOP ( 'NONE', ( #6647, #27636, #32455, #28236 ) ) ;
#27271 = AXIS2_PLACEMENT_3D ( 'NONE', #21674, #21113, #36114 ) ;
#27272 = AXIS2_PLACEMENT_3D ( 'NONE', #21689, #33689, #15882 ) ;
#27273 = CARTESIAN_POINT ( 'NONE',  ( -4.999999999999999112, 0.4881033300985041512, -6.000000000000000000 ) ) ;
#27274 = EDGE_CURVE ( 'NONE', #35191, #15953, #27454, .T. ) ;
#27275 = CARTESIAN_POINT ( 'NONE',  ( -63.00000337463102085, 60.62177826491077326, 12.50000000000000000 ) ) ;
#27276 = ORIENTED_EDGE ( 'NONE', *, *, #25213, .T. ) ;
#27277 = DIRECTION ( 'NONE',  ( 0.000000000000000000, 0.000000000000000000, -1.000000000000000000 ) ) ;
#27278 = EDGE_LOOP ( 'NONE', ( #9055, #26281, #7114 ) ) ;
#27279 = CYLINDRICAL_SURFACE ( 'NONE', #2767, 2.000000000000000000 ) ;
#27280 = DIRECTION ( 'NONE',  ( 1.000000000000000000, 0.000000000000000000, 0.000000000000000000 ) ) ;
#27281 = CARTESIAN_POINT ( 'NONE',  ( 0.000000000000000000, 0.000000000000000000, 27.50000000000000000 ) ) ;
#27282 = CIRCLE ( 'NONE', #27900, 3.000000000000002665 ) ;
#27283 = PLANE ( 'NONE',  #7424 ) ;
#27284 = AXIS2_PLACEMENT_3D ( 'NONE', #7905, #2280, #19340 ) ;
#27285 = ORIENTED_EDGE ( 'NONE', *, *, #36428, .T. ) ;
#27286 = CYLINDRICAL_SURFACE ( 'NONE', #912, 3.000000000000002665 ) ;
#27287 = AXIS2_PLACEMENT_3D ( 'NONE', #24136, #21130, #7078 ) ;
#27288 = ITEM_DEFINED_TRANSFORMATION ( 'NONE', 'NONE', #5781,  #21385 ) ;
#27289 = CIRCLE ( 'NONE', #25506, 2.000000000000001776 ) ;
#27290 = LINE ( 'NONE', #16065, #30238 ) ;
#27291 = DIRECTION ( 'NONE',  ( 0.000000000000000000, 0.000000000000000000, 1.000000000000000000 ) ) ;
#27292 = EDGE_CURVE ( 'NONE', #7532, #24583, #29656, .T. ) ;
#27293 = DIRECTION ( 'NONE',  ( 0.000000000000000000, 0.000000000000000000, 1.000000000000000000 ) ) ;
#27294 = CARTESIAN_POINT ( 'NONE',  ( 19.99999662536858835, 69.28203230275516944, -9.999999999999998224 ) ) ;
#27295 = EDGE_LOOP ( 'NONE', ( #12834, #23568, #1111, #13706 ) ) ;
#27296 = ADVANCED_FACE ( 'NONE', ( #16770 ), #59, .F. ) ;
#27297 = DIRECTION ( 'NONE',  ( 0.000000000000000000, 0.000000000000000000, 1.000000000000000000 ) ) ;
#27298 = CIRCLE ( 'NONE', #1549, 2.000000000000001776 ) ;
#27299 = DIRECTION ( 'NONE',  ( 0.000000000000000000, 0.000000000000000000, 1.000000000000000000 ) ) ;
#27300 = CARTESIAN_POINT ( 'NONE',  ( 54.99999662536844625, 60.62177826491077326, -5.000000000000000000 ) ) ;
#27301 = AXIS2_PLACEMENT_3D ( 'NONE', #24148, #21705, #35603 ) ;
#27302 = EDGE_LOOP ( 'NONE', ( #9015, #16582, #23470, #5487 ) ) ;
#27303 = ORIENTED_EDGE ( 'NONE', *, *, #2455, .T. ) ;
#27304 = ADVANCED_FACE ( 'NONE', ( #2680 ), #36639, .F. ) ;
#27305 = CARTESIAN_POINT ( 'NONE',  ( 52.99999662536844625, 60.62177826491077326, -9.999999999999998224 ) ) ;
#27306 = CARTESIAN_POINT ( 'NONE',  ( 82.99999662536831124, -25.98076211353319565, 17.49999999999999645 ) ) ;
#27307 = CIRCLE ( 'NONE', #17727, 2.541999999999999815 ) ;
#27308 = LINE ( 'NONE', #24522, #35072 ) ;
#27309 = ORIENTED_EDGE ( 'NONE', *, *, #21506, .T. ) ;
#27310 = AXIS2_PLACEMENT_3D ( 'NONE', #9965, #21409, #32852 ) ;
#27311 = DIRECTION ( 'NONE',  ( 0.000000000000000000, 0.000000000000000000, -1.000000000000000000 ) ) ;
#27312 = DIRECTION ( 'NONE',  ( -1.000000000000000000, -8.994862468027883963E-15, 0.000000000000000000 ) ) ;
#27313 = CARTESIAN_POINT ( 'NONE',  ( 73.47608876694671665, 59.13646009116074964, 12.49999999999999822 ) ) ;
#27314 = VECTOR ( 'NONE', #14673, 1000.000000000000000 ) ;
#27315 = AXIS2_PLACEMENT_3D ( 'NONE', #22002, #13360, #27622 ) ;
#27316 = CYLINDRICAL_SURFACE ( 'NONE', #3472, 2.000000000000001776 ) ;
#27317 = EDGE_CURVE ( 'NONE', #20745, #7037, #1508, .T. ) ;
#27318 = VECTOR ( 'NONE', #3703, 1000.000000000000000 ) ;
#27319 = EDGE_LOOP ( 'NONE', ( #15281, #707 ) ) ;
#27320 = VECTOR ( 'NONE', #34572, 1000.000000000000000 ) ;
#27322 = ORIENTED_EDGE ( 'NONE', *, *, #20563, .T. ) ;
#27321 = EDGE_CURVE ( 'NONE', #6252, #35994, #33858, .T. ) ;
#27323 = DIRECTION ( 'NONE',  ( 1.000000000000000000, 0.000000000000000000, 0.000000000000000000 ) ) ;
#27324 = AXIS2_PLACEMENT_3D ( 'NONE', #5582, #6134, #20550 ) ;
#27325 = ADVANCED_FACE ( 'NONE', ( #25379 ), #2507, .T. ) ;
#27326 = DIRECTION ( 'NONE',  ( 0.000000000000000000, 0.000000000000000000, 1.000000000000000000 ) ) ;
#27328 = EDGE_CURVE ( 'NONE', #7638, #23807, #16508, .T. ) ;
#27327 = ORIENTED_EDGE ( 'NONE', *, *, #11189, .T. ) ;
#27329 = CARTESIAN_POINT ( 'NONE',  ( -0.8441225671309252609, -5.568793373801227631, -4.176900509771872549 ) ) ;
#27330 = EDGE_LOOP ( 'NONE', ( #28330, #35818, #26847, #11889 ) ) ;
#27331 = DIRECTION ( 'NONE',  ( 1.000000000000000000, 0.000000000000000000, 0.000000000000000000 ) ) ;
#27332 = CIRCLE ( 'NONE', #11741, 3.500000000000003109 ) ;
#27333 = DIRECTION ( 'NONE',  ( 0.000000000000000000, 0.000000000000000000, 1.000000000000000000 ) ) ;
#27334 = VERTEX_POINT ( 'NONE', #34369 ) ;
#27335 = ORIENTED_EDGE ( 'NONE', *, *, #16844, .T. ) ;
#27336 = CARTESIAN_POINT ( 'NONE',  ( 0.000000000000000000, 0.000000000000000000, 27.50000000000000000 ) ) ;
#27337 = ORIENTED_EDGE ( 'NONE', *, *, #17072, .F. ) ;
#27338 = CIRCLE ( 'NONE', #30920, 2.000000000000001776 ) ;
#27339 = DIRECTION ( 'NONE',  ( 0.000000000000000000, 0.000000000000000000, 1.000000000000000000 ) ) ;
#27340 = CIRCLE ( 'NONE', #32749, 2.000000000000001776 ) ;
#27341 = DIRECTION ( 'NONE',  ( 0.000000000000000000, 0.000000000000000000, 1.000000000000000000 ) ) ;
#27342 = CARTESIAN_POINT ( 'NONE',  ( 57.99999662536842493, 51.96152422706639129, 12.50000000000000000 ) ) ;
#27343 = VERTEX_POINT ( 'NONE', #17120 ) ;
#27344 = FACE_OUTER_BOUND ( 'NONE', #9367, .T. ) ;
#27345 = AXIS2_PLACEMENT_3D ( 'NONE', #22835, #8016, #31626 ) ;
#27346 = LINE ( 'NONE', #27151, #29800 ) ;
#27347 = CYLINDRICAL_SURFACE ( 'NONE', #8916, 27.00000000000001066 ) ;
#27348 = VECTOR ( 'NONE', #3414, 1000.000000000000000 ) ;
#27349 = ORIENTED_EDGE ( 'NONE', *, *, #20843, .F. ) ;
#27350 = VECTOR ( 'NONE', #1433, 1000.000000000000000 ) ;
#27351 = EDGE_CURVE ( 'NONE', #18465, #30617, #6922, .T. ) ;
#27352 = CIRCLE ( 'NONE', #18362, 2.000000000000001776 ) ;
#27353 = ORIENTED_EDGE ( 'NONE', *, *, #36770, .T. ) ;
#27354 = AXIS2_PLACEMENT_3D ( 'NONE', #17173, #28601, #3106 ) ;
#27355 = ORIENTED_EDGE ( 'NONE', *, *, #24493, .T. ) ;
#27356 = DIRECTION ( 'NONE',  ( -1.000000000000000000, 0.000000000000000000, 0.000000000000000000 ) ) ;
#27357 = FACE_OUTER_BOUND ( 'NONE', #13248, .T. ) ;
#27358 = ORIENTED_EDGE ( 'NONE', *, *, #21793, .F. ) ;
#27359 = DIRECTION ( 'NONE',  ( 0.000000000000000000, 0.000000000000000000, 1.000000000000000000 ) ) ;
#27360 = DIRECTION ( 'NONE',  ( 0.000000000000000000, 0.000000000000000000, -1.000000000000000000 ) ) ;
#27361 = CARTESIAN_POINT ( 'NONE',  ( -87.00000337463093558, -8.660254037844422825, 12.50000000000000000 ) ) ;
#27362 = VECTOR ( 'NONE', #3406, 1000.000000000000000 ) ;
#27363 = CARTESIAN_POINT ( 'NONE',  ( 124.4080600076931375, 12.15049814296589226, 32.50002500000000083 ) ) ;
#27364 = DIRECTION ( 'NONE',  ( 1.000000000000000000, 0.000000000000000000, 0.000000000000000000 ) ) ;
#27365 = CARTESIAN_POINT ( 'NONE',  ( -47.63139720814438505, -27.49999999999955591, -15.00000000000000000 ) ) ;
#27366 = DIRECTION ( 'NONE',  ( 1.000000000000000000, 0.000000000000000000, 0.000000000000000000 ) ) ;
#27367 = VECTOR ( 'NONE', #17186, 1000.000000000000000 ) ;
#27368 = CYLINDRICAL_SURFACE ( 'NONE', #17847, 2.000000000000001776 ) ;
#27369 = EDGE_LOOP ( 'NONE', ( #35887, #36989 ) ) ;
#27370 = AXIS2_PLACEMENT_3D ( 'NONE', #29840, #21029, #18776 ) ;
#27371 = ORIENTED_EDGE ( 'NONE', *, *, #14217, .F. ) ;
#27372 = DIRECTION ( 'NONE',  ( 1.000000000000000000, 0.000000000000000000, 0.000000000000000000 ) ) ;
#27373 = VECTOR ( 'NONE', #33077, 1000.000000000000000 ) ;
#27374 = DIRECTION ( 'NONE',  ( 0.000000000000000000, 0.000000000000000000, 1.000000000000000000 ) ) ;
#27375 = EDGE_CURVE ( 'NONE', #985, #30974, #27258, .T. ) ;
#27376 = CARTESIAN_POINT ( 'NONE',  ( -32.49191361593891259, -89.27079897466116165, 12.49999999999999822 ) ) ;
#27377 = DIRECTION ( 'NONE',  ( 0.000000000000000000, 0.000000000000000000, 1.000000000000000000 ) ) ;
#27378 = LINE ( 'NONE', #33930, #34452 ) ;
#27379 = ORIENTED_EDGE ( 'NONE', *, *, #30719, .T. ) ;
#27381 = VECTOR ( 'NONE', #36915, 1000.000000000000000 ) ;
#27380 = CARTESIAN_POINT ( 'NONE',  ( -53.00000337463106348, 60.62177826491078747, -5.000000000000000000 ) ) ;
#27382 = CARTESIAN_POINT ( 'NONE',  ( 2.500000000000003109, -4.330127018922192761, -6.000000000000000000 ) ) ;
#27383 = AXIS2_PLACEMENT_3D ( 'NONE', #5547, #466, #11704 ) ;
#27384 = CARTESIAN_POINT ( 'NONE',  ( 5.000000000000000000, -1.349638343847295419, -0.8687551798607463516 ) ) ;
#27385 = EDGE_LOOP ( 'NONE', ( #5692, #15706 ) ) ;
#27386 = CARTESIAN_POINT ( 'NONE',  ( 0.000000000000000000, 89.94802294027088863, 30.49999999999999289 ) ) ;
#27387 = EDGE_LOOP ( 'NONE', ( #17150, #9802, #16969, #34552 ) ) ;
#27388 = AXIS2_PLACEMENT_3D ( 'NONE', #18514, #21503, #29937 ) ;
#27389 =( NAMED_UNIT ( * ) PLANE_ANGLE_UNIT ( ) SI_UNIT ( $, .RADIAN. ) );
#27390 = CARTESIAN_POINT ( 'NONE',  ( 36.00000000000000000, 2.445500000000000007, 0.000000000000000000 ) ) ;
#27391 = AXIS2_PLACEMENT_3D ( 'NONE', #7328, #3761, #15199 ) ;
#27392 = CARTESIAN_POINT ( 'NONE',  ( 81.99999662536833966, 34.64101615137759183, -9.999999999999998224 ) ) ;
#27393 = CIRCLE ( 'NONE', #1647, 2.000000000000001776 ) ;
#27394 = LINE ( 'NONE', #29628, #4084 ) ;
#27395 = ORIENTED_EDGE ( 'NONE', *, *, #34850, .F. ) ;
#27396 = ORIENTED_EDGE ( 'NONE', *, *, #13092, .T. ) ;
#27397 = EDGE_CURVE ( 'NONE', #9870, #34185, #895, .T. ) ;
#27398 = ADVANCED_FACE ( 'NONE', ( #25567 ), #28006, .T. ) ;
#27399 = CIRCLE ( 'NONE', #35789, 2.000000000000001776 ) ;
#27400 = ORIENTED_EDGE ( 'NONE', *, *, #18566, .T. ) ;
#27401 = DIRECTION ( 'NONE',  ( -0.000000000000000000, -0.000000000000000000, 1.000000000000000000 ) ) ;
#27402 = CARTESIAN_POINT ( 'NONE',  ( -82.00000337463094979, -17.32050807568882078, 12.50000000000000000 ) ) ;
#27403 = EDGE_CURVE ( 'NONE', #12539, #12117, #26083, .T. ) ;
#27404 = DIRECTION ( 'NONE',  ( 0.000000000000000000, 0.000000000000000000, 1.000000000000000000 ) ) ;
#27405 = CARTESIAN_POINT ( 'NONE',  ( 11.99999662536865763, -69.28203230275519786, 12.50000000000000000 ) ) ;
#27406 = LINE ( 'NONE', #18419, #10567 ) ;
#27407 = ORIENTED_EDGE ( 'NONE', *, *, #3405, .F. ) ;
#27408 = CYLINDRICAL_SURFACE ( 'NONE', #9322, 3.000000000000000888 ) ;
#27409 = CONICAL_SURFACE ( 'NONE', #33914, 3.000000000000000000, 0.9599310885968762586 ) ;
#27410 = DIRECTION ( 'NONE',  ( -1.000000000000000000, 0.000000000000000000, 0.000000000000000000 ) ) ;
#27411 = EDGE_CURVE ( 'NONE', #5750, #33336, #30869, .T. ) ;
#27412 = CARTESIAN_POINT ( 'NONE',  ( 0.000000000000000000, 101.4832769781154127, -24.97964607176053775 ) ) ;
#27413 = VERTEX_POINT ( 'NONE', #30798 ) ;
#27414 = CARTESIAN_POINT ( 'NONE',  ( 76.99999662536836809, 25.98076211353319565, -9.999999999999998224 ) ) ;
#27415 = DIRECTION ( 'NONE',  ( 0.000000000000000000, 0.000000000000000000, 1.000000000000000000 ) ) ;
#27416 = AXIS2_PLACEMENT_3D ( 'NONE', #3658, #653, #14710 ) ;
#27417 = ORIENTED_EDGE ( 'NONE', *, *, #13867, .F. ) ;
#27418 = ORIENTED_EDGE ( 'NONE', *, *, #27317, .T. ) ;
#27419 = DIRECTION ( 'NONE',  ( 1.000000000000000000, 0.000000000000000000, 0.000000000000000000 ) ) ;
#27420 = EDGE_CURVE ( 'NONE', #10442, #20675, #30257, .T. ) ;
#27421 = CARTESIAN_POINT ( 'NONE',  ( -52.39915983220772233, -35.19434990244957362, -4.999999999999997335 ) ) ;
#27422 = CARTESIAN_POINT ( 'NONE',  ( 3.000000000000000000, 2.935248768560057453, -3.903127820947815962E-15 ) ) ;
#27423 = ORIENTED_EDGE ( 'NONE', *, *, #6843, .T. ) ;
#27424 = ORIENTED_EDGE ( 'NONE', *, *, #5728, .F. ) ;
#27425 = VECTOR ( 'NONE', #14544, 1000.000000000000000 ) ;
#27426 = ORIENTED_EDGE ( 'NONE', *, *, #23505, .F. ) ;
#27427 = CIRCLE ( 'NONE', #23224, 2.000000000000001776 ) ;
#27428 = FACE_OUTER_BOUND ( 'NONE', #19825, .T. ) ;
#27429 = EDGE_LOOP ( 'NONE', ( #34032, #5394, #22085, #29866, #33552, #19042 ) ) ;
#27430 = DIRECTION ( 'NONE',  ( -1.000000000000000000, 0.000000000000000000, 0.000000000000000000 ) ) ;
#27431 = VERTEX_POINT ( 'NONE', #16574 ) ;
#27432 = VERTEX_POINT ( 'NONE', #2332 ) ;
#27433 = CIRCLE ( 'NONE', #2281, 2.000000000000000000 ) ;
#27434 = DIRECTION ( 'NONE',  ( 0.000000000000000000, 0.000000000000000000, 1.000000000000000000 ) ) ;
#27435 = EDGE_CURVE ( 'NONE', #4953, #1362, #10510, .T. ) ;
#27436 = CARTESIAN_POINT ( 'NONE',  ( 47.63139720814418610, 27.49999999999988987, -15.00000000000000000 ) ) ;
#27437 = ORIENTED_EDGE ( 'NONE', *, *, #27403, .T. ) ;
#27438 = ORIENTED_EDGE ( 'NONE', *, *, #32320, .F. ) ;
#27439 = CARTESIAN_POINT ( 'NONE',  ( 84.99999662536832545, 8.660254037844394404, -9.999999999999998224 ) ) ;
#27440 = CIRCLE ( 'NONE', #13688, 3.000000000000000444 ) ;
#27441 = DIRECTION ( 'NONE',  ( 0.000000000000000000, 0.000000000000000000, 1.000000000000000000 ) ) ;
#27442 = CARTESIAN_POINT ( 'NONE',  ( 36.99999662536855283, -77.94228634059960825, -5.000000000000000000 ) ) ;
#27443 = FACE_OUTER_BOUND ( 'NONE', #2889, .T. ) ;
#27444 = ORIENTED_EDGE ( 'NONE', *, *, #29791, .T. ) ;
#27445 = CARTESIAN_POINT ( 'NONE',  ( 61.99999662536842493, -51.96152422706639840, 12.50000000000000000 ) ) ;
#27446 = CIRCLE ( 'NONE', #3527, 2.000000000000001776 ) ;
#27447 = ORIENTED_EDGE ( 'NONE', *, *, #23402, .F. ) ;
#27448 = CARTESIAN_POINT ( 'NONE',  ( 68.19434990244977257, -52.39915983220758022, -4.999999999999997335 ) ) ;
#27449 = ADVANCED_FACE ( 'NONE', ( #5505 ), #11317, .T. ) ;
#27450 = CIRCLE ( 'NONE', #11286, 1.999999999999998224 ) ;
#27451 = CYLINDRICAL_SURFACE ( 'NONE', #18411, 3.000000000000002665 ) ;
#27452 = CARTESIAN_POINT ( 'NONE',  ( 51.68138994340220904, -113.8157894736842053, 27.50000000000000000 ) ) ;
#27453 = DIRECTION ( 'NONE',  ( 0.000000000000000000, 0.000000000000000000, 1.000000000000000000 ) ) ;
#27455 = CIRCLE ( 'NONE', #500, 3.000000000000002665 ) ;
#27454 = LINE ( 'NONE', #1773, #7515 ) ;
#27456 = CARTESIAN_POINT ( 'NONE',  ( -63.00000337463102085, 25.98076211353317433, 12.50000000000000000 ) ) ;
#27457 = EDGE_CURVE ( 'NONE', #34186, #19449, #3616, .T. ) ;
#27458 = CIRCLE ( 'NONE', #12479, 2.000000000000001776 ) ;
#27459 = DIRECTION ( 'NONE',  ( 1.000000000000000000, 0.000000000000000000, 0.000000000000000000 ) ) ;
#27460 = VERTEX_POINT ( 'NONE', #14861 ) ;
#27461 = DIRECTION ( 'NONE',  ( 0.000000000000000000, 0.000000000000000000, 1.000000000000000000 ) ) ;
#27462 = DIRECTION ( 'NONE',  ( 0.000000000000000000, 0.000000000000000000, 1.000000000000000000 ) ) ;
#27463 = CARTESIAN_POINT ( 'NONE',  ( 64.99999662536839651, 60.62177826491078747, 12.50000000000000000 ) ) ;
#27464 = AXIS2_PLACEMENT_3D ( 'NONE', #22345, #8098, #19539 ) ;
#27465 = VERTEX_POINT ( 'NONE', #6058 ) ;
#27466 = CIRCLE ( 'NONE', #8315, 2.000000000000001776 ) ;
#27467 = VERTEX_POINT ( 'NONE', #29288 ) ;
#27468 = VERTEX_POINT ( 'NONE', #18210 ) ;
#27469 = FACE_OUTER_BOUND ( 'NONE', #11937, .T. ) ;
#27470 = DIRECTION ( 'NONE',  ( 0.000000000000000000, 0.000000000000000000, 1.000000000000000000 ) ) ;
#27471 = ORIENTED_EDGE ( 'NONE', *, *, #23989, .F. ) ;
#27472 = LINE ( 'NONE', #18851, #32289 ) ;
#27473 = EDGE_CURVE ( 'NONE', #25535, #691, #9295, .T. ) ;
#27474 = VECTOR ( 'NONE', #28089, 1000.000000000000000 ) ;
#27475 = CARTESIAN_POINT ( 'NONE',  ( 2.500000000000000444, 0.000000000000000000, 1.716666666667001406 ) ) ;
#27476 = ORIENTED_EDGE ( 'NONE', *, *, #12359, .T. ) ;
#27477 = LINE ( 'NONE', #4967, #26950 ) ;
#27478 = EDGE_LOOP ( 'NONE', ( #29810, #14469, #11835, #12566 ) ) ;
#27479 = VECTOR ( 'NONE', #9252, 1000.000000000000000 ) ;
#27480 = CARTESIAN_POINT ( 'NONE',  ( -35.00000337463116296, 60.62177826491077326, -5.000000000000000000 ) ) ;
#27481 = EDGE_CURVE ( 'NONE', #105, #4760, #14085, .T. ) ;
#27482 = CARTESIAN_POINT ( 'NONE',  ( 2.500000000000000000, 0.000000000000000000, -6.000000000000000000 ) ) ;
#27483 = FACE_OUTER_BOUND ( 'NONE', #18426, .T. ) ;
#27484 = CIRCLE ( 'NONE', #1146, 1.999999999999998224 ) ;
#27485 = ADVANCED_FACE ( 'NONE', ( #26106 ), #32463, .T. ) ;
#27486 = LINE ( 'NONE', #33494, #12780 ) ;
#27487 = ORIENTED_EDGE ( 'NONE', *, *, #21432, .T. ) ;
#27488 = CARTESIAN_POINT ( 'NONE',  ( 0.000000000000000000, 0.000000000000000000, 17.49999999999999645 ) ) ;
#27489 = AXIS2_PLACEMENT_3D ( 'NONE', #20573, #26227, #26409 ) ;
#27490 = CARTESIAN_POINT ( 'NONE',  ( 4.390739357591696154E-15, -5.773502691896305272, -5.700000000000000178 ) ) ;
#27491 = CARTESIAN_POINT ( 'NONE',  ( -3.374631327851540519E-06, 86.60254037844397601, -9.999999999999998224 ) ) ;
#27492 = CIRCLE ( 'NONE', #8940, 2.000000000000001776 ) ;
#27493 = ORIENTED_EDGE ( 'NONE', *, *, #29357, .F. ) ;
#27494 = LINE ( 'NONE', #7428, #4823 ) ;
#27495 = CARTESIAN_POINT ( 'NONE',  ( -75.00000337463099243, -25.98076211353322051, -9.999999999999998224 ) ) ;
#27496 = ORIENTED_EDGE ( 'NONE', *, *, #2072, .T. ) ;
#27497 = AXIS2_PLACEMENT_3D ( 'NONE', #4872, #36170, #16125 ) ;
#27498 = DIRECTION ( 'NONE',  ( 0.000000000000000000, 0.000000000000000000, 1.000000000000000000 ) ) ;
#27499 = CYLINDRICAL_SURFACE ( 'NONE', #26867, 33.00000000000001421 ) ;
#27500 = CARTESIAN_POINT ( 'NONE',  ( 76.71706219562628348, -9.685771384082237034, -5.000000000000000000 ) ) ;
#27501 = ORIENTED_EDGE ( 'NONE', *, *, #21690, .F. ) ;
#27502 = EDGE_CURVE ( 'NONE', #21745, #8482, #11849, .T. ) ;
#27503 = CIRCLE ( 'NONE', #5358, 2.000000000000001776 ) ;
#27504 = ORIENTED_EDGE ( 'NONE', *, *, #11175, .T. ) ;
#27505 = AXIS2_PLACEMENT_3D ( 'NONE', #4768, #19012, #35699 ) ;
#27506 = CARTESIAN_POINT ( 'NONE',  ( 104.8061974404897683, -19.22934205795014151, 27.50000000000000000 ) ) ;
#27507 = CARTESIAN_POINT ( 'NONE',  ( -5.253368672218637236, 3.033033817057754877, -4.359491423763649287 ) ) ;
#27508 = DIRECTION ( 'NONE',  ( 0.000000000000000000, 0.000000000000000000, 1.000000000000000000 ) ) ;
#27509 = ORIENTED_EDGE ( 'NONE', *, *, #32427, .T. ) ;
#27510 = AXIS2_PLACEMENT_3D ( 'NONE', #15847, #23937, #21661 ) ;
#27511 = FACE_OUTER_BOUND ( 'NONE', #21515, .T. ) ;
#27512 = DIRECTION ( 'NONE',  ( -1.000000000000000000, 0.000000000000000000, 0.000000000000000000 ) ) ;
#27513 = DIRECTION ( 'NONE',  ( 0.000000000000000000, 0.000000000000000000, 1.000000000000000000 ) ) ;
#27515 = CARTESIAN_POINT ( 'NONE',  ( 54.99999662536844625, 43.30127018922198801, 17.49999999999999645 ) ) ;
#27514 = CIRCLE ( 'NONE', #25734, 2.000000000000001776 ) ;
#27516 = VERTEX_POINT ( 'NONE', #780 ) ;
#27517 = VERTEX_POINT ( 'NONE', #9046 ) ;
#27518 = SURFACE_STYLE_USAGE ( .BOTH. , #10092 ) ;
#27519 = AXIS2_PLACEMENT_3D ( 'NONE', #9111, #35196, #20936 ) ;
#27520 = EDGE_CURVE ( 'NONE', #23651, #17786, #17093, .T. ) ;
#27521 = DIRECTION ( 'NONE',  ( 0.000000000000000000, 0.000000000000000000, 1.000000000000000000 ) ) ;
#27522 = ORIENTED_EDGE ( 'NONE', *, *, #12992, .T. ) ;
#27523 = ADVANCED_FACE ( 'NONE', ( #12193 ), #23663, .T. ) ;
#27524 = FACE_BOUND ( 'NONE', #24838, .T. ) ;
#27525 = EDGE_LOOP ( 'NONE', ( #8076, #18649, #10137, #30765 ) ) ;
#27526 = EDGE_CURVE ( 'NONE', #36755, #20745, #15217, .T. ) ;
#27527 = DIRECTION ( 'NONE',  ( 0.000000000000000000, 0.000000000000000000, 1.000000000000000000 ) ) ;
#27528 = EDGE_CURVE ( 'NONE', #2589, #14801, #27874, .T. ) ;
#27529 = LINE ( 'NONE', #21534, #534 ) ;
#27530 = AXIS2_PLACEMENT_3D ( 'NONE', #17394, #37093, #28812 ) ;
#27531 = EDGE_LOOP ( 'NONE', ( #6937, #14258 ) ) ;
#27532 = EDGE_CURVE ( 'NONE', #36216, #33068, #32022, .T. ) ;
#27533 = VECTOR ( 'NONE', #23560, 1000.000000000000000 ) ;
#27534 = CYLINDRICAL_SURFACE ( 'NONE', #26039, 2.000000000000000000 ) ;
#27535 = EDGE_LOOP ( 'NONE', ( #25912, #11284, #5434, #34889 ) ) ;
#27536 = ADVANCED_FACE ( 'NONE', ( #35316 ), #414, .F. ) ;
#27537 = DIRECTION ( 'NONE',  ( -0.000000000000000000, -0.000000000000000000, -1.000000000000000000 ) ) ;
#27538 = DIRECTION ( 'NONE',  ( -1.000000000000000000, 0.000000000000000000, 0.000000000000000000 ) ) ;
#27539 = DIRECTION ( 'NONE',  ( -1.000000000000000000, 0.000000000000000000, -0.000000000000000000 ) ) ;
#27540 = VERTEX_POINT ( 'NONE', #3232 ) ;
#27541 = CARTESIAN_POINT ( 'NONE',  ( -75.00000337463099243, -25.98076211353322051, -9.999999999999998224 ) ) ;
#27542 = DIRECTION ( 'NONE',  ( -1.000000000000000000, 0.000000000000000000, 0.000000000000000000 ) ) ;
#27543 = CARTESIAN_POINT ( 'NONE',  ( -4.592054218142291866, -3.122278952918454031, -5.689399939901067071 ) ) ;
#27544 = AXIS2_PLACEMENT_3D ( 'NONE', #1048, #12473, #26540 ) ;
#27545 = EDGE_CURVE ( 'NONE', #31097, #5072, #21035, .T. ) ;
#27546 = ORIENTED_EDGE ( 'NONE', *, *, #21291, .F. ) ;
#27547 = B_SPLINE_CURVE_WITH_KNOTS ( 'NONE', 3,
 ( #16937, #8501, #13932, #19767, #33463, #17121, #2683, #28361, #25570, #33644, #37011, #11318, #5135, #34209, #30630, #19219, #31193, #25030 ),
 .UNSPECIFIED., .F., .F.,
 ( 4, 2, 2, 2, 2, 2, 2, 2, 4 ),
 ( 0.1412743459061075735, 0.2309557491716168476, 0.3206371524371260939, 0.4103185557026353125, 0.4999999589681445311, 0.5896813622336537497, 0.6793627654991629683, 0.7690441687646720759, 0.8587255720301810724 ),
 .UNSPECIFIED. ) ;
#27548 = ADVANCED_FACE ( 'NONE', ( #31891 ), #25926, .F. ) ;
#27549 = ORIENTED_EDGE ( 'NONE', *, *, #31420, .T. ) ;
#27550 = EDGE_LOOP ( 'NONE', ( #35332, #2158, #3913, #2629, #13692, #11791 ) ) ;
#27551 = EDGE_CURVE ( 'NONE', #32323, #36578, #24896, .T. ) ;
#27552 = ADVANCED_FACE ( 'NONE', ( #613 ), #12026, .F. ) ;
#27553 = VECTOR ( 'NONE', #31006, 1000.000000000000000 ) ;
#27554 = DIRECTION ( 'NONE',  ( 0.000000000000000000, 0.000000000000000000, 1.000000000000000000 ) ) ;
#27556 = EDGE_CURVE ( 'NONE', #12740, #1358, #6418, .T. ) ;
#27555 = VERTEX_POINT ( 'NONE', #32080 ) ;
#27557 = CARTESIAN_POINT ( 'NONE',  ( -4.999999999999999112, -1.831125658499874964, -1.158123955083390388 ) ) ;
#27558 = AXIS2_PLACEMENT_3D ( 'NONE', #16340, #36211, #27756 ) ;
#27559 = CARTESIAN_POINT ( 'NONE',  ( -28.00000337463118427, 69.28203230275516944, 17.49999999999999645 ) ) ;
#27560 = DIRECTION ( 'NONE',  ( 0.000000000000000000, 0.000000000000000000, -1.000000000000000000 ) ) ;
#27561 = VECTOR ( 'NONE', #28946, 1000.000000000000000 ) ;
#27562 = DIRECTION ( 'NONE',  ( 1.000000000000000000, 0.000000000000000000, 0.000000000000000000 ) ) ;
#27563 = CYLINDRICAL_SURFACE ( 'NONE', #13079, 3.500000000000003109 ) ;
#27564 = DIRECTION ( 'NONE',  ( 1.000000000000000000, -0.000000000000000000, 0.000000000000000000 ) ) ;
#27565 = AXIS2_PLACEMENT_3D ( 'NONE', #35002, #20382, #23203 ) ;
#27566 = DIRECTION ( 'NONE',  ( 1.000000000000000000, 0.000000000000000000, 0.000000000000000000 ) ) ;
#27567 = DIRECTION ( 'NONE',  ( 0.000000000000000000, 0.000000000000000000, 1.000000000000000000 ) ) ;
#27568 = VERTEX_POINT ( 'NONE', #35488 ) ;
#27569 = ORIENTED_EDGE ( 'NONE', *, *, #7395, .F. ) ;
#27570 = CARTESIAN_POINT ( 'NONE',  ( -30.99999999999944933, 58.88972745734214698, -49.86561046011506448 ) ) ;
#27571 = CARTESIAN_POINT ( 'NONE',  ( 49.99999662536846756, -69.28203230275519786, -9.999999999999998224 ) ) ;
#27572 = VECTOR ( 'NONE', #15618, 1000.000000000000000 ) ;
#27573 = CARTESIAN_POINT ( 'NONE',  ( 11.64412580323855018, 85.46375187899521109, 12.50000000000000000 ) ) ;
#27574 = ORIENTED_EDGE ( 'NONE', *, *, #12008, .T. ) ;
#27575 = PRODUCT_DEFINITION_CONTEXT ( 'detailed design', #316, 'design' ) ;
#27576 = CARTESIAN_POINT ( 'NONE',  ( -52.00000337463109190, 51.96152422706637708, 17.49999999999999645 ) ) ;
#27577 = DIRECTION ( 'NONE',  ( 0.000000000000000000, 0.000000000000000000, -1.000000000000000000 ) ) ;
#27578 = ORIENTED_EDGE ( 'NONE', *, *, #7539, .T. ) ;
#27579 = AXIS2_PLACEMENT_3D ( 'NONE', #567, #11444, #3028 ) ;
#27580 = CARTESIAN_POINT ( 'NONE',  ( 3.000000000000000000, -2.935248768560059229, 3.469446951953614189E-15 ) ) ;
#27581 = VECTOR ( 'NONE', #24366, 1000.000000000000000 ) ;
#27582 = ORIENTED_EDGE ( 'NONE', *, *, #2811, .T. ) ;
#27583 = CARTESIAN_POINT ( 'NONE',  ( -63.00000337463104927, -43.30127018922202353, -9.999999999999998224 ) ) ;
#27584 = DIRECTION ( 'NONE',  ( 1.000000000000000000, 0.000000000000000000, 0.000000000000000000 ) ) ;
#27585 = CARTESIAN_POINT ( 'NONE',  ( 0.3476802294499899415, 5.572769417831398897, -1.687189089856316215 ) ) ;
#27586 = ORIENTED_EDGE ( 'NONE', *, *, #12272, .T. ) ;
#27587 = ORIENTED_EDGE ( 'NONE', *, *, #34306, .T. ) ;
#27588 = LINE ( 'NONE', #23910, #24576 ) ;
#27589 = ORIENTED_EDGE ( 'NONE', *, *, #14044, .F. ) ;
#27590 = DIRECTION ( 'NONE',  ( 0.000000000000000000, 0.000000000000000000, 1.000000000000000000 ) ) ;
#27591 = ADVANCED_FACE ( 'NONE', ( #18976 ), #33410, .F. ) ;
#27592 = DIRECTION ( 'NONE',  ( 0.000000000000000000, 0.000000000000000000, 1.000000000000000000 ) ) ;
#27593 = DIRECTION ( 'NONE',  ( 0.000000000000000000, 0.000000000000000000, -1.000000000000000000 ) ) ;
#27594 = CARTESIAN_POINT ( 'NONE',  ( -82.00000337463094979, 34.64101615137757051, -9.999999999999998224 ) ) ;
#27595 = DIRECTION ( 'NONE',  ( 1.000000000000000000, 0.000000000000000000, 0.000000000000000000 ) ) ;
#27596 = ORIENTED_EDGE ( 'NONE', *, *, #22780, .F. ) ;
#27597 = LINE ( 'NONE', #33206, #26613 ) ;
#27598 = DIRECTION ( 'NONE',  ( 0.000000000000000000, 0.000000000000000000, 1.000000000000000000 ) ) ;
#27599 = CIRCLE ( 'NONE', #28794, 33.00000000000002132 ) ;
#27600 = ORIENTED_EDGE ( 'NONE', *, *, #33713, .T. ) ;
#27601 = CARTESIAN_POINT ( 'NONE',  ( -80.00000337463094979, 17.32050807568878525, -9.999999999999998224 ) ) ;
#27602 = CARTESIAN_POINT ( 'NONE',  ( 7.999996625368656744, -69.28203230275519786, 12.50000000000000000 ) ) ;
#27603 = ORIENTED_EDGE ( 'NONE', *, *, #9736, .F. ) ;
#27604 = EDGE_LOOP ( 'NONE', ( #34765, #13813, #24133, #32161, #32224, #36555 ) ) ;
#27605 = FACE_OUTER_BOUND ( 'NONE', #11884, .T. ) ;
#27606 = DIRECTION ( 'NONE',  ( -0.000000000000000000, -0.000000000000000000, 1.000000000000000000 ) ) ;
#27607 = DIRECTION ( 'NONE',  ( 0.000000000000000000, 0.000000000000000000, 1.000000000000000000 ) ) ;
#27608 = ORIENTED_EDGE ( 'NONE', *, *, #32688, .F. ) ;
#27609 = ORIENTED_EDGE ( 'NONE', *, *, #19094, .F. ) ;
#27610 = VERTEX_POINT ( 'NONE', #15608 ) ;
#27611 = EDGE_CURVE ( 'NONE', #20763, #25354, #1536, .T. ) ;
#27612 = DIRECTION ( 'NONE',  ( 0.000000000000000000, 0.000000000000000000, 1.000000000000000000 ) ) ;
#27613 = ORIENTED_EDGE ( 'NONE', *, *, #17926, .T. ) ;
#27614 = DIRECTION ( 'NONE',  ( 1.000000000000000000, 0.000000000000000000, 0.000000000000000000 ) ) ;
#27615 = ORIENTED_EDGE ( 'NONE', *, *, #35657, .T. ) ;
#27616 = ORIENTED_EDGE ( 'NONE', *, *, #150, .F. ) ;
#27617 = CYLINDRICAL_SURFACE ( 'NONE', #10044, 2.000000000000001776 ) ;
#27618 = CYLINDRICAL_SURFACE ( 'NONE', #15286, 2.000000000000001776 ) ;
#27619 = EDGE_LOOP ( 'NONE', ( #32923, #16405, #4767 ) ) ;
#27620 = ORIENTED_EDGE ( 'NONE', *, *, #15312, .T. ) ;
#27621 = CYLINDRICAL_SURFACE ( 'NONE', #37096, 6.000000000000005329 ) ;
#27622 = DIRECTION ( 'NONE',  ( 1.000000000000000000, 0.000000000000000000, 0.000000000000000000 ) ) ;
#27623 = FACE_OUTER_BOUND ( 'NONE', #33010, .T. ) ;
#27624 = DIRECTION ( 'NONE',  ( 0.8660254037844344888, -0.5000000000000071054, 0.000000000000000000 ) ) ;
#27625 = ORIENTED_EDGE ( 'NONE', *, *, #27053, .F. ) ;
#27626 = CARTESIAN_POINT ( 'NONE',  ( 69.99999662536841072, 51.96152422706640550, 17.49999999999999645 ) ) ;
#27627 = ADVANCED_FACE ( 'NONE', ( #10523 ), #18421, .F. ) ;
#27628 = FACE_BOUND ( 'NONE', #29718, .T. ) ;
#27629 = CARTESIAN_POINT ( 'NONE',  ( 76.99999662536836809, 25.98076211353319565, -5.000000000000000000 ) ) ;
#27630 = CARTESIAN_POINT ( 'NONE',  ( 0.000000000000000000, 0.000000000000000000, -5.000000000000000000 ) ) ;
#27631 = CARTESIAN_POINT ( 'NONE',  ( 77.93343913441695747, 72.12058696850802164, 27.50000000000000000 ) ) ;
#27632 = LINE ( 'NONE', #1575, #25475 ) ;
#27633 = DIRECTION ( 'NONE',  ( -1.000000000000000000, 0.000000000000000000, 0.000000000000000000 ) ) ;
#27634 = CIRCLE ( 'NONE', #4304, 2.541999999999999815 ) ;
#27635 = PLANE ( 'NONE',  #25360 ) ;
#27636 = ORIENTED_EDGE ( 'NONE', *, *, #7785, .T. ) ;
#27637 = CARTESIAN_POINT ( 'NONE',  ( -50.00000337463110611, -69.28203230275519786, -5.000000000000000000 ) ) ;
#27638 = CIRCLE ( 'NONE', #30020, 33.00000000000001421 ) ;
#27639 = CARTESIAN_POINT ( 'NONE',  ( -83.00000337463092137, 8.660254037844389075, 17.49999999999999645 ) ) ;
#27640 = CARTESIAN_POINT ( 'NONE',  ( -62.00000337463108480, -51.96152422706641971, -9.999999999999998224 ) ) ;
#27641 = ORIENTED_EDGE ( 'NONE', *, *, #23189, .F. ) ;
#27642 = ORIENTED_EDGE ( 'NONE', *, *, #21556, .T. ) ;
#27643 = EDGE_LOOP ( 'NONE', ( #8487, #32050 ) ) ;
#27644 = EDGE_CURVE ( 'NONE', #7812, #11869, #9967, .T. ) ;
#27645 = CARTESIAN_POINT ( 'NONE',  ( -67.00000337463102085, 60.62177826491077326, 12.50000000000000000 ) ) ;
#27646 = DIRECTION ( 'NONE',  ( -0.000000000000000000, -0.000000000000000000, -1.000000000000000000 ) ) ;
#27647 = ORIENTED_EDGE ( 'NONE', *, *, #11736, .T. ) ;
#27648 = EDGE_CURVE ( 'NONE', #745, #27432, #31401, .T. ) ;
#27649 = LINE ( 'NONE', #27823, #22113 ) ;
#27650 = CARTESIAN_POINT ( 'NONE',  ( -70.00000337463100664, -17.32050807568882078, 12.50000000000000000 ) ) ;
#27651 = VERTEX_POINT ( 'NONE', #13162 ) ;
#27652 = DIRECTION ( 'NONE',  ( -0.000000000000000000, -0.000000000000000000, -1.000000000000000000 ) ) ;
#27653 = EDGE_CURVE ( 'NONE', #7366, #32947, #29689, .T. ) ;
#27654 = ORIENTED_EDGE ( 'NONE', *, *, #16174, .F. ) ;
#27655 = FACE_BOUND ( 'NONE', #25693, .T. ) ;
#27656 = EDGE_CURVE ( 'NONE', #26265, #16950, #23710, .T. ) ;
#27657 = DIRECTION ( 'NONE',  ( 0.000000000000000000, 0.000000000000000000, 1.000000000000000000 ) ) ;
#27658 = CARTESIAN_POINT ( 'NONE',  ( 0.8653900595644530291, -5.556556492855614593, -4.190801088233106597 ) ) ;
#27659 = DIRECTION ( 'NONE',  ( 0.000000000000000000, 0.000000000000000000, 1.000000000000000000 ) ) ;
#27660 = ORIENTED_EDGE ( 'NONE', *, *, #10867, .F. ) ;
#27661 = DIRECTION ( 'NONE',  ( 0.000000000000000000, 0.000000000000000000, 1.000000000000000000 ) ) ;
#27662 = CONTEXT_DEPENDENT_SHAPE_REPRESENTATION ( #22846, #781 ) ;
#27663 = DIRECTION ( 'NONE',  ( -0.000000000000000000, -0.000000000000000000, 1.000000000000000000 ) ) ;
#27664 = DIRECTION ( 'NONE',  ( 0.000000000000000000, 0.000000000000000000, 1.000000000000000000 ) ) ;
#27665 = VERTEX_POINT ( 'NONE', #12958 ) ;
#27666 = DIRECTION ( 'NONE',  ( 0.000000000000000000, 0.000000000000000000, -1.000000000000000000 ) ) ;
#27667 = DIRECTION ( 'NONE',  ( 0.000000000000000000, 0.000000000000000000, 1.000000000000000000 ) ) ;
#27668 = VERTEX_POINT ( 'NONE', #21773 ) ;
#27669 = CARTESIAN_POINT ( 'NONE',  ( 19.99999662536857770, 86.60254037844397601, 12.50000000000000000 ) ) ;
#27670 = CARTESIAN_POINT ( 'NONE',  ( 72.77422209630367433, 61.06482292022032965, 12.49999999999999822 ) ) ;
#27671 = DIRECTION ( 'NONE',  ( 0.000000000000000000, 0.000000000000000000, 1.000000000000000000 ) ) ;
#27672 = EDGE_CURVE ( 'NONE', #1110, #17463, #5660, .T. ) ;
#27673 = ORIENTED_EDGE ( 'NONE', *, *, #13793, .F. ) ;
#27674 = VERTEX_POINT ( 'NONE', #24043 ) ;
#27675 = DIRECTION ( 'NONE',  ( 0.000000000000000000, 0.000000000000000000, 1.000000000000000000 ) ) ;
#27676 = DIRECTION ( 'NONE',  ( 0.000000000000000000, 0.000000000000000000, 1.000000000000000000 ) ) ;
#27677 = ADVANCED_FACE ( 'NONE', ( #12761 ), #8746, .T. ) ;
#27678 = LINE ( 'NONE', #19261, #36286 ) ;
#27679 = ORIENTED_EDGE ( 'NONE', *, *, #10131, .F. ) ;
#27680 = EDGE_LOOP ( 'NONE', ( #5906, #7346, #36058, #19231, #9054, #35352, #16197, #4529, #15721, #7105, #18739, #27417, #18647, #26464, #18170, #21422 ) ) ;
#27681 = AXIS2_PLACEMENT_3D ( 'NONE', #31309, #28146, #2633 ) ;
#27682 = EDGE_CURVE ( 'NONE', #14395, #24629, #27597, .T. ) ;
#27683 = DIRECTION ( 'NONE',  ( 0.000000000000000000, 0.000000000000000000, -1.000000000000000000 ) ) ;
#27684 = DIRECTION ( 'NONE',  ( 0.000000000000000000, 0.000000000000000000, -1.000000000000000000 ) ) ;
#27685 = CARTESIAN_POINT ( 'NONE',  ( -47.63139720814438505, -27.49999999999955591, 5.000000000000000888 ) ) ;
#27686 = CARTESIAN_POINT ( 'NONE',  ( -85.18031014763894859, 72.40127513648181434, 32.50000000000000000 ) ) ;
#27687 = ORIENTED_EDGE ( 'NONE', *, *, #25440, .T. ) ;
#27688 = ORIENTED_EDGE ( 'NONE', *, *, #29017, .F. ) ;
#27689 = DIRECTION ( 'NONE',  ( 0.000000000000000000, 0.000000000000000000, 1.000000000000000000 ) ) ;
#27690 = CARTESIAN_POINT ( 'NONE',  ( -34.00000000000027711, -58.88972745734168512, -49.22241343995298024 ) ) ;
#27691 = ORIENTED_EDGE ( 'NONE', *, *, #30353, .T. ) ;
#27692 = FACE_OUTER_BOUND ( 'NONE', #11125, .T. ) ;
#27693 = VERTEX_POINT ( 'NONE', #18613 ) ;
#27694 = DIRECTION ( 'NONE',  ( 0.000000000000000000, 0.000000000000000000, 1.000000000000000000 ) ) ;
#27695 = AXIS2_PLACEMENT_3D ( 'NONE', #32867, #13340, #6986 ) ;
#27696 = ADVANCED_FACE ( 'NONE', ( #16172, #1907 ), #24419, .T. ) ;
#27697 = DIRECTION ( 'NONE',  ( 1.000000000000000000, 0.000000000000000000, 0.000000000000000000 ) ) ;
#27698 = FACE_OUTER_BOUND ( 'NONE', #34947, .T. ) ;
#27699 = ORIENTED_EDGE ( 'NONE', *, *, #20218, .T. ) ;
#27700 = CYLINDRICAL_SURFACE ( 'NONE', #27830, 2.000000000000000000 ) ;
#27701 = CIRCLE ( 'NONE', #25919, 2.000000000000001776 ) ;
#27702 = DIRECTION ( 'NONE',  ( 1.000000000000000000, 0.000000000000000000, 0.000000000000000000 ) ) ;
#27703 = LINE ( 'NONE', #2021, #14310 ) ;
#27704 = ORIENTED_EDGE ( 'NONE', *, *, #11756, .F. ) ;
#27705 = CIRCLE ( 'NONE', #36105, 2.000000000000001776 ) ;
#27706 = DIRECTION ( 'NONE',  ( -0.000000000000000000, -0.000000000000000000, 1.000000000000000000 ) ) ;
#27707 = CARTESIAN_POINT ( 'NONE',  ( -70.00000337463102085, -34.64101615137762025, -9.999999999999998224 ) ) ;
#27708 = DIRECTION ( 'NONE',  ( 1.000000000000000000, 0.000000000000000000, 0.000000000000000000 ) ) ;
#27709 = EDGE_LOOP ( 'NONE', ( #21159, #5721, #11863, #2415 ) ) ;
#27710 = ORIENTED_EDGE ( 'NONE', *, *, #8262, .T. ) ;
#27711 = EDGE_CURVE ( 'NONE', #33896, #10442, #8656, .T. ) ;
#27712 = ORIENTED_EDGE ( 'NONE', *, *, #1998, .F. ) ;
#27713 = CARTESIAN_POINT ( 'NONE',  ( 59.99999662536842493, -51.96152422706639840, -9.999999999999998224 ) ) ;
#27714 = EDGE_CURVE ( 'NONE', #26973, #3118, #20699, .T. ) ;
#27715 = ORIENTED_EDGE ( 'NONE', *, *, #5291, .F. ) ;
#27716 = FACE_OUTER_BOUND ( 'NONE', #34684, .T. ) ;
#27717 = CARTESIAN_POINT ( 'NONE',  ( -75.00000337463097821, 43.30127018922197379, 12.50000000000000000 ) ) ;
#27718 = EDGE_CURVE ( 'NONE', #31778, #12006, #15237, .T. ) ;
#27719 = CIRCLE ( 'NONE', #20511, 2.000000000000001776 ) ;
#27720 = CARTESIAN_POINT ( 'NONE',  ( -7.041719095097282852E-16, 78.41276890242659192, 32.52035392823930948 ) ) ;
#27721 = DIRECTION ( 'NONE',  ( 0.000000000000000000, 0.000000000000000000, 1.000000000000000000 ) ) ;
#27722 = FACE_OUTER_BOUND ( 'NONE', #1002, .T. ) ;
#27723 = CARTESIAN_POINT ( 'NONE',  ( -79.75043533441352395, -72.37696440020876310, 32.50000000000000000 ) ) ;
#27724 = ADVANCED_FACE ( 'NONE', ( #21606 ), #27408, .F. ) ;
#27725 = DIRECTION ( 'NONE',  ( 0.000000000000000000, 0.000000000000000000, 1.000000000000000000 ) ) ;
#27726 = EDGE_CURVE ( 'NONE', #36242, #27228, #19714, .T. ) ;
#27727 = CARTESIAN_POINT ( 'NONE',  ( -28.00000337463119493, -69.28203230275522628, -9.999999999999998224 ) ) ;
#27728 = EDGE_LOOP ( 'NONE', ( #9373, #2256, #3893, #17402 ) ) ;
#27729 = ORIENTED_EDGE ( 'NONE', *, *, #3313, .T. ) ;
#27730 = CARTESIAN_POINT ( 'NONE',  ( -106.7731239591675205, 98.28784258493143966, 32.55002500000000509 ) ) ;
#27731 = VECTOR ( 'NONE', #33075, 1000.000000000000000 ) ;
#27732 = CARTESIAN_POINT ( 'NONE',  ( 62.99999662536842493, 43.30127018922200222, -5.000000000000000000 ) ) ;
#27733 = DIRECTION ( 'NONE',  ( 1.000000000000000000, 0.000000000000000000, 0.000000000000000000 ) ) ;
#27734 = LINE ( 'NONE', #33579, #5930 ) ;
#27735 = VERTEX_POINT ( 'NONE', #31312 ) ;
#27736 = EDGE_CURVE ( 'NONE', #20758, #27194, #8458, .T. ) ;
#27737 = EDGE_CURVE ( 'NONE', #35393, #12539, #951, .T. ) ;
#27738 = DIRECTION ( 'NONE',  ( 0.000000000000000000, 0.000000000000000000, -1.000000000000000000 ) ) ;
#27739 = EDGE_CURVE ( 'NONE', #4855, #32911, #24977, .T. ) ;
#27740 = DIRECTION ( 'NONE',  ( 0.000000000000000000, 0.000000000000000000, 1.000000000000000000 ) ) ;
#27741 = ORIENTED_EDGE ( 'NONE', *, *, #1514, .T. ) ;
#27742 = CYLINDRICAL_SURFACE ( 'NONE', #3877, 3.000000000000002665 ) ;
#27743 = AXIS2_PLACEMENT_3D ( 'NONE', #37027, #8882, #431 ) ;
#27744 = EDGE_LOOP ( 'NONE', ( #10227, #11773, #18540, #29982, #18181, #22178 ) ) ;
#27745 = CARTESIAN_POINT ( 'NONE',  ( 4.279621169095998212, -62.97617850287780072, 12.49999999999999822 ) ) ;
#27746 = AXIS2_PLACEMENT_3D ( 'NONE', #14032, #36739, #8248 ) ;
#27747 = PLANE ( 'NONE',  #11597 ) ;
#27748 = DIRECTION ( 'NONE',  ( 0.000000000000000000, -0.8660254037844418162, 0.4999999999999945044 ) ) ;
#27749 = ORIENTED_EDGE ( 'NONE', *, *, #7731, .F. ) ;
#27750 = ORIENTED_EDGE ( 'NONE', *, *, #32164, .F. ) ;
#27751 = CIRCLE ( 'NONE', #24176, 3.000000000000007550 ) ;
#27752 = ADVANCED_FACE ( 'NONE', ( #28149 ), #8627, .F. ) ;
#27753 = ORIENTED_EDGE ( 'NONE', *, *, #30580, .T. ) ;
#27754 = LINE ( 'NONE', #27949, #8790 ) ;
#27755 = AXIS2_PLACEMENT_3D ( 'NONE', #10937, #22377, #13210 ) ;
#27756 = DIRECTION ( 'NONE',  ( -1.000000000000000000, 0.000000000000000000, 0.000000000000000000 ) ) ;
#27757 = EDGE_CURVE ( 'NONE', #25195, #4245, #2752, .T. ) ;
#27758 = CARTESIAN_POINT ( 'NONE',  ( 0.000000000000000000, 0.000000000000000000, -5.000000000000000000 ) ) ;
#27759 = CARTESIAN_POINT ( 'NONE',  ( 0.000000000000000000, 0.000000000000000000, 13.31572692736085095 ) ) ;
#27760 = CYLINDRICAL_SURFACE ( 'NONE', #345, 3.000000000000000888 ) ;
#27761 = ORIENTED_EDGE ( 'NONE', *, *, #12008, .F. ) ;
#27762 = CIRCLE ( 'NONE', #22986, 2.000000000000001776 ) ;
#27763 = DIRECTION ( 'NONE',  ( 1.000000000000000000, 0.000000000000000000, 0.000000000000000000 ) ) ;
#27764 = CARTESIAN_POINT ( 'NONE',  ( 68.00000000000000000, 0.000000000000000000, 12.49999999999999822 ) ) ;
#27765 = FACE_OUTER_BOUND ( 'NONE', #7261, .T. ) ;
#27766 = ORIENTED_EDGE ( 'NONE', *, *, #21797, .T. ) ;
#27767 = DIRECTION ( 'NONE',  ( 1.000000000000000000, 0.000000000000000000, 0.000000000000000000 ) ) ;
#27768 = EDGE_CURVE ( 'NONE', #23390, #16038, #30762, .T. ) ;
#27769 = CARTESIAN_POINT ( 'NONE',  ( -22.00000337463124112, -86.60254037844400443, -9.999999999999998224 ) ) ;
#27770 = ORIENTED_EDGE ( 'NONE', *, *, #19979, .F. ) ;
#27771 = AXIS2_PLACEMENT_3D ( 'NONE', #26401, #9320, #3880 ) ;
#27772 = ORIENTED_EDGE ( 'NONE', *, *, #26377, .T. ) ;
#27773 = DIRECTION ( 'NONE',  ( 3.491481338843133355E-15, 1.000000000000000000, 0.000000000000000000 ) ) ;
#27774 = CARTESIAN_POINT ( 'NONE',  ( -80.00000337463094979, -17.32050807568882078, 17.49999999999999645 ) ) ;
#27775 = DIRECTION ( 'NONE',  ( 1.000000000000000000, 0.000000000000000000, 0.000000000000000000 ) ) ;
#27776 = CARTESIAN_POINT ( 'NONE',  ( -1.432312439535614379, -4.946556719366762778, -0.1121614189353595248 ) ) ;
#27777 = ORIENTED_EDGE ( 'NONE', *, *, #4607, .T. ) ;
#27778 = ORIENTED_EDGE ( 'NONE', *, *, #22872, .F. ) ;
#27779 = ADVANCED_FACE ( 'NONE', ( #25172 ), #17069, .T. ) ;
#27780 = AXIS2_PLACEMENT_3D ( 'NONE', #27015, #24601, #27584 ) ;
#27781 = EDGE_CURVE ( 'NONE', #26973, #12879, #10721, .T. ) ;
#27782 = DIRECTION ( 'NONE',  ( 0.000000000000000000, 0.000000000000000000, 1.000000000000000000 ) ) ;
#27783 = EDGE_CURVE ( 'NONE', #31670, #18483, #36963, .T. ) ;
#27784 = AXIS2_PLACEMENT_3D ( 'NONE', #10895, #10177, #24980 ) ;
#27785 = VERTEX_POINT ( 'NONE', #22889 ) ;
#27786 = EDGE_CURVE ( 'NONE', #20315, #25777, #33198, .T. ) ;
#27787 = DIRECTION ( 'NONE',  ( 1.000000000000000000, 0.000000000000000000, 0.000000000000000000 ) ) ;
#27788 = EDGE_LOOP ( 'NONE', ( #14186, #30862, #36588, #28215 ) ) ;
#27789 = ORIENTED_EDGE ( 'NONE', *, *, #600, .T. ) ;
#27790 = LINE ( 'NONE', #24070, #26789 ) ;
#27791 = FACE_OUTER_BOUND ( 'NONE', #29236, .T. ) ;
#27792 = ORIENTED_EDGE ( 'NONE', *, *, #10995, .F. ) ;
#27793 = VERTEX_POINT ( 'NONE', #5466 ) ;
#27794 = DIRECTION ( 'NONE',  ( 1.000000000000000000, 0.000000000000000000, 0.000000000000000000 ) ) ;
#27795 = FACE_OUTER_BOUND ( 'NONE', #28068, .T. ) ;
#27796 = DIRECTION ( 'NONE',  ( 0.000000000000000000, 0.000000000000000000, 1.000000000000000000 ) ) ;
#27797 = DIRECTION ( 'NONE',  ( 0.000000000000000000, 0.000000000000000000, 1.000000000000000000 ) ) ;
#27798 = AXIS2_PLACEMENT_3D ( 'NONE', #5943, #2946, #9100 ) ;
#27799 = ORIENTED_EDGE ( 'NONE', *, *, #18999, .F. ) ;
#27800 = DIRECTION ( 'NONE',  ( -0.000000000000000000, -0.000000000000000000, 1.000000000000000000 ) ) ;
#27801 = FACE_BOUND ( 'NONE', #16638, .T. ) ;
#27802 = DIRECTION ( 'NONE',  ( 0.000000000000000000, 0.000000000000000000, -1.000000000000000000 ) ) ;
#27803 = FACE_BOUND ( 'NONE', #22322, .T. ) ;
#27804 = DIRECTION ( 'NONE',  ( 0.000000000000000000, 0.000000000000000000, -1.000000000000000000 ) ) ;
#27805 = ADVANCED_FACE ( 'NONE', ( #34325 ), #4911, .F. ) ;
#27806 = DIRECTION ( 'NONE',  ( 1.000000000000000000, 0.000000000000000000, 0.000000000000000000 ) ) ;
#27807 = AXIS2_PLACEMENT_3D ( 'NONE', #14989, #26417, #23597 ) ;
#27808 = CARTESIAN_POINT ( 'NONE',  ( 0.000000000000000000, 0.000000000000000000, 32.50000000000000000 ) ) ;
#27809 = AXIS2_PLACEMENT_3D ( 'NONE', #35826, #16135, #18577 ) ;
#27810 = CARTESIAN_POINT ( 'NONE',  ( -17.00000337463126243, 77.94228634059957983, -9.999999999999998224 ) ) ;
#27811 = ORIENTED_EDGE ( 'NONE', *, *, #9640, .T. ) ;
#27812 = DIRECTION ( 'NONE',  ( 0.000000000000000000, 0.000000000000000000, -1.000000000000000000 ) ) ;
#27813 = CARTESIAN_POINT ( 'NONE',  ( -5.000000000000000000, -2.426004080355352421, -0.4213009713786332044 ) ) ;
#27814 = CARTESIAN_POINT ( 'NONE',  ( -60.00000337463104216, 34.64101615137757051, -5.000000000000000000 ) ) ;
#27815 = VERTEX_POINT ( 'NONE', #16893 ) ;
#27816 = ORIENTED_EDGE ( 'NONE', *, *, #14392, .F. ) ;
#27817 = ORIENTED_EDGE ( 'NONE', *, *, #34282, .T. ) ;
#27818 = DIRECTION ( 'NONE',  ( 0.000000000000000000, 0.000000000000000000, 1.000000000000000000 ) ) ;
#27819 = CYLINDRICAL_SURFACE ( 'NONE', #166, 2.000000000000001776 ) ;
#27820 = AXIS2_PLACEMENT_3D ( 'NONE', #29788, #26602, #33681 ) ;
#27821 = VERTEX_POINT ( 'NONE', #16724 ) ;
#27822 = CIRCLE ( 'NONE', #11645, 2.000000000000000000 ) ;
#27823 = CARTESIAN_POINT ( 'NONE',  ( -43.00000337463112743, -60.62177826491080168, -9.999999999999998224 ) ) ;
#27824 = CARTESIAN_POINT ( 'NONE',  ( -50.00000337463109190, 51.96152422706637708, -9.999999999999998224 ) ) ;
#27825 = EDGE_LOOP ( 'NONE', ( #35631, #30940, #32662, #14451 ) ) ;
#27826 = EDGE_CURVE ( 'NONE', #33506, #29268, #2157, .T. ) ;
#27827 = CARTESIAN_POINT ( 'NONE',  ( 80.69570903995992239, -15.44541228182035475, 12.50000000000000000 ) ) ;
#27828 = ORIENTED_EDGE ( 'NONE', *, *, #35813, .T. ) ;
#27829 = CARTESIAN_POINT ( 'NONE',  ( -68.00000337463099243, -2.428612866367529932E-14, -5.000000000000000000 ) ) ;
#27830 = AXIS2_PLACEMENT_3D ( 'NONE', #34272, #4857, #19286 ) ;
#27831 = VECTOR ( 'NONE', #13356, 1000.000000000000000 ) ;
#27832 = AXIS2_PLACEMENT_3D ( 'NONE', #31413, #22427, #14546 ) ;
#27833 = CARTESIAN_POINT ( 'NONE',  ( 67.99999662536836809, -51.96152422706639840, -9.999999999999998224 ) ) ;
#27834 = DIRECTION ( 'NONE',  ( 1.000000000000000000, 0.000000000000000000, 0.000000000000000000 ) ) ;
#27835 = ORIENTED_EDGE ( 'NONE', *, *, #36424, .T. ) ;
#27836 = DIRECTION ( 'NONE',  ( 0.000000000000000000, 0.000000000000000000, 1.000000000000000000 ) ) ;
#27837 = CARTESIAN_POINT ( 'NONE',  ( -50.00000337463109190, 69.28203230275518365, -5.000000000000000000 ) ) ;
#27838 = CARTESIAN_POINT ( 'NONE',  ( 5.000000000000000000, 25.00000000000000000, 15.00000000000000000 ) ) ;
#27839 = CIRCLE ( 'NONE', #25471, 3.000000000000002665 ) ;
#27840 = ORIENTED_EDGE ( 'NONE', *, *, #12258, .T. ) ;
#27841 = CARTESIAN_POINT ( 'NONE',  ( 71.99999662536838230, -34.64101615137759183, 12.50000000000000000 ) ) ;
#27842 = DIRECTION ( 'NONE',  ( 0.000000000000000000, 0.000000000000000000, 1.000000000000000000 ) ) ;
#27843 = ORIENTED_EDGE ( 'NONE', *, *, #8807, .F. ) ;
#27844 = CARTESIAN_POINT ( 'NONE',  ( 51.13139720814417899, 27.49999999999988987, -5.000000000000000000 ) ) ;
#27845 = AXIS2_PLACEMENT_3D ( 'NONE', #2124, #13371, #32900 ) ;
#27846 = DIRECTION ( 'NONE',  ( -1.000000000000000000, 0.000000000000000000, 0.000000000000000000 ) ) ;
#27847 = DIRECTION ( 'NONE',  ( 0.000000000000000000, 0.000000000000000000, 1.000000000000000000 ) ) ;
#27848 = EDGE_CURVE ( 'NONE', #20167, #8353, #26701, .T. ) ;
#27849 = CIRCLE ( 'NONE', #26647, 2.000000000000001776 ) ;
#27850 = AXIS2_PLACEMENT_3D ( 'NONE', #16689, #36737, #17031 ) ;
#27851 = VERTEX_POINT ( 'NONE', #28314 ) ;
#27852 = ORIENTED_EDGE ( 'NONE', *, *, #17633, .T. ) ;
#27853 = EDGE_CURVE ( 'NONE', #8974, #5583, #33291, .T. ) ;
#27854 = CARTESIAN_POINT ( 'NONE',  ( 66.99999662536839651, 60.62177826491078747, 12.50000000000000000 ) ) ;
#27855 = VECTOR ( 'NONE', #3293, 1000.000000000000000 ) ;
#27856 = CARTESIAN_POINT ( 'NONE',  ( 46.99999662536849598, -77.94228634059960825, -9.999999999999998224 ) ) ;
#27857 = VECTOR ( 'NONE', #8167, 1000.000000000000000 ) ;
#27858 = CIRCLE ( 'NONE', #4538, 3.000000000000005773 ) ;
#27859 = CARTESIAN_POINT ( 'NONE',  ( -72.00000337463102085, -51.96152422706641971, 12.50000000000000000 ) ) ;
#27861 = ORIENTED_EDGE ( 'NONE', *, *, #33845, .F. ) ;
#27860 = EDGE_CURVE ( 'NONE', #13060, #19610, #36298, .T. ) ;
#27862 = ORIENTED_EDGE ( 'NONE', *, *, #24288, .T. ) ;
#27863 = CARTESIAN_POINT ( 'NONE',  ( 76.99999662536836809, 8.660254037844394404, -9.999999999999998224 ) ) ;
#27864 = CARTESIAN_POINT ( 'NONE',  ( -3.675296855064184687, 3.651569063273166993, -0.8655517945778067324 ) ) ;
#27865 = CARTESIAN_POINT ( 'NONE',  ( 62.99999662536842493, 43.30127018922200222, -9.999999999999998224 ) ) ;
#27866 = CARTESIAN_POINT ( 'NONE',  ( 3.000000000000000000, -1.467624384280032501, -2.541999999999998483 ) ) ;
#27867 = ORIENTED_EDGE ( 'NONE', *, *, #18213, .T. ) ;
#27868 = ORIENTED_EDGE ( 'NONE', *, *, #33728, .T. ) ;
#27869 = CARTESIAN_POINT ( 'NONE',  ( 58.88972745734179171, -34.00000000000007105, 12.49999999999999822 ) ) ;
#27870 = AXIS2_PLACEMENT_3D ( 'NONE', #36113, #27661, #15864 ) ;
#27871 = DIRECTION ( 'NONE',  ( 0.000000000000000000, 0.000000000000000000, 1.000000000000000000 ) ) ;
#27872 = ORIENTED_EDGE ( 'NONE', *, *, #31138, .T. ) ;
#27873 = EDGE_CURVE ( 'NONE', #34867, #24850, #3862, .T. ) ;
#27874 = CIRCLE ( 'NONE', #29035, 2.000000000000001776 ) ;
#27875 = FACE_BOUND ( 'NONE', #30421, .T. ) ;
#27876 = ORIENTED_EDGE ( 'NONE', *, *, #25192, .T. ) ;
#27877 = CARTESIAN_POINT ( 'NONE',  ( -77.00000337463100664, -43.30127018922202353, -9.999999999999998224 ) ) ;
#27878 = AXIS2_PLACEMENT_3D ( 'NONE', #2238, #2794, #8039 ) ;
#27879 = AXIS2_PLACEMENT_3D ( 'NONE', #1743, #33619, #36615 ) ;
#27880 = AXIS2_PLACEMENT_3D ( 'NONE', #9496, #29360, #24283 ) ;
#27881 = AXIS2_PLACEMENT_3D ( 'NONE', #16640, #10991, #5396 ) ;
#27882 = DIRECTION ( 'NONE',  ( 1.000000000000000000, 0.000000000000000000, 0.000000000000000000 ) ) ;
#27883 = DIRECTION ( 'NONE',  ( 0.000000000000000000, 0.000000000000000000, 1.000000000000000000 ) ) ;
#27884 = ORIENTED_EDGE ( 'NONE', *, *, #6435, .F. ) ;
#27885 =( NAMED_UNIT ( * ) SI_UNIT ( $, .STERADIAN. ) SOLID_ANGLE_UNIT ( ) );
#27886 = EDGE_CURVE ( 'NONE', #24245, #28829, #13440, .T. ) ;
#27887 = CIRCLE ( 'NONE', #11135, 3.499999999999989342 ) ;
#27888 = CYLINDRICAL_SURFACE ( 'NONE', #10469, 2.000000000000001776 ) ;
#27889 = DIRECTION ( 'NONE',  ( 0.000000000000000000, 0.000000000000000000, 1.000000000000000000 ) ) ;
#27890 = DIRECTION ( 'NONE',  ( 0.000000000000000000, 0.000000000000000000, 1.000000000000000000 ) ) ;
#27891 = EDGE_CURVE ( 'NONE', #24391, #34954, #3377, .T. ) ;
#27892 = EDGE_LOOP ( 'NONE', ( #4206, #7600 ) ) ;
#27893 = DIRECTION ( 'NONE',  ( 1.000000000000000000, 0.000000000000000000, 0.000000000000000000 ) ) ;
#27894 = CARTESIAN_POINT ( 'NONE',  ( 9.999996625368625658, 86.60254037844397601, -5.000000000000000000 ) ) ;
#27895 = DIRECTION ( 'NONE',  ( 0.000000000000000000, 0.000000000000000000, 1.000000000000000000 ) ) ;
#27896 = AXIS2_PLACEMENT_3D ( 'NONE', #17700, #14903, #23521 ) ;
#27897 = ADVANCED_FACE ( 'NONE', ( #924 ), #25881, .F. ) ;
#27898 = ORIENTED_EDGE ( 'NONE', *, *, #2290, .F. ) ;
#27899 = ORIENTED_EDGE ( 'NONE', *, *, #3281, .T. ) ;
#27900 = AXIS2_PLACEMENT_3D ( 'NONE', #34018, #16573, #13930 ) ;
#27901 = CYLINDRICAL_SURFACE ( 'NONE', #27497, 2.000000000000001776 ) ;
#27902 = EDGE_LOOP ( 'NONE', ( #4247, #8560, #3870, #32575, #1742, #16250 ) ) ;
#27903 = AXIS2_PLACEMENT_3D ( 'NONE', #30028, #4349, #7347 ) ;
#27904 = ADVANCED_FACE ( 'NONE', ( #11607 ), #14119, .T. ) ;
#27905 = DIRECTION ( 'NONE',  ( -0.000000000000000000, -0.000000000000000000, -1.000000000000000000 ) ) ;
#27906 = DIRECTION ( 'NONE',  ( 0.000000000000000000, 0.000000000000000000, 1.000000000000000000 ) ) ;
#27907 = AXIS2_PLACEMENT_3D ( 'NONE', #21388, #29822, #24024 ) ;
#27908 = VECTOR ( 'NONE', #11821, 1000.000000000000000 ) ;
#27909 = VECTOR ( 'NONE', #2132, 1000.000000000000000 ) ;
#27910 = CARTESIAN_POINT ( 'NONE',  ( -124.4080600076932370, -12.15049814296501829, 27.50000000000000000 ) ) ;
#27911 = VECTOR ( 'NONE', #26007, 1000.000000000000000 ) ;
#27912 = EDGE_CURVE ( 'NONE', #26861, #12924, #34419, .T. ) ;
#27913 = LINE ( 'NONE', #21566, #30191 ) ;
#27914 = CYLINDRICAL_SURFACE ( 'NONE', #31646, 3.499999999999996003 ) ;
#27915 = PLANE ( 'NONE',  #6025 ) ;
#27916 = CARTESIAN_POINT ( 'NONE',  ( -70.00000337463102085, -34.64101615137762025, 17.49999999999999645 ) ) ;
#27917 = CARTESIAN_POINT ( 'NONE',  ( -83.00000337463092137, -25.98076211353322051, 12.50000000000000000 ) ) ;
#27918 = ORIENTED_EDGE ( 'NONE', *, *, #26163, .F. ) ;
#27919 = AXIS2_PLACEMENT_3D ( 'NONE', #28931, #23690, #3258 ) ;
#27920 = ORIENTED_EDGE ( 'NONE', *, *, #998, .T. ) ;
#27921 = CARTESIAN_POINT ( 'NONE',  ( 0.000000000000000000, -1.467624384280027172, 2.542000000000001592 ) ) ;
#27922 = DIRECTION ( 'NONE',  ( 0.000000000000000000, 0.000000000000000000, -1.000000000000000000 ) ) ;
#27923 = DIRECTION ( 'NONE',  ( 1.000000000000000000, 0.000000000000000000, 0.000000000000000000 ) ) ;
#27924 = DIRECTION ( 'NONE',  ( 0.000000000000000000, 0.000000000000000000, 1.000000000000000000 ) ) ;
#27925 = ORIENTED_EDGE ( 'NONE', *, *, #1776, .F. ) ;
#27926 = AXIS2_PLACEMENT_3D ( 'NONE', #34200, #11479, #8325 ) ;
#27927 = EDGE_CURVE ( 'NONE', #36735, #29715, #3186, .T. ) ;
#27928 = CIRCLE ( 'NONE', #33909, 2.000000000000001776 ) ;
#27929 = DIRECTION ( 'NONE',  ( 1.000000000000000000, 0.000000000000000000, 0.000000000000000000 ) ) ;
#27930 = VERTEX_POINT ( 'NONE', #14616 ) ;
#27931 = ORIENTED_EDGE ( 'NONE', *, *, #4989, .T. ) ;
#27932 = PRESENTATION_LAYER_ASSIGNMENT (  '', '', ( #21944 ) ) ;
#27933 = DIRECTION ( 'NONE',  ( -1.000000000000000000, 0.000000000000000000, 0.000000000000000000 ) ) ;
#27934 = ORIENTED_EDGE ( 'NONE', *, *, #36392, .T. ) ;
#27935 = AXIS2_PLACEMENT_3D ( 'NONE', #10560, #16759, #13195 ) ;
#27936 = CIRCLE ( 'NONE', #11755, 2.000000000000001776 ) ;
#27937 = DIRECTION ( 'NONE',  ( -1.000000000000000000, -0.000000000000000000, -0.000000000000000000 ) ) ;
#27938 = ADVANCED_FACE ( 'NONE', ( #9171 ), #32029, .F. ) ;
#27939 = CIRCLE ( 'NONE', #4589, 2.000000000000000000 ) ;
#27940 = DIRECTION ( 'NONE',  ( -1.000000000000000000, 0.000000000000000000, 0.000000000000000000 ) ) ;
#27941 = CIRCLE ( 'NONE', #25569, 2.000000000000000000 ) ;
#27942 = DIRECTION ( 'NONE',  ( -1.000000000000000000, 1.130782710266362465E-14, 0.000000000000000000 ) ) ;
#27943 = EDGE_CURVE ( 'NONE', #3582, #23793, #18263, .T. ) ;
#27944 = ORIENTED_EDGE ( 'NONE', *, *, #20159, .F. ) ;
#27945 = ORIENTED_EDGE ( 'NONE', *, *, #27711, .T. ) ;
#27946 = VERTEX_POINT ( 'NONE', #17609 ) ;
#27947 = VECTOR ( 'NONE', #12005, 1000.000000000000000 ) ;
#27948 = ORIENTED_EDGE ( 'NONE', *, *, #27826, .F. ) ;
#27949 = CARTESIAN_POINT ( 'NONE',  ( 2.094888803305880329E-14, 6.000000000000000000, 32.50000000000000000 ) ) ;
#27950 = CARTESIAN_POINT ( 'NONE',  ( -87.00000337463093558, 25.98076211353317433, -9.999999999999998224 ) ) ;
#27951 = CARTESIAN_POINT ( 'NONE',  ( -68.00000337463102085, -51.96152422706641971, -9.999999999999998224 ) ) ;
#27952 = DIRECTION ( 'NONE',  ( 0.000000000000000000, 0.000000000000000000, -1.000000000000000000 ) ) ;
#27953 = CARTESIAN_POINT ( 'NONE',  ( 4.999999999999999112, -1.069697119166215682, -3.973125653578879035 ) ) ;
#27954 = EDGE_LOOP ( 'NONE', ( #23626, #29706 ) ) ;
#27955 = DIRECTION ( 'NONE',  ( 1.000000000000000000, 0.000000000000000000, 0.000000000000000000 ) ) ;
#27956 = VECTOR ( 'NONE', #10331, 1000.000000000000000 ) ;
#27957 = CARTESIAN_POINT ( 'NONE',  ( -3.374631327851540519E-06, 86.60254037844397601, -9.999999999999998224 ) ) ;
#27958 = ADVANCED_FACE ( 'NONE', ( #6369 ), #17809, .F. ) ;
#27959 = CIRCLE ( 'NONE', #30921, 2.000000000000000000 ) ;
#27960 = CIRCLE ( 'NONE', #29161, 33.00000000000001421 ) ;
#27961 = ORIENTED_EDGE ( 'NONE', *, *, #18112, .T. ) ;
#27962 = FACE_OUTER_BOUND ( 'NONE', #1693, .T. ) ;
#27963 = LINE ( 'NONE', #31318, #34533 ) ;
#27964 = AXIS2_PLACEMENT_3D ( 'NONE', #13598, #16603, #17152 ) ;
#27965 = ORIENTED_EDGE ( 'NONE', *, *, #28873, .T. ) ;
#27966 = CIRCLE ( 'NONE', #32756, 2.000000000000001776 ) ;
#27967 = VERTEX_POINT ( 'NONE', #26433 ) ;
#27968 = AXIS2_PLACEMENT_3D ( 'NONE', #16024, #33256, #22203 ) ;
#27969 = DIRECTION ( 'NONE',  ( -0.5000000000000101030, -0.8660254037844328234, 0.000000000000000000 ) ) ;
#27970 = CYLINDRICAL_SURFACE ( 'NONE', #6128, 1.999999999999998224 ) ;
#27971 = CARTESIAN_POINT ( 'NONE',  ( -0.03111943836865636165, -6.084399642271208997, -4.366192694417998510 ) ) ;
#27972 = CARTESIAN_POINT ( 'NONE',  ( -101.8947384033993018, -31.99217250720169758, 32.50000000000000000 ) ) ;
#27973 = ORIENTED_EDGE ( 'NONE', *, *, #6713, .T. ) ;
#27974 = ORIENTED_EDGE ( 'NONE', *, *, #2949, .F. ) ;
#27975 = CIRCLE ( 'NONE', #36395, 2.000000000000000000 ) ;
#27976 = AXIS2_PLACEMENT_3D ( 'NONE', #16750, #7749, #22540 ) ;
#27977 = CARTESIAN_POINT ( 'NONE',  ( 19.99999662536857770, 86.60254037844397601, -5.000000000000000000 ) ) ;
#27978 = EDGE_CURVE ( 'NONE', #8893, #29771, #9368, .T. ) ;
#27979 = ORIENTED_EDGE ( 'NONE', *, *, #5240, .F. ) ;
#27980 = EDGE_CURVE ( 'NONE', #9828, #19877, #15007, .T. ) ;
#27981 = AXIS2_PLACEMENT_3D ( 'NONE', #33255, #16570, #1940 ) ;
#27982 = DIRECTION ( 'NONE',  ( 0.7071067811865489050, 0.7071067811865461294, -0.000000000000000000 ) ) ;
#27983 = VERTEX_POINT ( 'NONE', #20260 ) ;
#27984 = ORIENTED_EDGE ( 'NONE', *, *, #23567, .T. ) ;
#27985 = EDGE_CURVE ( 'NONE', #31670, #8095, #2694, .T. ) ;
#27986 = CARTESIAN_POINT ( 'NONE',  ( -72.00000337463100664, -2.404119930384582903E-14, -9.999999999999998224 ) ) ;
#27987 = LINE ( 'NONE', #11470, #10082 ) ;
#27988 = ORIENTED_EDGE ( 'NONE', *, *, #24016, .F. ) ;
#27989 = ORIENTED_EDGE ( 'NONE', *, *, #35094, .T. ) ;
#27990 = EDGE_CURVE ( 'NONE', #34413, #666, #31430, .T. ) ;
#27991 = CARTESIAN_POINT ( 'NONE',  ( -37.50000000000000000, 103.4105893997321743, 18.49999999999999645 ) ) ;
#27992 = FACE_OUTER_BOUND ( 'NONE', #22028, .T. ) ;
#27993 = ADVANCED_FACE ( 'NONE', ( #3743 ), #35272, .T. ) ;
#27994 = STYLED_ITEM ( 'NONE', ( #3353 ), #17512 ) ;
#27995 = FACE_BOUND ( 'NONE', #34536, .T. ) ;
#27996 = DIRECTION ( 'NONE',  ( 0.000000000000000000, 0.000000000000000000, 1.000000000000000000 ) ) ;
#27997 = AXIS2_PLACEMENT_3D ( 'NONE', #19006, #24636, #33057 ) ;
#27998 = EDGE_LOOP ( 'NONE', ( #20579, #17886, #10402, #5829 ) ) ;
#27999 = CARTESIAN_POINT ( 'NONE',  ( -62.97617850287781494, -4.279621169095772615, 12.49999999999999822 ) ) ;
#28000 = FACE_BOUND ( 'NONE', #10804, .T. ) ;
#28001 = CARTESIAN_POINT ( 'NONE',  ( 3.000000000000000000, -1.467624384280027172, 2.542000000000001592 ) ) ;
#28002 = DIRECTION ( 'NONE',  ( -1.000000000000000000, 0.000000000000000000, 0.000000000000000000 ) ) ;
#28003 = CIRCLE ( 'NONE', #17827, 95.00000000000000000 ) ;
#28004 = DIRECTION ( 'NONE',  ( -1.000000000000000000, 0.000000000000000000, -0.000000000000000000 ) ) ;
#28005 = EDGE_CURVE ( 'NONE', #10047, #29027, #2099, .T. ) ;
#28006 = PLANE ( 'NONE',  #5140 ) ;
#28007 = ADVANCED_FACE ( 'NONE', ( #20433 ), #6181, .F. ) ;
#28008 = CARTESIAN_POINT ( 'NONE',  ( -67.00000337463104927, -43.30127018922202353, -9.999999999999998224 ) ) ;
#28009 = ADVANCED_FACE ( 'NONE', ( #5830 ), #6738, .T. ) ;
#28010 = CIRCLE ( 'NONE', #11823, 2.000000000000001776 ) ;
#28011 = EDGE_CURVE ( 'NONE', #20792, #22677, #32603, .T. ) ;
#28012 = CARTESIAN_POINT ( 'NONE',  ( -56.74224907228983028, 68.66839587347264739, -49.22241343995295892 ) ) ;
#28013 = ORIENTED_EDGE ( 'NONE', *, *, #8040, .T. ) ;
#28014 = CARTESIAN_POINT ( 'NONE',  ( -5.000000000000000000, -0.4878135028931876449, -6.000000000000001776 ) ) ;
#28015 = AXIS2_PLACEMENT_3D ( 'NONE', #10888, #27593, #10334 ) ;
#28016 = CYLINDRICAL_SURFACE ( 'NONE', #26707, 2.000000000000001776 ) ;
#28017 = LINE ( 'NONE', #33471, #16348 ) ;
#28018 = AXIS2_PLACEMENT_3D ( 'NONE', #1817, #12674, #18515 ) ;
#28019 = ORIENTED_EDGE ( 'NONE', *, *, #17202, .F. ) ;
#28020 = ORIENTED_EDGE ( 'NONE', *, *, #36729, .T. ) ;
#28021 = ORIENTED_EDGE ( 'NONE', *, *, #1803, .T. ) ;
#28022 = PLANE ( 'NONE',  #20149 ) ;
#28023 = CARTESIAN_POINT ( 'NONE',  ( -65.00000337463102085, 25.98076211353317433, -9.999999999999998224 ) ) ;
#28024 = VERTEX_POINT ( 'NONE', #1126 ) ;
#28025 = VECTOR ( 'NONE', #34002, 1000.000000000000000 ) ;
#28026 = DIRECTION ( 'NONE',  ( 0.000000000000000000, 0.000000000000000000, -1.000000000000000000 ) ) ;
#28027 = DIRECTION ( 'NONE',  ( 1.000000000000000000, 0.000000000000000000, 0.000000000000000000 ) ) ;
#28028 = ORIENTED_EDGE ( 'NONE', *, *, #16249, .T. ) ;
#28029 = DIRECTION ( 'NONE',  ( 0.000000000000000000, 0.000000000000000000, 1.000000000000000000 ) ) ;
#28030 = ORIENTED_EDGE ( 'NONE', *, *, #9403, .F. ) ;
#28031 = DIRECTION ( 'NONE',  ( 1.000000000000000000, 0.000000000000000000, 0.000000000000000000 ) ) ;
#28032 = CIRCLE ( 'NONE', #1102, 2.000000000000001776 ) ;
#28033 = CARTESIAN_POINT ( 'NONE',  ( 68.19171716056558807, -52.81599796988855644, -5.000000000000000000 ) ) ;
#28034 = LINE ( 'NONE', #8703, #4046 ) ;
#28035 = VECTOR ( 'NONE', #12377, 1000.000000000000000 ) ;
#28036 = ORIENTED_EDGE ( 'NONE', *, *, #5531, .T. ) ;
#28037 = LINE ( 'NONE', #16963, #6298 ) ;
#28038 = AXIS2_PLACEMENT_3D ( 'NONE', #28856, #25712, #22711 ) ;
#28039 = AXIS2_PLACEMENT_3D ( 'NONE', #22610, #16424, #34062 ) ;
#28040 = DIRECTION ( 'NONE',  ( -1.000000000000000000, 0.000000000000000000, 0.000000000000000000 ) ) ;
#28041 = DIRECTION ( 'NONE',  ( 1.000000000000000000, 0.000000000000000000, 0.000000000000000000 ) ) ;
#28042 = CIRCLE ( 'NONE', #7683, 65.00000000000000000 ) ;
#28043 = ORIENTED_EDGE ( 'NONE', *, *, #15148, .F. ) ;
#28044 = CARTESIAN_POINT ( 'NONE',  ( 3.000000000000000000, -1.467624384280027172, 2.542000000000001592 ) ) ;
#28045 = DIRECTION ( 'NONE',  ( 0.000000000000000000, 0.000000000000000000, 1.000000000000000000 ) ) ;
#28046 = ORIENTED_EDGE ( 'NONE', *, *, #12860, .F. ) ;
#28047 = CARTESIAN_POINT ( 'NONE',  ( -67.00000337463104927, -25.98076211353322051, -5.000000000000000000 ) ) ;
#28048 = DIRECTION ( 'NONE',  ( 0.000000000000000000, 0.000000000000000000, -1.000000000000000000 ) ) ;
#28049 = CARTESIAN_POINT ( 'NONE',  ( -27.78182860042817026, -56.67878100130359087, 12.49999999999999822 ) ) ;
#28050 = AXIS2_PLACEMENT_3D ( 'NONE', #20618, #24189, #1316 ) ;
#28051 = DIRECTION ( 'NONE',  ( 0.000000000000000000, 0.000000000000000000, 1.000000000000000000 ) ) ;
#28052 = VECTOR ( 'NONE', #35521, 1000.000000000000000 ) ;
#28053 = EDGE_LOOP ( 'NONE', ( #36775, #33523, #26192, #13939, #32306 ) ) ;
#28054 = ADVANCED_FACE ( 'NONE', ( #15740 ), #29799, .F. ) ;
#28055 = EDGE_LOOP ( 'NONE', ( #20028, #34076 ) ) ;
#28056 = DIRECTION ( 'NONE',  ( -0.000000000000000000, -0.000000000000000000, 1.000000000000000000 ) ) ;
#28057 = CIRCLE ( 'NONE', #26263, 2.000000000000001776 ) ;
#28058 = CYLINDRICAL_SURFACE ( 'NONE', #19985, 2.000000000000000000 ) ;
#28059 = CARTESIAN_POINT ( 'NONE',  ( -10.00000337463125000, -86.60254037844400443, -9.999999999999998224 ) ) ;
#28060 = ORIENTED_EDGE ( 'NONE', *, *, #28312, .T. ) ;
#28061 = ORIENTED_EDGE ( 'NONE', *, *, #36460, .T. ) ;
#28062 = CIRCLE ( 'NONE', #2918, 2.000000000000001776 ) ;
#28063 = LINE ( 'NONE', #13820, #24215 ) ;
#28064 = DIRECTION ( 'NONE',  ( 0.000000000000000000, 0.000000000000000000, 1.000000000000000000 ) ) ;
#28065 = AXIS2_PLACEMENT_3D ( 'NONE', #29881, #16203, #21447 ) ;
#28066 = LINE ( 'NONE', #25820, #28420 ) ;
#28067 = ORIENTED_EDGE ( 'NONE', *, *, #25381, .T. ) ;
#28068 = EDGE_LOOP ( 'NONE', ( #32110, #26573, #35347, #28393 ) ) ;
#28069 = DIRECTION ( 'NONE',  ( 0.000000000000000000, 0.000000000000000000, 1.000000000000000000 ) ) ;
#28070 = CIRCLE ( 'NONE', #6502, 33.00000000000001421 ) ;
#28071 = CARTESIAN_POINT ( 'NONE',  ( 14.99999662536863632, -77.94228634059960825, 17.49999999999999645 ) ) ;
#28072 = VERTEX_POINT ( 'NONE', #18171 ) ;
#28073 = AXIS2_PLACEMENT_3D ( 'NONE', #17142, #14682, #23501 ) ;
#28074 = DIRECTION ( 'NONE',  ( 0.000000000000000000, 0.000000000000000000, 1.000000000000000000 ) ) ;
#28075 = ORIENTED_EDGE ( 'NONE', *, *, #34840, .F. ) ;
#28076 = FACE_BOUND ( 'NONE', #33225, .T. ) ;
#28077 = EDGE_CURVE ( 'NONE', #24891, #33006, #24006, .T. ) ;
#28078 = AXIS2_PLACEMENT_3D ( 'NONE', #18145, #9893, #12692 ) ;
#28079 = EDGE_CURVE ( 'NONE', #13800, #68, #6862, .T. ) ;
#28080 = CIRCLE ( 'NONE', #18928, 2.000000000000000000 ) ;
#28081 = AXIS2_PLACEMENT_3D ( 'NONE', #24544, #30694, #10839 ) ;
#28082 = DIRECTION ( 'NONE',  ( 0.000000000000000000, 0.000000000000000000, -1.000000000000000000 ) ) ;
#28083 = ORIENTED_EDGE ( 'NONE', *, *, #7149, .T. ) ;
#28084 = DIRECTION ( 'NONE',  ( 1.387778780781458618E-17, 2.403703357979451689E-17, 1.000000000000000000 ) ) ;
#28085 = CYLINDRICAL_SURFACE ( 'NONE', #35639, 2.000000000000001776 ) ;
#28086 = EDGE_CURVE ( 'NONE', #30390, #26110, #15867, .T. ) ;
#28087 = VECTOR ( 'NONE', #6909, 1000.000000000000000 ) ;
#28088 = DIRECTION ( 'NONE',  ( 1.000000000000000000, 0.000000000000000000, 0.000000000000000000 ) ) ;
#28089 = DIRECTION ( 'NONE',  ( 0.000000000000000000, 0.000000000000000000, 1.000000000000000000 ) ) ;
#28090 = ORIENTED_EDGE ( 'NONE', *, *, #30468, .F. ) ;
#28091 = CARTESIAN_POINT ( 'NONE',  ( 6.249999999999998224, 0.000000000000000000, 3.000000000000000888 ) ) ;
#28092 = AXIS2_PLACEMENT_3D ( 'NONE', #5665, #4934, #13749 ) ;
#28093 = CARTESIAN_POINT ( 'NONE',  ( 4.279621169095998212, -62.97617850287780072, -49.86561046011506448 ) ) ;
#28094 = DIRECTION ( 'NONE',  ( 0.000000000000000000, 0.000000000000000000, -1.000000000000000000 ) ) ;
#28095 = ORIENTED_EDGE ( 'NONE', *, *, #16952, .F. ) ;
#28096 = ORIENTED_EDGE ( 'NONE', *, *, #11129, .F. ) ;
#28097 = VECTOR ( 'NONE', #18670, 1000.000000000000000 ) ;
#28098 = EDGE_CURVE ( 'NONE', #35279, #27267, #14644, .T. ) ;
#28099 = DIRECTION ( 'NONE',  ( 1.000000000000000000, 0.000000000000000000, 0.000000000000000000 ) ) ;
#28100 = ORIENTED_EDGE ( 'NONE', *, *, #6322, .F. ) ;
#28101 = LINE ( 'NONE', #9090, #21125 ) ;
#28102 = CARTESIAN_POINT ( 'NONE',  ( -10.00000337463125000, -86.60254037844400443, 17.49999999999999645 ) ) ;
#28103 = AXIS2_PLACEMENT_3D ( 'NONE', #13436, #5011, #10447 ) ;
#28104 = CARTESIAN_POINT ( 'NONE',  ( 2.500000000000008438, 4.330127018922190096, -2.691222917490924395E-15 ) ) ;
#28105 = CIRCLE ( 'NONE', #5352, 2.000000000000000000 ) ;
#28106 = CARTESIAN_POINT ( 'NONE',  ( -62.97617850287781494, -4.279621169095772615, 12.49999999999999822 ) ) ;
#28107 = AXIS2_PLACEMENT_3D ( 'NONE', #29510, #20704, #29340 ) ;
#28108 = FACE_OUTER_BOUND ( 'NONE', #22078, .T. ) ;
#28109 = DIRECTION ( 'NONE',  ( 1.000000000000000000, 0.000000000000000000, 0.000000000000000000 ) ) ;
#28110 = CARTESIAN_POINT ( 'NONE',  ( -85.00000337463092137, -8.660254037844422825, 17.49999999999999645 ) ) ;
#28111 = CARTESIAN_POINT ( 'NONE',  ( -73.00000337463099243, -25.98076211353322051, 17.49999999999999645 ) ) ;
#28112 = EDGE_LOOP ( 'NONE', ( #11978, #15406 ) ) ;
#28113 = EDGE_LOOP ( 'NONE', ( #6921, #12799, #31799, #21153, #34228, #4018 ) ) ;
#28114 = AXIS2_PLACEMENT_3D ( 'NONE', #23953, #32940, #20739 ) ;
#28115 = ADVANCED_FACE ( 'NONE', ( #21173, #4132 ), #15928, .F. ) ;
#28116 = CARTESIAN_POINT ( 'NONE',  ( 52.39915983220795681, 35.19434990244919703, -4.999999999999997335 ) ) ;
#28117 = CARTESIAN_POINT ( 'NONE',  ( 44.99999662536851019, -60.62177826491080168, 17.49999999999999645 ) ) ;
#28118 = CARTESIAN_POINT ( 'NONE',  ( -70.00000337463099243, 51.96152422706637708, 17.49999999999999645 ) ) ;
#28119 = EDGE_LOOP ( 'NONE', ( #17492, #26914 ) ) ;
#28120 = CIRCLE ( 'NONE', #18550, 95.00000000000000000 ) ;
#28121 = CARTESIAN_POINT ( 'NONE',  ( 74.99999662536835388, -25.98076211353319565, -9.999999999999998224 ) ) ;
#28122 = ORIENTED_EDGE ( 'NONE', *, *, #12096, .T. ) ;
#28123 = ORIENTED_EDGE ( 'NONE', *, *, #8414, .T. ) ;
#28124 = EDGE_CURVE ( 'NONE', #36485, #22685, #3925, .T. ) ;
#28125 = CARTESIAN_POINT ( 'NONE',  ( -83.00000337463092137, 25.98076211353317433, 12.50000000000000000 ) ) ;
#28126 = ORIENTED_EDGE ( 'NONE', *, *, #9309, .F. ) ;
#28127 = AXIS2_PLACEMENT_3D ( 'NONE', #28379, #36831, #34392 ) ;
#28128 = PRESENTATION_STYLE_ASSIGNMENT (( #3005 ) ) ;
#28129 = CARTESIAN_POINT ( 'NONE',  ( 47.63139720814400846, -27.50000000000022737, -10.00000000000000178 ) ) ;
#28130 = CARTESIAN_POINT ( 'NONE',  ( -70.00000337463099243, -2.428612866367529932E-14, 12.50000000000000000 ) ) ;
#28131 = AXIS2_PLACEMENT_3D ( 'NONE', #3854, #26188, #9504 ) ;
#28132 = ADVANCED_FACE ( 'NONE', ( #1478 ), #9738, .F. ) ;
#28133 = DIRECTION ( 'NONE',  ( 0.000000000000000000, 0.000000000000000000, 1.000000000000000000 ) ) ;
#28134 = CIRCLE ( 'NONE', #17963, 2.000000000000001776 ) ;
#28135 = VERTEX_POINT ( 'NONE', #27361 ) ;
#28136 = ORIENTED_EDGE ( 'NONE', *, *, #15171, .F. ) ;
#28137 = AXIS2_PLACEMENT_3D ( 'NONE', #35107, #12952, #18606 ) ;
#28138 = ORIENTED_EDGE ( 'NONE', *, *, #31170, .T. ) ;
#28139 = ORIENTED_EDGE ( 'NONE', *, *, #679, .T. ) ;
#28140 = VERTEX_POINT ( 'NONE', #21367 ) ;
#28141 = DIRECTION ( 'NONE',  ( 1.000000000000000000, 0.000000000000000000, 0.000000000000000000 ) ) ;
#28142 = CIRCLE ( 'NONE', #34155, 2.000000000000001776 ) ;
#28143 = DIRECTION ( 'NONE',  ( 0.000000000000000000, 0.000000000000000000, 1.000000000000000000 ) ) ;
#28144 = VECTOR ( 'NONE', #32939, 1000.000000000000000 ) ;
#28145 = DIRECTION ( 'NONE',  ( 0.000000000000000000, 0.000000000000000000, -1.000000000000000000 ) ) ;
#28146 = DIRECTION ( 'NONE',  ( 0.000000000000000000, 0.000000000000000000, 1.000000000000000000 ) ) ;
#28147 = CARTESIAN_POINT ( 'NONE',  ( 5.000000000000000000, 2.068880869914945020, -4.095521153410206949 ) ) ;
#28148 = EDGE_LOOP ( 'NONE', ( #16714, #7127 ) ) ;
#28149 = FACE_OUTER_BOUND ( 'NONE', #23633, .T. ) ;
#28150 = ADVANCED_FACE ( 'NONE', ( #32807 ), #4311, .T. ) ;
#28151 = DIRECTION ( 'NONE',  ( 0.000000000000000000, 0.000000000000000000, 1.000000000000000000 ) ) ;
#28152 = CARTESIAN_POINT ( 'NONE',  ( -76.71706625813334313, 9.685775882613420151, 12.50000000000000000 ) ) ;
#28153 = ORIENTED_EDGE ( 'NONE', *, *, #21585, .F. ) ;
#28154 = CARTESIAN_POINT ( 'NONE',  ( -45.00000337463112743, -60.62177826491080168, -9.999999999999998224 ) ) ;
#28155 = DIRECTION ( 'NONE',  ( 1.000000000000000000, 0.000000000000000000, 0.000000000000000000 ) ) ;
#28156 = CIRCLE ( 'NONE', #5420, 2.000000000000001776 ) ;
#28157 = ORIENTED_EDGE ( 'NONE', *, *, #7828, .F. ) ;
#28158 = EDGE_CURVE ( 'NONE', #29596, #26861, #20053, .T. ) ;
#28159 = VERTEX_POINT ( 'NONE', #24572 ) ;
#28160 = DIRECTION ( 'NONE',  ( 1.000000000000000000, 0.000000000000000000, 0.000000000000000000 ) ) ;
#28161 = EDGE_CURVE ( 'NONE', #34663, #5470, #36004, .T. ) ;
#28162 = DIRECTION ( 'NONE',  ( 0.000000000000000000, 0.000000000000000000, -1.000000000000000000 ) ) ;
#28163 = AXIS2_PLACEMENT_3D ( 'NONE', #8286, #19341, #19715 ) ;
#28164 = CARTESIAN_POINT ( 'NONE',  ( -77.00000337463097821, 8.660254037844374864, -9.999999999999998224 ) ) ;
#28165 = CARTESIAN_POINT ( 'NONE',  ( -2.068360682592148336, -4.579334095020483275, -0.01465562841810411250 ) ) ;
#28166 = VERTEX_POINT ( 'NONE', #9297 ) ;
#28167 = ORIENTED_EDGE ( 'NONE', *, *, #8726, .T. ) ;
#28168 = CIRCLE ( 'NONE', #11976, 30.00000000000000000 ) ;
#28169 = DIRECTION ( 'NONE',  ( 1.000000000000000000, 0.000000000000000000, 0.000000000000000000 ) ) ;
#28170 = ORIENTED_EDGE ( 'NONE', *, *, #35356, .F. ) ;
#28171 = FACE_OUTER_BOUND ( 'NONE', #15116, .T. ) ;
#28172 = ORIENTED_EDGE ( 'NONE', *, *, #11654, .T. ) ;
#28173 = CARTESIAN_POINT ( 'NONE',  ( 0.000000000000000000, 81.28776890242656350, 37.49999999999985079 ) ) ;
#28174 = EDGE_CURVE ( 'NONE', #6836, #34930, #5075, .T. ) ;
#28175 = FACE_OUTER_BOUND ( 'NONE', #14135, .T. ) ;
#28176 = EDGE_LOOP ( 'NONE', ( #21075, #30514, #3453 ) ) ;
#28177 = ORIENTED_EDGE ( 'NONE', *, *, #19763, .F. ) ;
#28178 = CARTESIAN_POINT ( 'NONE',  ( -3.866666666667000651, 4.735300956703508322E-16, 2.266666666667000563 ) ) ;
#28179 = DIRECTION ( 'NONE',  ( 0.000000000000000000, 0.000000000000000000, 1.000000000000000000 ) ) ;
#28180 = CARTESIAN_POINT ( 'NONE',  ( 46.99999662536851019, -60.62177826491080168, -9.999999999999998224 ) ) ;
#28181 = CARTESIAN_POINT ( 'NONE',  ( 4.999999999999999112, 2.886751345948153968, -0.5999999999999998668 ) ) ;
#28182 = ORIENTED_EDGE ( 'NONE', *, *, #415, .T. ) ;
#28183 = CARTESIAN_POINT ( 'NONE',  ( 1.999996625368696490, -86.60254037844400443, 12.50000000000000000 ) ) ;
#28184 = AXIS2_PLACEMENT_3D ( 'NONE', #18003, #4134, #29427 ) ;
#28185 = FACE_BOUND ( 'NONE', #32556, .T. ) ;
#28186 = DIRECTION ( 'NONE',  ( 1.000000000000000000, 0.000000000000000000, 0.000000000000000000 ) ) ;
#28187 = CARTESIAN_POINT ( 'NONE',  ( 0.000000000000000000, 0.000000000000000000, -5.700000000000000178 ) ) ;
#28188 = FACE_OUTER_BOUND ( 'NONE', #24714, .T. ) ;
#28189 = DIRECTION ( 'NONE',  ( 0.000000000000000000, 0.000000000000000000, 1.000000000000000000 ) ) ;
#28190 = EDGE_CURVE ( 'NONE', #35211, #9870, #5756, .T. ) ;
#28191 = CARTESIAN_POINT ( 'NONE',  ( -46.74666114985175369, -61.59604035298635694, 12.50000000000000000 ) ) ;
#28192 = DIRECTION ( 'NONE',  ( 0.000000000000000000, 0.000000000000000000, 1.000000000000000000 ) ) ;
#28193 = ORIENTED_EDGE ( 'NONE', *, *, #3325, .F. ) ;
#28194 = ADVANCED_FACE ( 'NONE', ( #3515 ), #15300, .F. ) ;
#28195 = DIRECTION ( 'NONE',  ( 0.000000000000000000, 0.000000000000000000, 1.000000000000000000 ) ) ;
#28196 = DIRECTION ( 'NONE',  ( -0.8660254037844449249, -0.4999999999999888978, 0.000000000000000000 ) ) ;
#28197 = DIRECTION ( 'NONE',  ( 1.000000000000000000, 0.000000000000000000, 0.000000000000000000 ) ) ;
#28198 = VERTEX_POINT ( 'NONE', #12483 ) ;
#28199 = EDGE_CURVE ( 'NONE', #36258, #35811, #29371, .T. ) ;
#28200 = EDGE_LOOP ( 'NONE', ( #36408, #17125, #24732 ) ) ;
#28201 = ORIENTED_EDGE ( 'NONE', *, *, #5521, .F. ) ;
#28202 = DIRECTION ( 'NONE',  ( -1.000000000000000000, 0.000000000000000000, 0.000000000000000000 ) ) ;
#28203 = CARTESIAN_POINT ( 'NONE',  ( -77.00000337463100664, -43.30127018922202353, 17.49999999999999645 ) ) ;
#28204 = EDGE_CURVE ( 'NONE', #15127, #36972, #21111, .T. ) ;
#28205 = ORIENTED_EDGE ( 'NONE', *, *, #31407, .T. ) ;
#28206 = EDGE_CURVE ( 'NONE', #29785, #25826, #33229, .T. ) ;
#28207 = B_SPLINE_CURVE_WITH_KNOTS ( 'NONE', 3,
 ( #6273, #24086, #8915, #20351, #6655 ),
 .UNSPECIFIED., .F., .F.,
 ( 4, 1, 4 ),
 ( 6.279784878834714258E-20, 0.002886751345948134623, 0.005773502691896268378 ),
 .UNSPECIFIED. ) ;
#28208 = CARTESIAN_POINT ( 'NONE',  ( 17.14523346298344109, -93.36492675454773860, -4.999999999999997335 ) ) ;
#28209 = ORIENTED_EDGE ( 'NONE', *, *, #26511, .F. ) ;
#28210 = AXIS2_PLACEMENT_3D ( 'NONE', #30118, #35415, #32191 ) ;
#28211 = FACE_OUTER_BOUND ( 'NONE', #7009, .T. ) ;
#28212 = VERTEX_POINT ( 'NONE', #5959 ) ;
#28213 = CARTESIAN_POINT ( 'NONE',  ( -77.00000337463097821, 8.660254037844374864, -9.999999999999998224 ) ) ;
#28214 = EDGE_CURVE ( 'NONE', #21455, #12472, #11739, .T. ) ;
#28215 = ORIENTED_EDGE ( 'NONE', *, *, #18805, .T. ) ;
#28216 = EDGE_CURVE ( 'NONE', #32044, #36485, #26024, .T. ) ;
#28217 = DIRECTION ( 'NONE',  ( -1.000000000000000000, 0.000000000000000000, 0.000000000000000000 ) ) ;
#28218 = DIRECTION ( 'NONE',  ( 0.000000000000000000, 0.000000000000000000, 1.000000000000000000 ) ) ;
#28219 = EDGE_CURVE ( 'NONE', #4119, #26898, #21856, .T. ) ;
#28220 = ADVANCED_FACE ( 'NONE', ( #35200 ), #20939, .F. ) ;
#28221 = EDGE_CURVE ( 'NONE', #14572, #2310, #17945, .T. ) ;
#28222 = ORIENTED_EDGE ( 'NONE', *, *, #10333, .T. ) ;
#28223 = CARTESIAN_POINT ( 'NONE',  ( 124.4080600076930665, -12.15049814296675201, 27.50000000000000000 ) ) ;
#28224 = CONTEXT_DEPENDENT_SHAPE_REPRESENTATION ( #10638, #13097 ) ;
#28225 = DIRECTION ( 'NONE',  ( 0.000000000000000000, 0.000000000000000000, 1.000000000000000000 ) ) ;
#28226 = DIRECTION ( 'NONE',  ( 0.000000000000000000, 0.000000000000000000, 1.000000000000000000 ) ) ;
#28227 = ORIENTED_EDGE ( 'NONE', *, *, #11407, .T. ) ;
#28228 = DIRECTION ( 'NONE',  ( 0.000000000000000000, 0.000000000000000000, 1.000000000000000000 ) ) ;
#28229 = DIRECTION ( 'NONE',  ( 1.000000000000000000, 0.000000000000000000, 0.000000000000000000 ) ) ;
#28230 = ORIENTED_EDGE ( 'NONE', *, *, #32760, .F. ) ;
#28231 = CARTESIAN_POINT ( 'NONE',  ( -19.31922176934808633, 76.99660315353983719, -19.99999999999999645 ) ) ;
#28232 = AXIS2_PLACEMENT_3D ( 'NONE', #13133, #24753, #19146 ) ;
#28233 = DIRECTION ( 'NONE',  ( 0.000000000000000000, 0.000000000000000000, 1.000000000000000000 ) ) ;
#28234 = PLANE ( 'NONE',  #33951 ) ;
#28235 = DIRECTION ( 'NONE',  ( -1.000000000000000000, 0.000000000000000000, 0.000000000000000000 ) ) ;
#28236 = ORIENTED_EDGE ( 'NONE', *, *, #33235, .F. ) ;
#28237 = ORIENTED_EDGE ( 'NONE', *, *, #21482, .T. ) ;
#28238 = DIRECTION ( 'NONE',  ( 0.000000000000000000, 0.000000000000000000, 1.000000000000000000 ) ) ;
#28239 = CARTESIAN_POINT ( 'NONE',  ( -53.00000337463110611, -43.30127018922202353, -5.000000000000000000 ) ) ;
#28240 = ORIENTED_EDGE ( 'NONE', *, *, #32607, .F. ) ;
#28241 = ORIENTED_EDGE ( 'NONE', *, *, #7610, .T. ) ;
#28242 = CARTESIAN_POINT ( 'NONE',  ( 0.000000000000000000, 0.000000000000000000, -5.000000000000000000 ) ) ;
#28243 = CARTESIAN_POINT ( 'NONE',  ( -20.00000000000001066, 89.94802294027088863, 27.49999999999999645 ) ) ;
#28244 = CARTESIAN_POINT ( 'NONE',  ( -57.00000337463109901, -60.62177826491083010, 12.50000000000000000 ) ) ;
#28245 = ORIENTED_EDGE ( 'NONE', *, *, #489, .T. ) ;
#28246 = ORIENTED_EDGE ( 'NONE', *, *, #26387, .F. ) ;
#28247 = DIRECTION ( 'NONE',  ( 0.000000000000000000, 0.000000000000000000, -1.000000000000000000 ) ) ;
#28248 = VECTOR ( 'NONE', #5124, 1000.000000000000000 ) ;
#28249 = CARTESIAN_POINT ( 'NONE',  ( 69.99999662536838230, -34.64101615137759183, -5.000000000000000000 ) ) ;
#28250 = EDGE_LOOP ( 'NONE', ( #33269, #6203, #34234, #15711 ) ) ;
#28251 = DIRECTION ( 'NONE',  ( -0.000000000000000000, -0.000000000000000000, 1.000000000000000000 ) ) ;
#28252 = ORIENTED_EDGE ( 'NONE', *, *, #241, .F. ) ;
#28253 = AXIS2_PLACEMENT_3D ( 'NONE', #13902, #30, #17286 ) ;
#28254 = FACE_BOUND ( 'NONE', #8465, .T. ) ;
#28255 = EDGE_CURVE ( 'NONE', #25448, #20697, #8685, .T. ) ;
#28256 = CYLINDRICAL_SURFACE ( 'NONE', #28689, 95.00000000000001421 ) ;
#28257 = EDGE_CURVE ( 'NONE', #24628, #16096, #23948, .T. ) ;
#28258 = EDGE_CURVE ( 'NONE', #12074, #24619, #860, .T. ) ;
#28259 = ORIENTED_EDGE ( 'NONE', *, *, #10564, .T. ) ;
#28260 = DIRECTION ( 'NONE',  ( 0.000000000000000000, 0.000000000000000000, 1.000000000000000000 ) ) ;
#28261 = CARTESIAN_POINT ( 'NONE',  ( 25.00000000000000000, 3.061616997868383043E-15, 15.00000000000000000 ) ) ;
#28262 = DIRECTION ( 'NONE',  ( 0.000000000000000000, 0.000000000000000000, 1.000000000000000000 ) ) ;
#28263 = DIRECTION ( 'NONE',  ( 0.000000000000000000, 0.000000000000000000, -1.000000000000000000 ) ) ;
#28264 = ORIENTED_EDGE ( 'NONE', *, *, #35692, .T. ) ;
#28265 = CARTESIAN_POINT ( 'NONE',  ( 36.99999662536855283, -77.94228634059960825, 17.49999999999999645 ) ) ;
#28266 = CYLINDRICAL_SURFACE ( 'NONE', #20806, 2.000000000000001776 ) ;
#28267 = CARTESIAN_POINT ( 'NONE',  ( -55.00000337463107059, 60.62177826491078747, -5.000000000000000000 ) ) ;
#28268 = ORIENTED_EDGE ( 'NONE', *, *, #35479, .F. ) ;
#28269 = ORIENTED_EDGE ( 'NONE', *, *, #7818, .T. ) ;
#28270 = AXIS2_PLACEMENT_3D ( 'NONE', #11314, #2678, #34752 ) ;
#28271 = ORIENTED_EDGE ( 'NONE', *, *, #22400, .T. ) ;
#28272 = CARTESIAN_POINT ( 'NONE',  ( 58.88972745734179171, -34.00000000000007105, 12.49999999999999822 ) ) ;
#28273 = DIRECTION ( 'NONE',  ( 0.000000000000000000, 0.000000000000000000, 1.000000000000000000 ) ) ;
#28274 = EDGE_CURVE ( 'NONE', #29492, #31614, #9114, .T. ) ;
#28275 = CARTESIAN_POINT ( 'NONE',  ( 4.999996625368676284, -77.94228634059960825, -9.999999999999998224 ) ) ;
#28276 = DIRECTION ( 'NONE',  ( 0.000000000000000000, -0.4999999999999996114, 0.8660254037844388186 ) ) ;
#28277 = DIRECTION ( 'NONE',  ( 0.000000000000000000, 0.000000000000000000, -1.000000000000000000 ) ) ;
#28278 = CARTESIAN_POINT ( 'NONE',  ( -98.00106544729364089, -66.93781643011477911, 32.49999999999999289 ) ) ;
#28279 = CARTESIAN_POINT ( 'NONE',  ( 34.99999662536855283, 60.62177826491078747, -9.999999999999998224 ) ) ;
#28280 = DIRECTION ( 'NONE',  ( 0.000000000000000000, 0.000000000000000000, 1.000000000000000000 ) ) ;
#28281 = ORIENTED_EDGE ( 'NONE', *, *, #13286, .F. ) ;
#28282 = ORIENTED_EDGE ( 'NONE', *, *, #2668, .T. ) ;
#28283 = CIRCLE ( 'NONE', #28861, 2.000000000000001776 ) ;
#28284 = CIRCLE ( 'NONE', #33081, 3.250000000000001332 ) ;
#28285 = CARTESIAN_POINT ( 'NONE',  ( 3.000000000000000888, 0.000000000000000000, -5.700000000000000178 ) ) ;
#28286 = DIRECTION ( 'NONE',  ( 0.000000000000000000, 0.000000000000000000, -1.000000000000000000 ) ) ;
#28287 = CYLINDRICAL_SURFACE ( 'NONE', #12039, 2.000000000000001776 ) ;
#28288 = CYLINDRICAL_SURFACE ( 'NONE', #11898, 2.000000000000001776 ) ;
#28289 = ORIENTED_EDGE ( 'NONE', *, *, #22021, .T. ) ;
#28290 = DIRECTION ( 'NONE',  ( 1.000000000000000000, 0.000000000000000000, 0.000000000000000000 ) ) ;
#28291 = ORIENTED_EDGE ( 'NONE', *, *, #16334, .F. ) ;
#28292 = VECTOR ( 'NONE', #21769, 1000.000000000000000 ) ;
#28293 = EDGE_LOOP ( 'NONE', ( #5641, #36038, #3142, #34748 ) ) ;
#28294 = EDGE_CURVE ( 'NONE', #23645, #28919, #27226, .T. ) ;
#28295 = PLANE ( 'NONE',  #20622 ) ;
#28296 = ORIENTED_EDGE ( 'NONE', *, *, #17980, .F. ) ;
#28297 = DIRECTION ( 'NONE',  ( 1.000000000000000000, 0.000000000000000000, 0.000000000000000000 ) ) ;
#28298 = CARTESIAN_POINT ( 'NONE',  ( -31.74999999999995737, 0.000000000000000000, 0.000000000000000000 ) ) ;
#28299 = CARTESIAN_POINT ( 'NONE',  ( 84.99999662536832545, 25.98076211353319565, 17.49999999999999645 ) ) ;
#28300 = EDGE_LOOP ( 'NONE', ( #163, #675, #16078, #16849 ) ) ;
#28301 = ORIENTED_EDGE ( 'NONE', *, *, #29066, .F. ) ;
#28302 = ORIENTED_EDGE ( 'NONE', *, *, #33101, .T. ) ;
#28303 = EDGE_LOOP ( 'NONE', ( #20636, #17148, #29416, #3936, #5458, #28703 ) ) ;
#28304 = AXIS2_PLACEMENT_3D ( 'NONE', #17285, #9380, #6580 ) ;
#28305 = EDGE_LOOP ( 'NONE', ( #10107, #6429, #23656 ) ) ;
#28306 = DIRECTION ( 'NONE',  ( 0.000000000000000000, 0.000000000000000000, -1.000000000000000000 ) ) ;
#28307 = EDGE_CURVE ( 'NONE', #24720, #18017, #36823, .T. ) ;
#28308 = CARTESIAN_POINT ( 'NONE',  ( 69.99999662536838230, -51.96152422706639840, 12.50000000000000000 ) ) ;
#28309 = CARTESIAN_POINT ( 'NONE',  ( 0.000000000000000000, 0.000000000000000000, 12.49999999999999822 ) ) ;
#28310 = DIRECTION ( 'NONE',  ( 1.000000000000000000, 0.000000000000000000, 0.000000000000000000 ) ) ;
#28311 = CARTESIAN_POINT ( 'NONE',  ( 36.99999662536855283, -77.94228634059960825, -9.999999999999998224 ) ) ;
#28312 = EDGE_CURVE ( 'NONE', #16370, #31031, #14056, .T. ) ;
#28313 = EDGE_LOOP ( 'NONE', ( #32961, #13774 ) ) ;
#28314 = CARTESIAN_POINT ( 'NONE',  ( 51.13139720814399425, -27.50000000000022737, -5.000000000000000000 ) ) ;
#28315 = CARTESIAN_POINT ( 'NONE',  ( 46.99999662536849598, 60.62177826491077326, -9.999999999999998224 ) ) ;
#28316 = AXIS2_PLACEMENT_3D ( 'NONE', #23531, #34113, #8418 ) ;
#28317 = CARTESIAN_POINT ( 'NONE',  ( 65.00000000000000000, 7.960204194457797252E-15, 5.000000000000000000 ) ) ;
#28318 = EDGE_LOOP ( 'NONE', ( #19198, #24495, #30776, #15353 ) ) ;
#28319 = CARTESIAN_POINT ( 'NONE',  ( 0.000000000000000000, 0.000000000000000000, 17.49999999999999645 ) ) ;
#28320 = EDGE_CURVE ( 'NONE', #13311, #12717, #32630, .T. ) ;
#28321 = CARTESIAN_POINT ( 'NONE',  ( 34.60911832077664485, -75.98085468209112037, 12.50000000000000000 ) ) ;
#28322 = VERTEX_POINT ( 'NONE', #7247 ) ;
#28323 = ORIENTED_EDGE ( 'NONE', *, *, #12407, .T. ) ;
#28324 = ADVANCED_FACE ( 'NONE', ( #35566 ), #27286, .T. ) ;
#28325 = FACE_OUTER_BOUND ( 'NONE', #21593, .T. ) ;
#28326 = CARTESIAN_POINT ( 'NONE',  ( 66.99999662536841072, 25.98076211353318854, -9.999999999999998224 ) ) ;
#28327 = DIRECTION ( 'NONE',  ( 0.000000000000000000, 0.000000000000000000, 1.000000000000000000 ) ) ;
#28328 = CARTESIAN_POINT ( 'NONE',  ( -5.184911785340888812, -2.993510214990782625, -4.330720594357050146 ) ) ;
#28329 = ORIENTED_EDGE ( 'NONE', *, *, #2301, .F. ) ;
#28330 = ORIENTED_EDGE ( 'NONE', *, *, #27736, .F. ) ;
#28331 = CIRCLE ( 'NONE', #3787, 2.000000000000001776 ) ;
#28332 = PLANE ( 'NONE',  #36855 ) ;
#28333 = CIRCLE ( 'NONE', #18769, 27.00000000000001421 ) ;
#28334 = ORIENTED_EDGE ( 'NONE', *, *, #27786, .F. ) ;
#28335 = EDGE_CURVE ( 'NONE', #17344, #30803, #11088, .T. ) ;
#28336 = CARTESIAN_POINT ( 'NONE',  ( 46.74665512060159500, 61.59603906214631763, -5.000000000000000000 ) ) ;
#28337 = VERTEX_POINT ( 'NONE', #12843 ) ;
#28338 = DIRECTION ( 'NONE',  ( 0.000000000000000000, 0.000000000000000000, 1.000000000000000000 ) ) ;
#28339 = PLANE ( 'NONE',  #32541 ) ;
#28340 = CARTESIAN_POINT ( 'NONE',  ( -40.98360655737705827, 111.1639425680974398, 27.49999999999999645 ) ) ;
#28341 = AXIS2_PLACEMENT_3D ( 'NONE', #34758, #225, #17485 ) ;
#28342 = CARTESIAN_POINT ( 'NONE',  ( -62.00000337463108480, -51.96152422706641971, -9.999999999999998224 ) ) ;
#28343 = VERTEX_POINT ( 'NONE', #21852 ) ;
#28344 = ORIENTED_EDGE ( 'NONE', *, *, #14907, .T. ) ;
#28345 = DIRECTION ( 'NONE',  ( 1.000000000000000000, 0.000000000000000000, 0.000000000000000000 ) ) ;
#28346 = CYLINDRICAL_SURFACE ( 'NONE', #36447, 2.000000000000001776 ) ;
#28347 = CIRCLE ( 'NONE', #810, 2.000000000000001776 ) ;
#28348 = ADVANCED_FACE ( 'NONE', ( #1609 ), #4253, .F. ) ;
#28349 = FACE_OUTER_BOUND ( 'NONE', #30395, .T. ) ;
#28350 = DIRECTION ( 'NONE',  ( 0.000000000000000000, 0.000000000000000000, -1.000000000000000000 ) ) ;
#28351 = ORIENTED_EDGE ( 'NONE', *, *, #33669, .F. ) ;
#28352 = DIRECTION ( 'NONE',  ( 0.8660254037844415942, 0.4999999999999949485, 0.000000000000000000 ) ) ;
#28353 = ADVANCED_FACE ( 'NONE', ( #10411 ), #24682, .F. ) ;
#28354 = FACE_BOUND ( 'NONE', #3143, .T. ) ;
#28355 = DIRECTION ( 'NONE',  ( 1.000000000000000000, 0.000000000000000000, 0.000000000000000000 ) ) ;
#28356 = VECTOR ( 'NONE', #21982, 1000.000000000000000 ) ;
#28357 = CARTESIAN_POINT ( 'NONE',  ( -60.00000337463107059, -34.64101615137762025, 12.50000000000000000 ) ) ;
#28358 = DIRECTION ( 'NONE',  ( -1.000000000000000000, 0.000000000000000000, 0.000000000000000000 ) ) ;
#28359 = DIRECTION ( 'NONE',  ( -0.000000000000000000, -0.000000000000000000, 1.000000000000000000 ) ) ;
#28360 = AXIS2_PLACEMENT_3D ( 'NONE', #24702, #32955, #12683 ) ;
#28361 = CARTESIAN_POINT ( 'NONE',  ( -5.089798516654387761, 119.6083603441600047, 27.49998800000000543 ) ) ;
#28362 = DIRECTION ( 'NONE',  ( -0.000000000000000000, 0.000000000000000000, -1.000000000000000000 ) ) ;
#28363 = ORIENTED_EDGE ( 'NONE', *, *, #2482, .F. ) ;
#28364 = CARTESIAN_POINT ( 'NONE',  ( 41.99999662536853151, -69.28203230275519786, 12.50000000000000000 ) ) ;
#28365 = EDGE_CURVE ( 'NONE', #28166, #13878, #4520, .T. ) ;
#28366 = DIRECTION ( 'NONE',  ( -1.000000000000000000, 0.000000000000000000, 0.000000000000000000 ) ) ;
#28367 = DIRECTION ( 'NONE',  ( 1.000000000000000000, 0.000000000000000000, 0.000000000000000000 ) ) ;
#28368 = AXIS2_PLACEMENT_3D ( 'NONE', #34055, #22803, #2924 ) ;
#28369 = VERTEX_POINT ( 'NONE', #7614 ) ;
#28370 = EDGE_LOOP ( 'NONE', ( #3668, #2640 ) ) ;
#28371 = VERTEX_POINT ( 'NONE', #7423 ) ;
#28372 = EDGE_CURVE ( 'NONE', #28959, #16790, #24573, .T. ) ;
#28373 = STYLED_ITEM ( 'NONE', ( #29851 ), #19278 ) ;
#28374 = DIRECTION ( 'NONE',  ( 0.000000000000000000, 0.000000000000000000, 1.000000000000000000 ) ) ;
#28375 = DIRECTION ( 'NONE',  ( 0.000000000000000000, 0.000000000000000000, 1.000000000000000000 ) ) ;
#28376 = VERTEX_POINT ( 'NONE', #16059 ) ;
#28377 = CARTESIAN_POINT ( 'NONE',  ( 22.99999662536857059, 77.94228634059957983, 12.50000000000000000 ) ) ;
#28378 = ORIENTED_EDGE ( 'NONE', *, *, #367, .T. ) ;
#28379 = CARTESIAN_POINT ( 'NONE',  ( -25.00000337463121980, -77.94228634059963667, -9.999999999999998224 ) ) ;
#28380 = VERTEX_POINT ( 'NONE', #21295 ) ;
#28381 = CARTESIAN_POINT ( 'NONE',  ( 54.99999662536844625, 60.62177826491077326, 12.50000000000000000 ) ) ;
#28382 = ORIENTED_EDGE ( 'NONE', *, *, #20823, .T. ) ;
#28383 = ORIENTED_EDGE ( 'NONE', *, *, #11951, .F. ) ;
#28384 = CIRCLE ( 'NONE', #20016, 2.000000000000001776 ) ;
#28385 = EDGE_CURVE ( 'NONE', #16153, #20325, #3303, .T. ) ;
#28386 = CARTESIAN_POINT ( 'NONE',  ( 65.00000000000000000, 7.960204194457797252E-15, 5.000000000000000000 ) ) ;
#28387 = CARTESIAN_POINT ( 'NONE',  ( 77.99999662536832545, -17.32050807568879591, -9.999999999999998224 ) ) ;
#28388 = ORIENTED_EDGE ( 'NONE', *, *, #24241, .F. ) ;
#28389 = DIRECTION ( 'NONE',  ( 0.000000000000000000, 0.000000000000000000, 1.000000000000000000 ) ) ;
#28390 = EDGE_CURVE ( 'NONE', #30085, #21337, #3914, .T. ) ;
#28391 = LINE ( 'NONE', #2166, #13485 ) ;
#28392 = DIRECTION ( 'NONE',  ( 1.000000000000000000, 0.000000000000000000, 0.000000000000000000 ) ) ;
#28393 = ORIENTED_EDGE ( 'NONE', *, *, #3278, .F. ) ;
#28394 = CARTESIAN_POINT ( 'NONE',  ( 104.8061974404898820, 19.22934205794938478, 27.50000000000000000 ) ) ;
#28395 = CARTESIAN_POINT ( 'NONE',  ( 0.000000000000000000, 0.000000000000000000, -5.000000000000000000 ) ) ;
#28397 = VERTEX_POINT ( 'NONE', #19061 ) ;
#28396 = ADVANCED_FACE ( 'NONE', ( #4426 ), #27102, .F. ) ;
#28398 = B_SPLINE_CURVE_WITH_KNOTS ( 'NONE', 3,
 ( #3920, #32422, #35059, #9168, #562, #6178, #9734, #21170, #29037, #17606, #3570, #20600, #17997, #1122, #12346, #23815, #9563, #15175, #3740, #26430, #31842, #32024, #11984, #3374, #32600, #6924, #26250, #34877, #738, #17806, #35268, #12547, #20994, #6735, #29598 ),
 .UNSPECIFIED., .F., .F.,
 ( 4, 2, 1, 1, 2, 2, 1, 2, 2, 2, 2, 1, 2, 2, 1, 2, 2, 1, 1, 2, 4 ),
 ( 0.05563282717590559839, 0.06778080578341673379, 0.07992878439092786225, 0.1042247416059501192, 0.1163727202134613725, 0.1285206988209726398, 0.1528166560359950910, 0.1771126132510175422, 0.1892605918585288927, 0.2014085704660402432, 0.2500004848960857839, 0.2985923993261312415, 0.3107403779336425642, 0.3228883565411538870, 0.3471843137561765325, 0.3714802709711991224, 0.3836282495787105007, 0.3957762281862218789, 0.4200721854012446355, 0.4322201640087560692, 0.4443681426162675030 ),
 .UNSPECIFIED. ) ;
#28399 = CYLINDRICAL_SURFACE ( 'NONE', #9430, 25.00000000000000000 ) ;
#28400 = EDGE_CURVE ( 'NONE', #24755, #28819, #17091, .T. ) ;
#28401 = DIRECTION ( 'NONE',  ( 3.491481338843135327E-15, 1.000000000000000000, 0.000000000000000000 ) ) ;
#28402 = CYLINDRICAL_SURFACE ( 'NONE', #35769, 2.000000000000001776 ) ;
#28403 = LINE ( 'NONE', #2729, #9273 ) ;
#28404 = ORIENTED_EDGE ( 'NONE', *, *, #8071, .T. ) ;
#28405 = ORIENTED_EDGE ( 'NONE', *, *, #29821, .T. ) ;
#28406 = CIRCLE ( 'NONE', #2071, 1.999999999999998224 ) ;
#28407 = CYLINDRICAL_SURFACE ( 'NONE', #26146, 150.0000000000000284 ) ;
#28408 = DIRECTION ( 'NONE',  ( -0.000000000000000000, -0.000000000000000000, 1.000000000000000000 ) ) ;
#28409 = AXIS2_PLACEMENT_3D ( 'NONE', #17452, #28512, #26 ) ;
#28410 = ORIENTED_EDGE ( 'NONE', *, *, #7868, .T. ) ;
#28411 = ORIENTED_EDGE ( 'NONE', *, *, #9951, .F. ) ;
#28412 = EDGE_CURVE ( 'NONE', #7932, #30738, #19476, .T. ) ;
#28413 = DIRECTION ( 'NONE',  ( 0.000000000000000000, 0.000000000000000000, 1.000000000000000000 ) ) ;
#28414 = CARTESIAN_POINT ( 'NONE',  ( -35.00000337463116296, -60.62177826491080168, 12.50000000000000000 ) ) ;
#28415 = CARTESIAN_POINT ( 'NONE',  ( -67.00000337463102085, 60.62177826491077326, -9.999999999999998224 ) ) ;
#28416 = ORIENTED_EDGE ( 'NONE', *, *, #4809, .F. ) ;
#28417 = CIRCLE ( 'NONE', #18880, 27.00000000000001421 ) ;
#28418 = AXIS2_PLACEMENT_3D ( 'NONE', #9719, #7284, #32581 ) ;
#28419 = ORIENTED_EDGE ( 'NONE', *, *, #35923, .F. ) ;
#28420 = VECTOR ( 'NONE', #34081, 1000.000000000000000 ) ;
#28421 = CARTESIAN_POINT ( 'NONE',  ( 54.99999662536844625, -60.62177826491080168, 17.49999999999999645 ) ) ;
#28422 = CIRCLE ( 'NONE', #33219, 2.000000000000001776 ) ;
#28423 = DIRECTION ( 'NONE',  ( -1.000000000000000000, 0.000000000000000000, 0.000000000000000000 ) ) ;
#28424 = EDGE_LOOP ( 'NONE', ( #27444, #4003 ) ) ;
#28425 = DIRECTION ( 'NONE',  ( 0.000000000000000000, 0.000000000000000000, -1.000000000000000000 ) ) ;
#28426 = EDGE_LOOP ( 'NONE', ( #6078, #24783 ) ) ;
#28427 = CARTESIAN_POINT ( 'NONE',  ( 54.99999662536844625, 60.62177826491077326, -9.999999999999998224 ) ) ;
#28428 = EDGE_CURVE ( 'NONE', #20425, #15155, #5720, .T. ) ;
#28429 = DIRECTION ( 'NONE',  ( 0.000000000000000000, 0.000000000000000000, 1.000000000000000000 ) ) ;
#28430 = EDGE_CURVE ( 'NONE', #18017, #2273, #18507, .T. ) ;
#28431 = CIRCLE ( 'NONE', #20635, 150.0000000000000284 ) ;
#28432 = ORIENTED_EDGE ( 'NONE', *, *, #27147, .T. ) ;
#28433 = CARTESIAN_POINT ( 'NONE',  ( 0.000000000000000000, 0.000000000000000000, 0.000000000000000000 ) ) ;
#28434 = EDGE_CURVE ( 'NONE', #2403, #8706, #8102, .T. ) ;
#28435 = VECTOR ( 'NONE', #8596, 1000.000000000000000 ) ;
#28436 = DIRECTION ( 'NONE',  ( -0.000000000000000000, -0.000000000000000000, 1.000000000000000000 ) ) ;
#28437 = CARTESIAN_POINT ( 'NONE',  ( -80.00000337463094979, -17.32050807568882078, -9.999999999999998224 ) ) ;
#28438 = CARTESIAN_POINT ( 'NONE',  ( -3.374631334790434423E-06, 69.28203230275516944, -9.999999999999998224 ) ) ;
#28439 = ORIENTED_EDGE ( 'NONE', *, *, #7594, .T. ) ;
#28440 = CARTESIAN_POINT ( 'NONE',  ( -87.00000337463093558, 25.98076211353317433, -9.999999999999998224 ) ) ;
#28441 = EDGE_CURVE ( 'NONE', #33934, #4453, #15296, .T. ) ;
#28442 = DIRECTION ( 'NONE',  ( -1.000000000000000000, 0.000000000000000000, 0.000000000000000000 ) ) ;
#28443 = DIRECTION ( 'NONE',  ( 0.000000000000000000, 0.000000000000000000, -1.000000000000000000 ) ) ;
#28444 = AXIS2_PLACEMENT_3D ( 'NONE', #3691, #34453, #26382 ) ;
#28445 = AXIS2_PLACEMENT_3D ( 'NONE', #16284, #10277, #2014 ) ;
#28446 = ORIENTED_EDGE ( 'NONE', *, *, #14972, .T. ) ;
#28447 = EDGE_LOOP ( 'NONE', ( #5102, #25781, #30089, #4903 ) ) ;
#28448 = EDGE_LOOP ( 'NONE', ( #19295, #14502, #15876, #22876 ) ) ;
#28449 = FACE_OUTER_BOUND ( 'NONE', #2033, .T. ) ;
#28450 = ADVANCED_FACE ( 'NONE', ( #2160 ), #25605, .F. ) ;
#28451 = EDGE_CURVE ( 'NONE', #26458, #30803, #296, .T. ) ;
#28452 = DIRECTION ( 'NONE',  ( -1.000000000000000000, 0.000000000000000000, 0.000000000000000000 ) ) ;
#28453 = EDGE_CURVE ( 'NONE', #11641, #34302, #10507, .T. ) ;
#28454 = AXIS2_PLACEMENT_3D ( 'NONE', #30290, #6858, #32540 ) ;
#28455 = EDGE_CURVE ( 'NONE', #33896, #28909, #25060, .T. ) ;
#28456 = CARTESIAN_POINT ( 'NONE',  ( 5.000000000000000000, 30.00000000000000355, -15.00000000000000000 ) ) ;
#28457 = DIRECTION ( 'NONE',  ( -1.000000000000000000, 0.000000000000000000, 0.000000000000000000 ) ) ;
#28458 = CARTESIAN_POINT ( 'NONE',  ( 0.000000000000000000, 5.773502691896262640, -6.000000000000000000 ) ) ;
#28459 = VECTOR ( 'NONE', #8865, 1000.000000000000000 ) ;
#28460 = CYLINDRICAL_SURFACE ( 'NONE', #22621, 2.000000000000001776 ) ;
#28461 = AXIS2_PLACEMENT_3D ( 'NONE', #6796, #4200, #32310 ) ;
#28462 = CARTESIAN_POINT ( 'NONE',  ( -27.78182860042817026, -56.67878100130359087, 12.49999999999999822 ) ) ;
#28463 = ORIENTED_EDGE ( 'NONE', *, *, #27317, .F. ) ;
#28464 = CIRCLE ( 'NONE', #21893, 3.050000000000000711 ) ;
#28465 = ORIENTED_EDGE ( 'NONE', *, *, #18350, .T. ) ;
#28466 = CARTESIAN_POINT ( 'NONE',  ( 27.99999662536857414, -69.28203230275519786, -9.999999999999998224 ) ) ;
#28467 = VECTOR ( 'NONE', #24029, 1000.000000000000000 ) ;
#28468 = CARTESIAN_POINT ( 'NONE',  ( -45.00000000000000000, 0.000000000000000000, 15.00000000000000000 ) ) ;
#28469 = DIRECTION ( 'NONE',  ( 0.000000000000000000, 0.4999999999999953926, 0.8660254037844412611 ) ) ;
#28470 = CARTESIAN_POINT ( 'NONE',  ( 3.499999999999987566, -55.00000000000000000, -10.00000000000000178 ) ) ;
#28471 = ORIENTED_EDGE ( 'NONE', *, *, #25907, .F. ) ;
#28472 = CIRCLE ( 'NONE', #312, 27.00000000000001421 ) ;
#28473 = AXIS2_PLACEMENT_3D ( 'NONE', #12108, #26566, #23574 ) ;
#28474 = FACE_BOUND ( 'NONE', #31786, .T. ) ;
#28475 = ORIENTED_EDGE ( 'NONE', *, *, #13882, .F. ) ;
#28476 = ORIENTED_EDGE ( 'NONE', *, *, #4185, .T. ) ;
#28477 = DIRECTION ( 'NONE',  ( 0.000000000000000000, 0.000000000000000000, 1.000000000000000000 ) ) ;
#28478 = ORIENTED_EDGE ( 'NONE', *, *, #36873, .T. ) ;
#28479 = FILL_AREA_STYLE ('',( #343 ) ) ;
#28480 = EDGE_CURVE ( 'NONE', #24664, #34239, #17672, .T. ) ;
#28481 = LINE ( 'NONE', #36751, #23930 ) ;
#28482 = DIRECTION ( 'NONE',  ( 1.000000000000000000, 0.000000000000000000, 0.000000000000000000 ) ) ;
#28483 = AXIS2_PLACEMENT_3D ( 'NONE', #25565, #31191, #28004 ) ;
#28484 = DIRECTION ( 'NONE',  ( 0.000000000000000000, 0.000000000000000000, 1.000000000000000000 ) ) ;
#28485 = ORIENTED_EDGE ( 'NONE', *, *, #31574, .T. ) ;
#28486 = ORIENTED_EDGE ( 'NONE', *, *, #32205, .T. ) ;
#28487 = AXIS2_PLACEMENT_3D ( 'NONE', #24527, #35772, #6882 ) ;
#28488 = AXIS2_PLACEMENT_3D ( 'NONE', #4890, #1702, #30574 ) ;
#28489 = ORIENTED_EDGE ( 'NONE', *, *, #36062, .F. ) ;
#28490 = CIRCLE ( 'NONE', #12306, 3.500000000000003109 ) ;
#28491 = AXIS2_PLACEMENT_3D ( 'NONE', #13577, #31361, #5348 ) ;
#28492 = EDGE_LOOP ( 'NONE', ( #4668, #5278, #21685, #15575 ) ) ;
#28493 = VECTOR ( 'NONE', #14756, 1000.000000000000000 ) ;
#28494 = ORIENTED_EDGE ( 'NONE', *, *, #2709, .F. ) ;
#28495 = DIRECTION ( 'NONE',  ( 0.000000000000000000, 0.000000000000000000, 1.000000000000000000 ) ) ;
#28496 = DIRECTION ( 'NONE',  ( 0.000000000000000000, 0.000000000000000000, 1.000000000000000000 ) ) ;
#28497 = CARTESIAN_POINT ( 'NONE',  ( -23.00000337463121980, -77.94228634059963667, -5.000000000000000000 ) ) ;
#28498 = AXIS2_PLACEMENT_3D ( 'NONE', #16430, #22420, #8183 ) ;
#28499 = CARTESIAN_POINT ( 'NONE',  ( 0.000000000000000000, 0.000000000000000000, 32.50000000000000000 ) ) ;
#28500 = CARTESIAN_POINT ( 'NONE',  ( -37.00000337463117717, -77.94228634059963667, 12.50000000000000000 ) ) ;
#28501 = EDGE_LOOP ( 'NONE', ( #473, #26498 ) ) ;
#28502 = CARTESIAN_POINT ( 'NONE',  ( -34.00000000000027711, -58.88972745734168512, -49.22241343995298024 ) ) ;
#28503 = CARTESIAN_POINT ( 'NONE',  ( -2.176667689905596337, -4.790324513057907296, -4.057749648769110706 ) ) ;
#28504 = EDGE_CURVE ( 'NONE', #19348, #29705, #36269, .T. ) ;
#28505 = DIRECTION ( 'NONE',  ( 0.000000000000000000, 0.000000000000000000, -1.000000000000000000 ) ) ;
#28506 = ORIENTED_EDGE ( 'NONE', *, *, #14441, .T. ) ;
#28507 = DIRECTION ( 'NONE',  ( 0.000000000000000000, 0.000000000000000000, -1.000000000000000000 ) ) ;
#28508 = DIRECTION ( 'NONE',  ( -0.000000000000000000, -0.000000000000000000, 1.000000000000000000 ) ) ;
#28509 = EDGE_LOOP ( 'NONE', ( #16578, #27789 ) ) ;
#28510 = CIRCLE ( 'NONE', #13523, 27.00000000000001421 ) ;
#28511 = ORIENTED_EDGE ( 'NONE', *, *, #14379, .T. ) ;
#28512 = DIRECTION ( 'NONE',  ( 0.000000000000000000, -0.8660254037844421493, -0.4999999999999942268 ) ) ;
#28513 = CARTESIAN_POINT ( 'NONE',  ( 67.99999662536836809, -34.64101615137759183, -9.999999999999998224 ) ) ;
#28514 = DIRECTION ( 'NONE',  ( 1.000000000000000000, 0.000000000000000000, 0.000000000000000000 ) ) ;
#28515 = LINE ( 'NONE', #8833, #1717 ) ;
#28516 = AXIS2_PLACEMENT_3D ( 'NONE', #2766, #14002, #11390 ) ;
#28517 = ORIENTED_EDGE ( 'NONE', *, *, #22172, .F. ) ;
#28518 = ORIENTED_EDGE ( 'NONE', *, *, #30448, .T. ) ;
#28519 = AXIS2_PLACEMENT_3D ( 'NONE', #14330, #72, #31554 ) ;
#28520 = CONICAL_SURFACE ( 'NONE', #983, 20.00000000000001066, 0.1396263401595466691 ) ;
#28521 = VECTOR ( 'NONE', #29262, 1000.000000000000000 ) ;
#28522 = FACE_OUTER_BOUND ( 'NONE', #8151, .T. ) ;
#28523 = AXIS2_PLACEMENT_3D ( 'NONE', #25179, #22522, #16731 ) ;
#28524 = FACE_OUTER_BOUND ( 'NONE', #8310, .T. ) ;
#28525 = ORIENTED_EDGE ( 'NONE', *, *, #34940, .F. ) ;
#28526 = DIRECTION ( 'NONE',  ( 0.000000000000000000, 0.000000000000000000, -1.000000000000000000 ) ) ;
#28527 = ORIENTED_EDGE ( 'NONE', *, *, #35635, .T. ) ;
#28528 = ADVANCED_FACE ( 'NONE', ( #30658 ), #36498, .F. ) ;
#28529 = EDGE_CURVE ( 'NONE', #28159, #20602, #13958, .T. ) ;
#28530 = ORIENTED_EDGE ( 'NONE', *, *, #19696, .T. ) ;
#28531 = AXIS2_PLACEMENT_3D ( 'NONE', #25788, #5706, #11508 ) ;
#28532 = CARTESIAN_POINT ( 'NONE',  ( 84.88770958243756581, -10.65709945499358824, -5.000000000000000000 ) ) ;
#28533 = FACE_OUTER_BOUND ( 'NONE', #18296, .T. ) ;
#28534 = CARTESIAN_POINT ( 'NONE',  ( 3.000000000000000000, 2.935248768560057453, -3.903127820947815962E-15 ) ) ;
#28535 = ORIENTED_EDGE ( 'NONE', *, *, #8137, .F. ) ;
#28536 = ORIENTED_EDGE ( 'NONE', *, *, #800, .T. ) ;
#28537 = DIRECTION ( 'NONE',  ( 0.000000000000000000, 0.000000000000000000, 1.000000000000000000 ) ) ;
#28538 = DIRECTION ( 'NONE',  ( -0.000000000000000000, -0.000000000000000000, 1.000000000000000000 ) ) ;
#28539 = AXIS2_PLACEMENT_3D ( 'NONE', #4578, #16019, #10375 ) ;
#28540 = DIRECTION ( 'NONE',  ( 0.000000000000000000, 0.000000000000000000, 1.000000000000000000 ) ) ;
#28541 = DIRECTION ( 'NONE',  ( 0.000000000000000000, 0.000000000000000000, -1.000000000000000000 ) ) ;
#28542 = EDGE_CURVE ( 'NONE', #13878, #28166, #8711, .T. ) ;
#28543 = CIRCLE ( 'NONE', #32115, 2.000000000000001776 ) ;
#28544 = VERTEX_POINT ( 'NONE', #25795 ) ;
#28545 = CARTESIAN_POINT ( 'NONE',  ( 3.866666666667000651, 0.000000000000000000, 2.266666666667000563 ) ) ;
#28546 = FACE_BOUND ( 'NONE', #31969, .T. ) ;
#28547 = CYLINDRICAL_SURFACE ( 'NONE', #21990, 2.000000000000001776 ) ;
#28548 = DIRECTION ( 'NONE',  ( -0.000000000000000000, -0.000000000000000000, -1.000000000000000000 ) ) ;
#28549 = CARTESIAN_POINT ( 'NONE',  ( -82.00000337463094979, -2.404119930384582903E-14, -5.000000000000000000 ) ) ;
#28550 = CARTESIAN_POINT ( 'NONE',  ( -34.00000000000027711, -58.88972745734168512, 12.49999999999999822 ) ) ;
#28551 = VECTOR ( 'NONE', #14277, 1000.000000000000000 ) ;
#28552 = CIRCLE ( 'NONE', #30377, 2.000000000000001776 ) ;
#28553 = LINE ( 'NONE', #14113, #22175 ) ;
#28554 = EDGE_CURVE ( 'NONE', #32213, #16797, #28587, .T. ) ;
#28555 = DIRECTION ( 'NONE',  ( 0.000000000000000000, 0.000000000000000000, 1.000000000000000000 ) ) ;
#28556 = VERTEX_POINT ( 'NONE', #33671 ) ;
#28557 = CARTESIAN_POINT ( 'NONE',  ( 0.000000000000000000, -2.935248768560059229, 3.469446951953614189E-15 ) ) ;
#28558 = CARTESIAN_POINT ( 'NONE',  ( 54.99999662536844625, -60.62177826491080168, -9.999999999999998224 ) ) ;
#28559 = CARTESIAN_POINT ( 'NONE',  ( -40.00000337463113453, -69.28203230275519786, -9.999999999999998224 ) ) ;
#28560 = ORIENTED_EDGE ( 'NONE', *, *, #5342, .T. ) ;
#28561 = CIRCLE ( 'NONE', #27976, 27.00000000000001421 ) ;
#28562 = ORIENTED_EDGE ( 'NONE', *, *, #33351, .F. ) ;
#28563 = ORIENTED_EDGE ( 'NONE', *, *, #23329, .F. ) ;
#28564 = LINE ( 'NONE', #5150, #30317 ) ;
#28565 = CARTESIAN_POINT ( 'NONE',  ( -70.00000337463099243, 34.64101615137758472, 17.49999999999999645 ) ) ;
#28566 = CARTESIAN_POINT ( 'NONE',  ( -75.00000337463100664, -43.30127018922202353, -9.999999999999998224 ) ) ;
#28567 = ORIENTED_EDGE ( 'NONE', *, *, #11218, .F. ) ;
#28568 = AXIS2_PLACEMENT_3D ( 'NONE', #30626, #27802, #16766 ) ;
#28569 = CIRCLE ( 'NONE', #35178, 65.00000000000000000 ) ;
#28570 = DIRECTION ( 'NONE',  ( 0.000000000000000000, 0.000000000000000000, 1.000000000000000000 ) ) ;
#28571 = AXIS2_PLACEMENT_3D ( 'NONE', #32514, #35377, #24266 ) ;
#28572 = ORIENTED_EDGE ( 'NONE', *, *, #32538, .T. ) ;
#28573 = EDGE_CURVE ( 'NONE', #29660, #7478, #27839, .T. ) ;
#28574 = CARTESIAN_POINT ( 'NONE',  ( -101.4252494179839488, 31.43181965331819683, 32.50001250000000397 ) ) ;
#28575 = EDGE_LOOP ( 'NONE', ( #5566, #16447, #6830, #21071 ) ) ;
#28576 = DIRECTION ( 'NONE',  ( 1.000000000000000000, 0.000000000000000000, 0.000000000000000000 ) ) ;
#28577 = VERTEX_POINT ( 'NONE', #22055 ) ;
#28578 = AXIS2_PLACEMENT_3D ( 'NONE', #2916, #3092, #11880 ) ;
#28579 = VERTEX_POINT ( 'NONE', #33496 ) ;
#28580 = AXIS2_PLACEMENT_3D ( 'NONE', #9806, #21630, #1752 ) ;
#28581 = CARTESIAN_POINT ( 'NONE',  ( -62.00000337463108480, -51.96152422706641971, 12.50000000000000000 ) ) ;
#28582 = LINE ( 'NONE', #22960, #3460 ) ;
#28583 = CARTESIAN_POINT ( 'NONE',  ( -0.1702248550645419911, 5.871782057790544407, -4.289066185948687604 ) ) ;
#28584 =( REPRESENTATION_RELATIONSHIP ('NONE','NONE', #15268, #6396 ) REPRESENTATION_RELATIONSHIP_WITH_TRANSFORMATION ( #33102 )SHAPE_REPRESENTATION_RELATIONSHIP( ) );
#28585 = EDGE_CURVE ( 'NONE', #7967, #625, #4976, .T. ) ;
#28586 = EDGE_LOOP ( 'NONE', ( #36145, #22532 ) ) ;
#28587 = LINE ( 'NONE', #31217, #9293 ) ;
#28588 = CONTEXT_DEPENDENT_SHAPE_REPRESENTATION ( #18287, #12763 ) ;
#28589 = CARTESIAN_POINT ( 'NONE',  ( 70.80619744048946984, -84.18124734178287838, 32.50000000000000000 ) ) ;
#28590 = LINE ( 'NONE', #22969, #34939 ) ;
#28591 = EDGE_CURVE ( 'NONE', #7201, #4684, #2126, .T. ) ;
#28592 = EDGE_LOOP ( 'NONE', ( #24173, #1735, #36673, #17422 ) ) ;
#28593 = DIRECTION ( 'NONE',  ( -1.000000000000000000, 5.268419445559189404E-15, 0.000000000000000000 ) ) ;
#28595 = DIRECTION ( 'NONE',  ( -1.000000000000000000, 0.000000000000000000, 0.000000000000000000 ) ) ;
#28594 = CIRCLE ( 'NONE', #9434, 2.000000000000001776 ) ;
#28596 = ORIENTED_EDGE ( 'NONE', *, *, #7828, .T. ) ;
#28597 = DIRECTION ( 'NONE',  ( 0.000000000000000000, 0.000000000000000000, -1.000000000000000000 ) ) ;
#28598 = CIRCLE ( 'NONE', #12417, 1.999999999999998224 ) ;
#28599 = AXIS2_PLACEMENT_3D ( 'NONE', #34015, #19022, #13561 ) ;
#28600 = DIRECTION ( 'NONE',  ( 0.000000000000000000, 0.000000000000000000, 1.000000000000000000 ) ) ;
#28601 = DIRECTION ( 'NONE',  ( 0.000000000000000000, 0.000000000000000000, -1.000000000000000000 ) ) ;
#28603 = CIRCLE ( 'NONE', #13615, 2.000000000000001776 ) ;
#28602 = DIRECTION ( 'NONE',  ( 0.000000000000000000, 0.000000000000000000, 1.000000000000000000 ) ) ;
#28604 = ORIENTED_EDGE ( 'NONE', *, *, #15853, .F. ) ;
#28605 = VECTOR ( 'NONE', #10345, 1000.000000000000000 ) ;
#28606 = EDGE_LOOP ( 'NONE', ( #20018, #19194, #618, #18414 ) ) ;
#28607 = CARTESIAN_POINT ( 'NONE',  ( 1.647413659512552364, -4.822367972110057188, -0.05822226285685519476 ) ) ;
#28608 = DIRECTION ( 'NONE',  ( 0.000000000000000000, 0.000000000000000000, -1.000000000000000000 ) ) ;
#28609 = AXIS2_PLACEMENT_3D ( 'NONE', #19485, #11412, #34289 ) ;
#28610 = EDGE_CURVE ( 'NONE', #4355, #11389, #5107, .T. ) ;
#28611 = ORIENTED_EDGE ( 'NONE', *, *, #28810, .F. ) ;
#28612 = ORIENTED_EDGE ( 'NONE', *, *, #6917, .F. ) ;
#28613 = CYLINDRICAL_SURFACE ( 'NONE', #20829, 2.000000000000000000 ) ;
#28614 = LINE ( 'NONE', #2563, #18252 ) ;
#28615 = CIRCLE ( 'NONE', #34631, 6.000000000000005329 ) ;
#28616 = EDGE_CURVE ( 'NONE', #26529, #23686, #28037, .T. ) ;
#28617 = ORIENTED_EDGE ( 'NONE', *, *, #22045, .F. ) ;
#28618 = VECTOR ( 'NONE', #35848, 1000.000000000000000 ) ;
#28619 = CARTESIAN_POINT ( 'NONE',  ( -33.00000337463117006, -77.94228634059963667, 12.50000000000000000 ) ) ;
#28620 = ORIENTED_EDGE ( 'NONE', *, *, #24885, .T. ) ;
#28621 = EDGE_CURVE ( 'NONE', #22736, #5071, #30835, .T. ) ;
#28622 = CARTESIAN_POINT ( 'NONE',  ( 0.000000000000000000, 0.000000000000000000, 13.31572692736085095 ) ) ;
#28623 = ORIENTED_EDGE ( 'NONE', *, *, #29944, .F. ) ;
#28624 = VECTOR ( 'NONE', #34751, 1000.000000000000000 ) ;
#28625 = CYLINDRICAL_SURFACE ( 'NONE', #31492, 2.000000000000001776 ) ;
#28626 = VECTOR ( 'NONE', #22109, 1000.000000000000000 ) ;
#28627 = AXIS2_PLACEMENT_3D ( 'NONE', #34887, #11806, #18178 ) ;
#28628 = LINE ( 'NONE', #25445, #19134 ) ;
#28629 = PLANE ( 'NONE',  #21490 ) ;
#28630 = VERTEX_POINT ( 'NONE', #25237 ) ;
#28631 = CARTESIAN_POINT ( 'NONE',  ( 108.3061974404897825, -19.22934205795014151, 38.50000000000000711 ) ) ;
#28632 = CARTESIAN_POINT ( 'NONE',  ( -46.00000000000000000, 103.4105893997321886, 27.49999999999999645 ) ) ;
#28633 = AXIS2_PLACEMENT_3D ( 'NONE', #28462, #8042, #25681 ) ;
#28634 = ADVANCED_FACE ( 'NONE', ( #10962 ), #14148, .F. ) ;
#28635 = DIRECTION ( 'NONE',  ( 0.000000000000000000, -0.000000000000000000, -1.000000000000000000 ) ) ;
#28636 = LINE ( 'NONE', #26199, #29909 ) ;
#28637 = ORIENTED_EDGE ( 'NONE', *, *, #16743, .T. ) ;
#28638 = CARTESIAN_POINT ( 'NONE',  ( -18.00000337463123756, -86.60254037844400443, 12.50000000000000000 ) ) ;
#28639 = FACE_OUTER_BOUND ( 'NONE', #33629, .T. ) ;
#28640 = CIRCLE ( 'NONE', #8291, 2.000000000000001776 ) ;
#28641 = CARTESIAN_POINT ( 'NONE',  ( 0.000000000000000000, 0.000000000000000000, -5.324496230895142901 ) ) ;
#28642 = VERTEX_POINT ( 'NONE', #10575 ) ;
#28643 = ORIENTED_EDGE ( 'NONE', *, *, #33709, .F. ) ;
#28644 = AXIS2_PLACEMENT_3D ( 'NONE', #19507, #36585, #36401 ) ;
#28645 = ORIENTED_EDGE ( 'NONE', *, *, #31170, .F. ) ;
#28646 = CIRCLE ( 'NONE', #31037, 2.000000000000001776 ) ;
#28647 = AXIS2_PLACEMENT_3D ( 'NONE', #10973, #36509, #33509 ) ;
#28648 = DIRECTION ( 'NONE',  ( 0.000000000000000000, 0.000000000000000000, 1.000000000000000000 ) ) ;
#28649 = EDGE_CURVE ( 'NONE', #24286, #17057, #27253, .T. ) ;
#28650 = AXIS2_PLACEMENT_3D ( 'NONE', #20395, #6703, #15321 ) ;
#28651 = LINE ( 'NONE', #8237, #18861 ) ;
#28652 = CARTESIAN_POINT ( 'NONE',  ( 90.51363901676214141, -71.13863674840979456, 32.50000000000000711 ) ) ;
#28653 = LINE ( 'NONE', #23218, #5143 ) ;
#28654 = EDGE_CURVE ( 'NONE', #36932, #30829, #18892, .T. ) ;
#28655 = DIRECTION ( 'NONE',  ( 1.000000000000000000, -1.850371707708594366E-15, 0.000000000000000000 ) ) ;
#28657 = AXIS2_PLACEMENT_3D ( 'NONE', #23275, #17287, #3393 ) ;
#28656 = CARTESIAN_POINT ( 'NONE',  ( -50.00000337463110611, -69.28203230275519786, -9.999999999999998224 ) ) ;
#28658 = ORIENTED_EDGE ( 'NONE', *, *, #27648, .T. ) ;
#28659 = EDGE_CURVE ( 'NONE', #2842, #15693, #36458, .T. ) ;
#28660 = EDGE_LOOP ( 'NONE', ( #3791, #34465, #13242, #22758 ) ) ;
#28661 = AXIS2_PLACEMENT_3D ( 'NONE', #33248, #27797, #1762 ) ;
#28662 = CARTESIAN_POINT ( 'NONE',  ( -31.74999999999995737, 0.000000000000000000, 5.000000000000000000 ) ) ;
#28663 = CYLINDRICAL_SURFACE ( 'NONE', #20535, 2.500000000000000000 ) ;
#28664 = FACE_OUTER_BOUND ( 'NONE', #22358, .T. ) ;
#28665 = CARTESIAN_POINT ( 'NONE',  ( 62.99999662536839651, -60.62177826491080168, -5.000000000000000000 ) ) ;
#28666 = EDGE_CURVE ( 'NONE', #22278, #6597, #30252, .T. ) ;
#28667 = ORIENTED_EDGE ( 'NONE', *, *, #32722, .T. ) ;
#28668 = UNCERTAINTY_MEASURE_WITH_UNIT (LENGTH_MEASURE( 1.000000000000000082E-05 ), #25495, 'distance_accuracy_value', 'NONE');
#28669 = ADVANCED_FACE ( 'NONE', ( #2123 ), #13207, .F. ) ;
#28670 = FACE_BOUND ( 'NONE', #5005, .T. ) ;
#28671 = VECTOR ( 'NONE', #33147, 1000.000000000000000 ) ;
#28672 = VERTEX_POINT ( 'NONE', #36263 ) ;
#28673 = ORIENTED_EDGE ( 'NONE', *, *, #36193, .T. ) ;
#28674 = CIRCLE ( 'NONE', #19120, 1.999999999999998224 ) ;
#28675 = CARTESIAN_POINT ( 'NONE',  ( -48.00000337463109190, 51.96152422706637708, -9.999999999999998224 ) ) ;
#28676 = EDGE_LOOP ( 'NONE', ( #23852, #5359, #34569, #8570 ) ) ;
#28677 = EDGE_CURVE ( 'NONE', #24850, #34867, #6321, .T. ) ;
#28678 = EDGE_CURVE ( 'NONE', #14243, #2055, #21913, .T. ) ;
#28679 = CARTESIAN_POINT ( 'NONE',  ( 84.99999662536832545, 8.660254037844394404, -9.999999999999998224 ) ) ;
#28680 = ADVANCED_FACE ( 'NONE', ( #10767 ), #35713, .F. ) ;
#28681 = FACE_OUTER_BOUND ( 'NONE', #19690, .T. ) ;
#28682 = EDGE_CURVE ( 'NONE', #5583, #8974, #21290, .T. ) ;
#28683 = ORIENTED_EDGE ( 'NONE', *, *, #4256, .F. ) ;
#28684 = EDGE_CURVE ( 'NONE', #8353, #13437, #30285, .T. ) ;
#28685 = ORIENTED_EDGE ( 'NONE', *, *, #1156, .F. ) ;
#28686 = AXIS2_PLACEMENT_3D ( 'NONE', #3720, #712, #34849 ) ;
#28687 = EDGE_LOOP ( 'NONE', ( #21722, #6103, #36835, #18617 ) ) ;
#28688 = VERTEX_POINT ( 'NONE', #7772 ) ;
#28689 = AXIS2_PLACEMENT_3D ( 'NONE', #36886, #28429, #31621 ) ;
#28690 = ORIENTED_EDGE ( 'NONE', *, *, #26092, .T. ) ;
#28691 = DIRECTION ( 'NONE',  ( 0.000000000000000000, 0.000000000000000000, 1.000000000000000000 ) ) ;
#28693 = DIRECTION ( 'NONE',  ( 0.000000000000000000, 0.000000000000000000, 1.000000000000000000 ) ) ;
#28692 = CIRCLE ( 'NONE', #11927, 3.000000000000002665 ) ;
#28694 = DIRECTION ( 'NONE',  ( 1.000000000000000000, 0.000000000000000000, 0.000000000000000000 ) ) ;
#28695 = CARTESIAN_POINT ( 'NONE',  ( -68.00000337463099243, 51.96152422706637708, -5.000000000000000000 ) ) ;
#28696 = DIRECTION ( 'NONE',  ( 0.000000000000000000, 0.000000000000000000, -1.000000000000000000 ) ) ;
#28697 = ORIENTED_EDGE ( 'NONE', *, *, #15761, .T. ) ;
#28698 = DIRECTION ( 'NONE',  ( -1.000000000000000000, 0.000000000000000000, 0.000000000000000000 ) ) ;
#28699 = CARTESIAN_POINT ( 'NONE',  ( 0.000000000000000000, 0.000000000000000000, 5.000000000000000000 ) ) ;
#28700 = AXIS2_PLACEMENT_3D ( 'NONE', #24764, #33014, #24961 ) ;
#28701 = AXIS2_PLACEMENT_3D ( 'NONE', #31439, #5769, #14751 ) ;
#28702 = CARTESIAN_POINT ( 'NONE',  ( 54.99999662536846046, -43.30127018922200222, -9.999999999999998224 ) ) ;
#28703 = ORIENTED_EDGE ( 'NONE', *, *, #9371, .F. ) ;
#28704 = CARTESIAN_POINT ( 'NONE',  ( 67.99999662536838230, 17.32050807568879236, -9.999999999999998224 ) ) ;
#28705 = AXIS2_PLACEMENT_3D ( 'NONE', #31180, #14099, #19560 ) ;
#28706 = CARTESIAN_POINT ( 'NONE',  ( -45.00000337463111322, 60.62177826491077326, 17.49999999999999645 ) ) ;
#28707 = ORIENTED_EDGE ( 'NONE', *, *, #3713, .T. ) ;
#28708 = VERTEX_POINT ( 'NONE', #4779 ) ;
#28709 = CARTESIAN_POINT ( 'NONE',  ( 84.99999662536831124, -25.98076211353319565, -9.999999999999998224 ) ) ;
#28710 = CARTESIAN_POINT ( 'NONE',  ( -30.00000337463119848, -69.28203230275522628, -9.999999999999998224 ) ) ;
#28711 = LINE ( 'NONE', #2649, #8000 ) ;
#28712 = PLANE ( 'NONE',  #5315 ) ;
#28713 = ORIENTED_EDGE ( 'NONE', *, *, #18273, .T. ) ;
#28714 = EDGE_LOOP ( 'NONE', ( #28802, #11574 ) ) ;
#28715 = CIRCLE ( 'NONE', #14942, 2.000000000000001776 ) ;
#28716 = FACE_OUTER_BOUND ( 'NONE', #36033, .T. ) ;
#28717 = DIRECTION ( 'NONE',  ( -1.000000000000000000, 0.000000000000000000, 0.000000000000000000 ) ) ;
#28718 = FACE_BOUND ( 'NONE', #3154, .T. ) ;
#28719 = AXIS2_PLACEMENT_3D ( 'NONE', #19241, #30654, #27834 ) ;
#28720 = ORIENTED_EDGE ( 'NONE', *, *, #1873, .T. ) ;
#28721 = ADVANCED_FACE ( 'NONE', ( #30628 ), #4945, .F. ) ;
#28722 = FACE_OUTER_BOUND ( 'NONE', #3998, .T. ) ;
#28723 = CIRCLE ( 'NONE', #7190, 2.000000000000001776 ) ;
#28724 = ORIENTED_EDGE ( 'NONE', *, *, #21186, .T. ) ;
#28725 = ORIENTED_EDGE ( 'NONE', *, *, #32842, .F. ) ;
#28726 = CYLINDRICAL_SURFACE ( 'NONE', #18804, 2.000000000000001776 ) ;
#28727 = AXIS2_PLACEMENT_3D ( 'NONE', #9468, #24607, #651 ) ;
#28728 = DIRECTION ( 'NONE',  ( 1.000000000000000000, 0.000000000000000000, 0.000000000000000000 ) ) ;
#28729 = EDGE_CURVE ( 'NONE', #30923, #4610, #4585, .T. ) ;
#28730 = ORIENTED_EDGE ( 'NONE', *, *, #24997, .F. ) ;
#28731 = VERTEX_POINT ( 'NONE', #21814 ) ;
#28732 = VECTOR ( 'NONE', #20009, 1000.000000000000000 ) ;
#28733 = LINE ( 'NONE', #22755, #15485 ) ;
#28734 = DIRECTION ( 'NONE',  ( 0.000000000000000000, 0.000000000000000000, 1.000000000000000000 ) ) ;
#28735 = DIRECTION ( 'NONE',  ( 0.000000000000000000, 0.000000000000000000, 1.000000000000000000 ) ) ;
#28736 = ORIENTED_EDGE ( 'NONE', *, *, #3430, .T. ) ;
#28737 = DIRECTION ( 'NONE',  ( 0.000000000000000000, 0.000000000000000000, 1.000000000000000000 ) ) ;
#28738 = FACE_BOUND ( 'NONE', #4554, .T. ) ;
#28739 = DIRECTION ( 'NONE',  ( 0.000000000000000000, 0.000000000000000000, 1.000000000000000000 ) ) ;
#28740 = CARTESIAN_POINT ( 'NONE',  ( 42.99999662536848888, 60.62177826491077326, -5.000000000000000000 ) ) ;
#28741 = CARTESIAN_POINT ( 'NONE',  ( 1.999996625368710257, -69.28203230275519786, 12.50000000000000000 ) ) ;
#28742 = AXIS2_PLACEMENT_3D ( 'NONE', #12215, #17503, #15239 ) ;
#28743 = DIRECTION ( 'NONE',  ( -1.000000000000000000, 0.000000000000000000, 0.000000000000000000 ) ) ;
#28744 = DIRECTION ( 'NONE',  ( 1.000000000000000000, 0.000000000000000000, 0.000000000000000000 ) ) ;
#28745 = AXIS2_PLACEMENT_3D ( 'NONE', #22206, #8129, #19577 ) ;
#28746 = LINE ( 'NONE', #20308, #16366 ) ;
#28747 = ORIENTED_EDGE ( 'NONE', *, *, #1281, .T. ) ;
#28748 = CARTESIAN_POINT ( 'NONE',  ( 9.999996625368618552, 69.28203230275516944, -5.000000000000000000 ) ) ;
#28749 = CARTESIAN_POINT ( 'NONE',  ( -2.179555516819077443, 4.788648424347429433, -4.057628883416041887 ) ) ;
#28750 = CIRCLE ( 'NONE', #35971, 45.00000000000000711 ) ;
#28751 = CARTESIAN_POINT ( 'NONE',  ( 84.99999662536831124, -8.660254037844397956, 12.50000000000000000 ) ) ;
#28752 = ADVANCED_FACE ( 'NONE', ( #22204 ), #16215, .T. ) ;
#28753 = EDGE_LOOP ( 'NONE', ( #30321, #23973, #8530, #28463 ) ) ;
#28754 = ORIENTED_EDGE ( 'NONE', *, *, #28901, .T. ) ;
#28755 = ORIENTED_EDGE ( 'NONE', *, *, #28385, .T. ) ;
#28756 = DIRECTION ( 'NONE',  ( 0.000000000000000000, 0.000000000000000000, -1.000000000000000000 ) ) ;
#28757 = CARTESIAN_POINT ( 'NONE',  ( -45.00000337463111322, 77.94228634059959404, 17.49999999999999645 ) ) ;
#28758 = DIRECTION ( 'NONE',  ( 0.000000000000000000, 0.000000000000000000, -1.000000000000000000 ) ) ;
#28759 = VERTEX_POINT ( 'NONE', #10380 ) ;
#28760 = DIRECTION ( 'NONE',  ( -0.4999999999999968359, 0.8660254037844404840, 0.000000000000000000 ) ) ;
#28761 = ORIENTED_EDGE ( 'NONE', *, *, #11468, .F. ) ;
#28762 = VECTOR ( 'NONE', #12598, 1000.000000000000000 ) ;
#28763 = DIRECTION ( 'NONE',  ( -1.000000000000000000, 0.000000000000000000, 0.000000000000000000 ) ) ;
#28764 = VERTEX_POINT ( 'NONE', #1771 ) ;
#28765 = DIRECTION ( 'NONE',  ( 0.000000000000000000, 0.000000000000000000, -1.000000000000000000 ) ) ;
#28766 = VERTEX_POINT ( 'NONE', #27631 ) ;
#28767 = ORIENTED_EDGE ( 'NONE', *, *, #8246, .F. ) ;
#28768 = DIRECTION ( 'NONE',  ( 0.000000000000000000, 0.000000000000000000, 1.000000000000000000 ) ) ;
#28769 = FACE_OUTER_BOUND ( 'NONE', #33540, .T. ) ;
#28771 = AXIS2_PLACEMENT_3D ( 'NONE', #2469, #13890, #19175 ) ;
#28770 = CARTESIAN_POINT ( 'NONE',  ( 34.99999662536855283, 60.62177826491078747, 12.50000000000000000 ) ) ;
#28772 = EDGE_CURVE ( 'NONE', #4318, #24271, #35674, .T. ) ;
#28773 = EDGE_LOOP ( 'NONE', ( #6691, #9768, #36796, #31410 ) ) ;
#28774 = CYLINDRICAL_SURFACE ( 'NONE', #8327, 2.000000000000001776 ) ;
#28775 = CARTESIAN_POINT ( 'NONE',  ( 82.99999662536831124, -25.98076211353319565, -9.999999999999998224 ) ) ;
#28776 = CARTESIAN_POINT ( 'NONE',  ( -33.00000337463116296, -60.62177826491080168, 12.50000000000000000 ) ) ;
#28777 = ORIENTED_EDGE ( 'NONE', *, *, #26189, .T. ) ;
#28778 = FACE_OUTER_BOUND ( 'NONE', #19202, .T. ) ;
#28779 = LINE ( 'NONE', #11699, #16784 ) ;
#28780 = EDGE_LOOP ( 'NONE', ( #25407, #7544 ) ) ;
#28781 = DIRECTION ( 'NONE',  ( 1.000000000000000000, 0.000000000000000000, 0.000000000000000000 ) ) ;
#28782 = CYLINDRICAL_SURFACE ( 'NONE', #4632, 2.000000000000001776 ) ;
#28783 = DIRECTION ( 'NONE',  ( 1.000000000000000000, 0.000000000000000000, 0.000000000000000000 ) ) ;
#28784 = CARTESIAN_POINT ( 'NONE',  ( 102.5304832720496080, 102.5304832720492527, 27.50000000000000000 ) ) ;
#28785 = CARTESIAN_POINT ( 'NONE',  ( -68.00000000000000000, 0.000000000000000000, 12.49999999999999822 ) ) ;
#28786 = ADVANCED_FACE ( 'NONE', ( #15650 ), #24651, .F. ) ;
#28787 = EDGE_LOOP ( 'NONE', ( #17018, #30565, #26022, #31301, #7702, #4265, #13975, #15292, #35556, #32925, #22451, #4594, #17178 ) ) ;
#28788 = CARTESIAN_POINT ( 'NONE',  ( 52.39915983220795681, 35.19434990244919703, -4.999999999999997335 ) ) ;
#28789 = DIRECTION ( 'NONE',  ( 0.000000000000000000, 0.000000000000000000, 1.000000000000000000 ) ) ;
#28790 = EDGE_CURVE ( 'NONE', #35117, #13323, #27282, .T. ) ;
#28791 = VERTEX_POINT ( 'NONE', #28549 ) ;
#28792 = ORIENTED_EDGE ( 'NONE', *, *, #30263, .T. ) ;
#28793 = ORIENTED_EDGE ( 'NONE', *, *, #23802, .T. ) ;
#28794 = AXIS2_PLACEMENT_3D ( 'NONE', #13672, #2428, #10478 ) ;
#28795 = DIRECTION ( 'NONE',  ( 0.000000000000000000, 0.000000000000000000, 1.000000000000000000 ) ) ;
#28796 = EDGE_CURVE ( 'NONE', #9908, #3457, #11115, .T. ) ;
#28797 = CARTESIAN_POINT ( 'NONE',  ( 55.27226924886129211, 77.26562141134560591, 27.50000000000000000 ) ) ;
#28798 = EDGE_CURVE ( 'NONE', #33601, #24245, #22931, .T. ) ;
#28799 = DIRECTION ( 'NONE',  ( -0.000000000000000000, -0.000000000000000000, 1.000000000000000000 ) ) ;
#28800 = ORIENTED_EDGE ( 'NONE', *, *, #32563, .F. ) ;
#28801 = CARTESIAN_POINT ( 'NONE',  ( -45.00000337463111322, 77.94228634059959404, -9.999999999999998224 ) ) ;
#28802 = ORIENTED_EDGE ( 'NONE', *, *, #18079, .F. ) ;
#28803 = FACE_BOUND ( 'NONE', #9839, .T. ) ;
#28804 = CARTESIAN_POINT ( 'NONE',  ( 56.67878100130369035, -27.78182860042797131, -4.999999999999997335 ) ) ;
#28805 = CARTESIAN_POINT ( 'NONE',  ( -42.00000337463114164, 69.28203230275516944, -9.999999999999998224 ) ) ;
#28806 = CARTESIAN_POINT ( 'NONE',  ( 87.99999662536828282, 2.449293598294706414E-16, -9.999999999999998224 ) ) ;
#28807 = AXIS2_PLACEMENT_3D ( 'NONE', #6581, #30003, #30569 ) ;
#28808 = CARTESIAN_POINT ( 'NONE',  ( 37.50000000000000000, 103.4105893997321743, 38.50000000000000000 ) ) ;
#28809 = DIRECTION ( 'NONE',  ( 0.000000000000000000, 0.000000000000000000, 1.000000000000000000 ) ) ;
#28810 = EDGE_CURVE ( 'NONE', #36526, #17340, #32689, .T. ) ;
#28811 = CARTESIAN_POINT ( 'NONE',  ( -4.279621169095561228, 62.97617850287782915, 12.49999999999999822 ) ) ;
#28812 = DIRECTION ( 'NONE',  ( 1.000000000000000000, 0.000000000000000000, 0.000000000000000000 ) ) ;
#28813 = EDGE_LOOP ( 'NONE', ( #25646, #25162, #32419, #16276 ) ) ;
#28814 = DIRECTION ( 'NONE',  ( 0.000000000000000000, 0.000000000000000000, 1.000000000000000000 ) ) ;
#28815 = DIRECTION ( 'NONE',  ( -0.000000000000000000, 0.000000000000000000, 1.000000000000000000 ) ) ;
#28816 = DIRECTION ( 'NONE',  ( 0.000000000000000000, 0.000000000000000000, 1.000000000000000000 ) ) ;
#28817 = ADVANCED_FACE ( 'NONE', ( #25924 ), #25763, .T. ) ;
#28818 = VERTEX_POINT ( 'NONE', #5879 ) ;
#28819 = VERTEX_POINT ( 'NONE', #221 ) ;
#28820 = EDGE_CURVE ( 'NONE', #26898, #4119, #11696, .T. ) ;
#28821 = ORIENTED_EDGE ( 'NONE', *, *, #5191, .T. ) ;
#28822 = DIRECTION ( 'NONE',  ( 1.000000000000000000, 0.000000000000000000, 0.000000000000000000 ) ) ;
#28823 = AXIS2_PLACEMENT_3D ( 'NONE', #7209, #9813, #21068 ) ;
#28824 = CARTESIAN_POINT ( 'NONE',  ( 0.000000000000000000, 0.000000000000000000, -6.000000000000000000 ) ) ;
#28825 = CARTESIAN_POINT ( 'NONE',  ( 79.99999662536833966, 34.64101615137759183, -9.999999999999998224 ) ) ;
#28826 = CIRCLE ( 'NONE', #27043, 2.000000000000001776 ) ;
#28827 = DIRECTION ( 'NONE',  ( 1.000000000000000000, 0.000000000000000000, 0.000000000000000000 ) ) ;
#28828 = DIRECTION ( 'NONE',  ( 1.000000000000000000, 0.000000000000000000, 0.000000000000000000 ) ) ;
#28829 = VERTEX_POINT ( 'NONE', #34368 ) ;
#28830 = ORIENTED_EDGE ( 'NONE', *, *, #16688, .T. ) ;
#28831 = CARTESIAN_POINT ( 'NONE',  ( -51.13139720814437084, -27.49999999999955591, -10.00000000000000178 ) ) ;
#28832 = EDGE_CURVE ( 'NONE', #19362, #13179, #18320, .T. ) ;
#28833 = DIRECTION ( 'NONE',  ( 0.000000000000000000, 0.000000000000000000, -1.000000000000000000 ) ) ;
#28834 = DIRECTION ( 'NONE',  ( 0.000000000000000000, 0.000000000000000000, 1.000000000000000000 ) ) ;
#28835 = EDGE_LOOP ( 'NONE', ( #36184, #31316 ) ) ;
#28836 = FACE_BOUND ( 'NONE', #1832, .T. ) ;
#28837 = EDGE_LOOP ( 'NONE', ( #5714, #35750 ) ) ;
#28838 = ORIENTED_EDGE ( 'NONE', *, *, #22097, .F. ) ;
#28839 = DIRECTION ( 'NONE',  ( 1.000000000000000000, 0.000000000000000000, 0.000000000000000000 ) ) ;
#28840 = EDGE_LOOP ( 'NONE', ( #34291, #7585, #2490, #13084, #8471 ) ) ;
#28841 = DIRECTION ( 'NONE',  ( 0.000000000000000000, 0.000000000000000000, -1.000000000000000000 ) ) ;
#28842 = EDGE_CURVE ( 'NONE', #28991, #35130, #9913, .T. ) ;
#28843 = AXIS2_PLACEMENT_3D ( 'NONE', #28187, #34016, #20109 ) ;
#28844 = DIRECTION ( 'NONE',  ( 0.000000000000000000, 0.000000000000000000, 1.000000000000000000 ) ) ;
#28845 = EDGE_LOOP ( 'NONE', ( #12319, #13856, #27710, #6039 ) ) ;
#28846 = EDGE_CURVE ( 'NONE', #16912, #15905, #5337, .T. ) ;
#28847 = VERTEX_POINT ( 'NONE', #8670 ) ;
#28848 = ORIENTED_EDGE ( 'NONE', *, *, #22290, .T. ) ;
#28849 = ADVANCED_FACE ( 'NONE', ( #28188 ), #25211, .T. ) ;
#28850 = ORIENTED_EDGE ( 'NONE', *, *, #22703, .T. ) ;
#28851 = ORIENTED_EDGE ( 'NONE', *, *, #2511, .F. ) ;
#28852 = CARTESIAN_POINT ( 'NONE',  ( -30.00000337463118427, 69.28203230275516944, 17.49999999999999645 ) ) ;
#28853 = ADVANCED_FACE ( 'NONE', ( #5676 ), #11112, .F. ) ;
#28854 = DIRECTION ( 'NONE',  ( -1.000000000000000000, 0.000000000000000000, 0.000000000000000000 ) ) ;
#28855 = EDGE_CURVE ( 'NONE', #2567, #12964, #11651, .T. ) ;
#28856 = CARTESIAN_POINT ( 'NONE',  ( 62.33939050065184517, -13.89091430021398565, 12.49999999999999822 ) ) ;
#28857 = DIRECTION ( 'NONE',  ( 0.000000000000000000, 0.000000000000000000, -1.000000000000000000 ) ) ;
#28858 = CARTESIAN_POINT ( 'NONE',  ( -74.30619744048887299, 84.18124734178336155, 32.50000000000000000 ) ) ;
#28859 = ORIENTED_EDGE ( 'NONE', *, *, #21482, .F. ) ;
#28860 = DIRECTION ( 'NONE',  ( 0.000000000000000000, 0.000000000000000000, 1.000000000000000000 ) ) ;
#28861 = AXIS2_PLACEMENT_3D ( 'NONE', #15765, #13493, #13316 ) ;
#28862 = CIRCLE ( 'NONE', #15119, 2.000000000000001776 ) ;
#28863 = DIRECTION ( 'NONE',  ( 0.000000000000000000, 0.000000000000000000, 1.000000000000000000 ) ) ;
#28864 = CARTESIAN_POINT ( 'NONE',  ( 47.99999662536846756, 51.96152422706637708, -9.999999999999998224 ) ) ;
#28865 = ORIENTED_EDGE ( 'NONE', *, *, #2829, .F. ) ;
#28866 = DIRECTION ( 'NONE',  ( 1.000000000000000000, 0.000000000000000000, 0.000000000000000000 ) ) ;
#28867 = CARTESIAN_POINT ( 'NONE',  ( 39.99999662536853151, 69.28203230275518365, -9.999999999999998224 ) ) ;
#28868 = ADVANCED_FACE ( 'NONE', ( #37008 ), #22561, .T. ) ;
#28869 = VERTEX_POINT ( 'NONE', #28741 ) ;
#28870 = EDGE_CURVE ( 'NONE', #9726, #36932, #17123, .T. ) ;
#28871 = ORIENTED_EDGE ( 'NONE', *, *, #18044, .F. ) ;
#28872 = DIRECTION ( 'NONE',  ( 0.000000000000000000, 0.000000000000000000, 1.000000000000000000 ) ) ;
#28873 = EDGE_CURVE ( 'NONE', #31910, #21959, #30866, .T. ) ;
#28874 = AXIS2_PLACEMENT_3D ( 'NONE', #2277, #16342, #36412 ) ;
#28875 = CARTESIAN_POINT ( 'NONE',  ( -35.19434990244938888, 52.39915983220783602, -4.999999999999997335 ) ) ;
#28876 = CARTESIAN_POINT ( 'NONE',  ( 19.99999662536861678, -69.28203230275519786, -5.000000000000000000 ) ) ;
#28877 = DIRECTION ( 'NONE',  ( -1.000000000000000000, 0.000000000000000000, 0.000000000000000000 ) ) ;
#28878 = ORIENTED_EDGE ( 'NONE', *, *, #8363, .T. ) ;
#28879 = CARTESIAN_POINT ( 'NONE',  ( -68.00000337463102085, -51.96152422706641971, 12.50000000000000000 ) ) ;
#28880 = FACE_OUTER_BOUND ( 'NONE', #29084, .T. ) ;
#28881 = CARTESIAN_POINT ( 'NONE',  ( -57.00000337463109901, -60.62177826491083010, -9.999999999999998224 ) ) ;
#28882 = EDGE_LOOP ( 'NONE', ( #13017, #13358 ) ) ;
#28883 = DIRECTION ( 'NONE',  ( 0.000000000000000000, 0.000000000000000000, 1.000000000000000000 ) ) ;
#28884 = VERTEX_POINT ( 'NONE', #2679 ) ;
#28885 = DIRECTION ( 'NONE',  ( 1.000000000000000000, 0.000000000000000000, 0.000000000000000000 ) ) ;
#28886 = CIRCLE ( 'NONE', #9763, 45.00000000000000711 ) ;
#28887 = DIRECTION ( 'NONE',  ( 0.000000000000000000, 0.000000000000000000, -1.000000000000000000 ) ) ;
#28888 = EDGE_CURVE ( 'NONE', #20815, #12717, #22764, .T. ) ;
#28889 = DIRECTION ( 'NONE',  ( 1.000000000000000000, 0.000000000000000000, 0.000000000000000000 ) ) ;
#28890 = ORIENTED_EDGE ( 'NONE', *, *, #2142, .F. ) ;
#28891 = ADVANCED_FACE ( 'NONE', ( #17119 ), #6774, .F. ) ;
#28892 = ORIENTED_EDGE ( 'NONE', *, *, #1629, .T. ) ;
#28893 = DIRECTION ( 'NONE',  ( 0.000000000000000000, 0.000000000000000000, 1.000000000000000000 ) ) ;
#28894 = DIRECTION ( 'NONE',  ( 0.000000000000000000, 0.000000000000000000, 1.000000000000000000 ) ) ;
#28895 = DIRECTION ( 'NONE',  ( 1.000000000000000000, 0.000000000000000000, 0.000000000000000000 ) ) ;
#28896 = ORIENTED_EDGE ( 'NONE', *, *, #4073, .T. ) ;
#28897 = DIRECTION ( 'NONE',  ( 0.000000000000000000, 0.000000000000000000, 1.000000000000000000 ) ) ;
#28898 = CIRCLE ( 'NONE', #30702, 27.00000000000001421 ) ;
#28899 = FACE_BOUND ( 'NONE', #30713, .T. ) ;
#28900 = AXIS2_PLACEMENT_3D ( 'NONE', #35540, #36276, #24837 ) ;
#28901 = EDGE_CURVE ( 'NONE', #15901, #1755, #9045, .T. ) ;
#28902 = CARTESIAN_POINT ( 'NONE',  ( -75.00000337463097821, 25.98076211353318854, -9.999999999999998224 ) ) ;
#28903 = CARTESIAN_POINT ( 'NONE',  ( 56.99999662536844625, -60.62177826491080168, -5.000000000000000000 ) ) ;
#28904 = DIRECTION ( 'NONE',  ( -1.000000000000000000, 0.000000000000000000, -0.000000000000000000 ) ) ;
#28905 = DIRECTION ( 'NONE',  ( 1.000000000000000000, 0.000000000000000000, 0.000000000000000000 ) ) ;
#28906 = PRODUCT_DEFINITION_SHAPE ( 'NONE', 'NONE',  #377 ) ;
#28907 = DIRECTION ( 'NONE',  ( 1.000000000000000000, 0.000000000000000000, 0.000000000000000000 ) ) ;
#28908 = CARTESIAN_POINT ( 'NONE',  ( -80.00000337463094979, 34.64101615137757051, 12.50000000000000000 ) ) ;
#28909 = VERTEX_POINT ( 'NONE', #15043 ) ;
#28910 = LINE ( 'NONE', #20118, #2840 ) ;
#28911 = LINE ( 'NONE', #3434, #11182 ) ;
#28912 = CIRCLE ( 'NONE', #16964, 2.000000000000001776 ) ;
#28913 = DIRECTION ( 'NONE',  ( 1.000000000000000000, 0.000000000000000000, 0.000000000000000000 ) ) ;
#28914 = EDGE_CURVE ( 'NONE', #16077, #1955, #2748, .T. ) ;
#28915 = EDGE_LOOP ( 'NONE', ( #14499, #12130 ) ) ;
#28916 = EDGE_CURVE ( 'NONE', #36648, #8999, #3329, .T. ) ;
#28917 = AXIS2_PLACEMENT_3D ( 'NONE', #11578, #6334, #26408 ) ;
#28918 = ORIENTED_EDGE ( 'NONE', *, *, #337, .F. ) ;
#28919 = VERTEX_POINT ( 'NONE', #35111 ) ;
#28920 = EDGE_CURVE ( 'NONE', #36282, #20160, #24291, .T. ) ;
#28921 = EDGE_CURVE ( 'NONE', #32452, #7645, #26469, .T. ) ;
#28922 = DIRECTION ( 'NONE',  ( 0.000000000000000000, 0.000000000000000000, 1.000000000000000000 ) ) ;
#28923 = CARTESIAN_POINT ( 'NONE',  ( 64.99999662536839651, -60.62177826491080168, -9.999999999999998224 ) ) ;
#28924 = DIRECTION ( 'NONE',  ( 0.000000000000000000, 0.000000000000000000, 1.000000000000000000 ) ) ;
#28925 = VERTEX_POINT ( 'NONE', #26854 ) ;
#28926 = FACE_OUTER_BOUND ( 'NONE', #21638, .T. ) ;
#28927 = AXIS2_PLACEMENT_3D ( 'NONE', #37013, #34212, #11320 ) ;
#28928 = ORIENTED_EDGE ( 'NONE', *, *, #20817, .F. ) ;
#28929 = DIRECTION ( 'NONE',  ( 1.000000000000000000, 0.000000000000000000, 0.000000000000000000 ) ) ;
#28930 = ORIENTED_EDGE ( 'NONE', *, *, #25811, .T. ) ;
#28931 = CARTESIAN_POINT ( 'NONE',  ( 66.00000000000000000, 0.000000000000000000, 0.000000000000000000 ) ) ;
#28932 = VERTEX_POINT ( 'NONE', #20303 ) ;
#28933 = EDGE_LOOP ( 'NONE', ( #30242, #8549, #23908, #4076 ) ) ;
#28934 = CARTESIAN_POINT ( 'NONE',  ( 51.68138994340220904, 113.8157894736842053, 32.50000000000000000 ) ) ;
#28935 = CARTESIAN_POINT ( 'NONE',  ( 2.991272306860053298, -4.046490820311139380, -0.5592653008974324269 ) ) ;
#28936 = DIRECTION ( 'NONE',  ( 0.000000000000000000, 0.000000000000000000, 1.000000000000000000 ) ) ;
#28937 = ORIENTED_EDGE ( 'NONE', *, *, #26454, .T. ) ;
#28938 = DIRECTION ( 'NONE',  ( -0.000000000000000000, -0.000000000000000000, 1.000000000000000000 ) ) ;
#28939 = AXIS2_PLACEMENT_3D ( 'NONE', #9436, #34935, #21048 ) ;
#28940 = ADVANCED_FACE ( 'NONE', ( #23661 ), #12589, .F. ) ;
#28941 = DIRECTION ( 'NONE',  ( 1.000000000000000000, 0.000000000000000000, 0.000000000000000000 ) ) ;
#28942 = DIRECTION ( 'NONE',  ( 0.000000000000000000, 0.000000000000000000, -1.000000000000000000 ) ) ;
#28943 = CIRCLE ( 'NONE', #13396, 25.00000000000000000 ) ;
#28944 = ORIENTED_EDGE ( 'NONE', *, *, #31808, .T. ) ;
#28945 = DIRECTION ( 'NONE',  ( -1.000000000000000000, 0.000000000000000000, 0.000000000000000000 ) ) ;
#28946 = DIRECTION ( 'NONE',  ( 0.000000000000000000, 0.000000000000000000, 1.000000000000000000 ) ) ;
#28947 = ORIENTED_EDGE ( 'NONE', *, *, #8860, .F. ) ;
#28948 = FACE_OUTER_BOUND ( 'NONE', #15342, .T. ) ;
#28949 = DIRECTION ( 'NONE',  ( 1.000000000000000000, 0.000000000000000000, 0.000000000000000000 ) ) ;
#28950 = DIRECTION ( 'NONE',  ( 0.000000000000000000, 0.000000000000000000, -1.000000000000000000 ) ) ;
#28951 = DIRECTION ( 'NONE',  ( 1.000000000000000000, 0.000000000000000000, 0.000000000000000000 ) ) ;
#28952 = AXIS2_PLACEMENT_3D ( 'NONE', #26740, #9687, #33098 ) ;
#28953 = CARTESIAN_POINT ( 'NONE',  ( 2.999999999999768630, -68.00000000000000000, -4.999999999999997335 ) ) ;
#28954 = AXIS2_PLACEMENT_3D ( 'NONE', #31150, #13891, #17 ) ;
#28955 = ORIENTED_EDGE ( 'NONE', *, *, #22469, .F. ) ;
#28956 = CARTESIAN_POINT ( 'NONE',  ( -108.3061974404900241, -19.22934205794863516, 32.50000000000000000 ) ) ;
#28957 = DIRECTION ( 'NONE',  ( -0.000000000000000000, -0.000000000000000000, 1.000000000000000000 ) ) ;
#28958 = DIRECTION ( 'NONE',  ( 0.000000000000000000, 0.000000000000000000, 1.000000000000000000 ) ) ;
#28959 = VERTEX_POINT ( 'NONE', #6057 ) ;
#28960 = ORIENTED_EDGE ( 'NONE', *, *, #29289, .T. ) ;
#28961 = ORIENTED_EDGE ( 'NONE', *, *, #2525, .T. ) ;
#28962 = EDGE_CURVE ( 'NONE', #9593, #19500, #18208, .T. ) ;
#28963 = DIRECTION ( 'NONE',  ( 1.000000000000000000, 0.000000000000000000, 0.000000000000000000 ) ) ;
#28964 = DIRECTION ( 'NONE',  ( 1.000000000000000000, 0.000000000000000000, 0.000000000000000000 ) ) ;
#28965 = LINE ( 'NONE', #845, #18279 ) ;
#28966 = CIRCLE ( 'NONE', #13990, 33.00000000000001421 ) ;
#28967 = FACE_OUTER_BOUND ( 'NONE', #25558, .T. ) ;
#28968 = ORIENTED_EDGE ( 'NONE', *, *, #19979, .T. ) ;
#28969 = DIRECTION ( 'NONE',  ( 0.000000000000000000, 0.000000000000000000, -1.000000000000000000 ) ) ;
#28970 = ORIENTED_EDGE ( 'NONE', *, *, #30286, .T. ) ;
#28971 = FACE_BOUND ( 'NONE', #32818, .T. ) ;
#28972 = AXIS2_PLACEMENT_3D ( 'NONE', #959, #12375, #23848 ) ;
#28973 = DIRECTION ( 'NONE',  ( 0.000000000000000000, 0.000000000000000000, 1.000000000000000000 ) ) ;
#28974 = AXIS2_PLACEMENT_3D ( 'NONE', #16305, #7487, #27562 ) ;
#28975 = DIRECTION ( 'NONE',  ( 0.000000000000000000, 0.000000000000000000, -1.000000000000000000 ) ) ;
#28976 = ORIENTED_EDGE ( 'NONE', *, *, #27397, .T. ) ;
#28977 = DIRECTION ( 'NONE',  ( 1.000000000000000000, 0.000000000000000000, 0.000000000000000000 ) ) ;
#28978 = EDGE_CURVE ( 'NONE', #12040, #32985, #29064, .T. ) ;
#28979 = PRODUCT_CONTEXT ( 'NONE', #11542, 'mechanical' ) ;
#28980 = CARTESIAN_POINT ( 'NONE',  ( -67.30619744048885877, 84.18124734178336155, 32.50000000000000000 ) ) ;
#28981 = CARTESIAN_POINT ( 'NONE',  ( -67.00000337463102085, 43.30127018922198801, -9.999999999999998224 ) ) ;
#28982 = CARTESIAN_POINT ( 'NONE',  ( -78.00000337463094979, 34.64101615137757051, -9.999999999999998224 ) ) ;
#28983 = ORIENTED_EDGE ( 'NONE', *, *, #12252, .T. ) ;
#28984 = CARTESIAN_POINT ( 'NONE',  ( -51.13139720814380951, 27.50000000000055422, 5.000000000000000888 ) ) ;
#28985 = AXIS2_PLACEMENT_3D ( 'NONE', #20254, #26049, #23607 ) ;
#28986 = DIRECTION ( 'NONE',  ( 1.000000000000000000, 0.000000000000000000, 0.000000000000000000 ) ) ;
#28987 = DIRECTION ( 'NONE',  ( 1.000000000000000000, 0.000000000000000000, 0.000000000000000000 ) ) ;
#28988 = ORIENTED_EDGE ( 'NONE', *, *, #7100, .F. ) ;
#28989 = MECHANICAL_DESIGN_GEOMETRIC_PRESENTATION_REPRESENTATION (  '', ( #32584 ), #3844 ) ;
#28990 = EDGE_CURVE ( 'NONE', #1755, #6989, #33883, .T. ) ;
#28991 = VERTEX_POINT ( 'NONE', #3972 ) ;
#28992 = ORIENTED_EDGE ( 'NONE', *, *, #998, .F. ) ;
#28993 = CARTESIAN_POINT ( 'NONE',  ( -51.13139720814437084, -27.49999999999955591, -10.00000000000000000 ) ) ;
#28994 = CIRCLE ( 'NONE', #2057, 27.00000000000001421 ) ;
#28995 = CIRCLE ( 'NONE', #2682, 6.000000000000005329 ) ;
#28996 = DIRECTION ( 'NONE',  ( 0.000000000000000000, 0.000000000000000000, 1.000000000000000000 ) ) ;
#28997 = ORIENTED_EDGE ( 'NONE', *, *, #35762, .F. ) ;
#28998 = AXIS2_PLACEMENT_3D ( 'NONE', #22061, #25067, #33500 ) ;
#28999 = ADVANCED_FACE ( 'NONE', ( #15415 ), #9215, .T. ) ;
#29000 = CARTESIAN_POINT ( 'NONE',  ( -37.50000000000000000, 103.4105893997321743, 18.49999999999999645 ) ) ;
#29001 = DIRECTION ( 'NONE',  ( 0.000000000000000000, 0.000000000000000000, 1.000000000000000000 ) ) ;
#29002 = CARTESIAN_POINT ( 'NONE',  ( 110.2237710830536770, 101.7384897088147397, 32.55002500000000509 ) ) ;
#29003 = CARTESIAN_POINT ( 'NONE',  ( -3.374631289687624047E-06, -69.28203230275519786, -9.999999999999998224 ) ) ;
#29004 = ORIENTED_EDGE ( 'NONE', *, *, #33880, .T. ) ;
#29005 = ORIENTED_EDGE ( 'NONE', *, *, #33101, .F. ) ;
#29006 = DIRECTION ( 'NONE',  ( 1.000000000000000000, 0.000000000000000000, 0.000000000000000000 ) ) ;
#29007 = VECTOR ( 'NONE', #12152, 1000.000000000000000 ) ;
#29008 = FACE_OUTER_BOUND ( 'NONE', #16775, .T. ) ;
#29009 = AXIS2_PLACEMENT_3D ( 'NONE', #6477, #17909, #29338 ) ;
#29010 = FACE_OUTER_BOUND ( 'NONE', #34857, .T. ) ;
#29011 = ORIENTED_EDGE ( 'NONE', *, *, #13464, .T. ) ;
#29012 = ADVANCED_FACE ( 'NONE', ( #3230 ), #35314, .F. ) ;
#29013 = VECTOR ( 'NONE', #8467, 1000.000000000000000 ) ;
#29014 = FACE_BOUND ( 'NONE', #1844, .T. ) ;
#29015 = ORIENTED_EDGE ( 'NONE', *, *, #24622, .F. ) ;
#29016 = ORIENTED_EDGE ( 'NONE', *, *, #711, .F. ) ;
#29017 = EDGE_CURVE ( 'NONE', #630, #7909, #27928, .T. ) ;
#29018 = CARTESIAN_POINT ( 'NONE',  ( 2.500000000000003109, -4.330127018922192761, -6.000000000000000000 ) ) ;
#29019 = EDGE_LOOP ( 'NONE', ( #12938, #21124, #26907, #24718 ) ) ;
#29020 = CIRCLE ( 'NONE', #4508, 3.000000000000002665 ) ;
#29021 = AXIS2_PLACEMENT_3D ( 'NONE', #17693, #29128, #26502 ) ;
#29022 = FACE_OUTER_BOUND ( 'NONE', #31028, .T. ) ;
#29023 = CARTESIAN_POINT ( 'NONE',  ( 49.99999662536846756, 69.28203230275516944, -5.000000000000000000 ) ) ;
#29024 = ORIENTED_EDGE ( 'NONE', *, *, #28219, .F. ) ;
#29025 = VERTEX_POINT ( 'NONE', #412 ) ;
#29026 = EDGE_CURVE ( 'NONE', #3457, #9908, #12934, .T. ) ;
#29027 = VERTEX_POINT ( 'NONE', #29089 ) ;
#29028 = ORIENTED_EDGE ( 'NONE', *, *, #25934, .T. ) ;
#29029 = EDGE_CURVE ( 'NONE', #15973, #28764, #20647, .T. ) ;
#29030 = EDGE_LOOP ( 'NONE', ( #35618, #31709, #22320 ) ) ;
#29032 = CYLINDRICAL_SURFACE ( 'NONE', #4467, 2.000000000000001776 ) ;
#29031 = AXIS2_PLACEMENT_3D ( 'NONE', #22597, #27836, #7805 ) ;
#29033 = DIRECTION ( 'NONE',  ( 0.000000000000000000, 0.000000000000000000, -1.000000000000000000 ) ) ;
#29034 = ORIENTED_EDGE ( 'NONE', *, *, #8493, .T. ) ;
#29035 = AXIS2_PLACEMENT_3D ( 'NONE', #29643, #9418, #23865 ) ;
#29036 = DIRECTION ( 'NONE',  ( 1.000000000000000000, 0.000000000000000000, 0.000000000000000000 ) ) ;
#29037 = CARTESIAN_POINT ( 'NONE',  ( 88.66518046043564993, 71.67709580616666187, 32.50000000000000000 ) ) ;
#29038 = DIRECTION ( 'NONE',  ( -1.000000000000000000, 0.000000000000000000, 0.000000000000000000 ) ) ;
#29039 = AXIS2_PLACEMENT_3D ( 'NONE', #18444, #21054, #9797 ) ;
#29040 = ORIENTED_EDGE ( 'NONE', *, *, #28729, .T. ) ;
#29041 = CIRCLE ( 'NONE', #12885, 2.000000000000001776 ) ;
#29042 = CARTESIAN_POINT ( 'NONE',  ( 69.99999662536838230, -51.96152422706639840, -9.999999999999998224 ) ) ;
#29043 = DIRECTION ( 'NONE',  ( 0.000000000000000000, 0.000000000000000000, 1.000000000000000000 ) ) ;
#29044 = CARTESIAN_POINT ( 'NONE',  ( -63.00000337463102085, 25.98076211353317433, -5.000000000000000000 ) ) ;
#29045 = ORIENTED_EDGE ( 'NONE', *, *, #12293, .F. ) ;
#29046 = CYLINDRICAL_SURFACE ( 'NONE', #5310, 2.000000000000001776 ) ;
#29047 = DIRECTION ( 'NONE',  ( 0.000000000000000000, 0.000000000000000000, 1.000000000000000000 ) ) ;
#29048 = AXIS2_PLACEMENT_3D ( 'NONE', #29710, #31950, #15484 ) ;
#29049 = AXIS2_PLACEMENT_3D ( 'NONE', #16247, #36500, #28040 ) ;
#29050 = ORIENTED_EDGE ( 'NONE', *, *, #22045, .T. ) ;
#29051 = VECTOR ( 'NONE', #31703, 1000.000000000000000 ) ;
#29052 = VERTEX_POINT ( 'NONE', #3614 ) ;
#29053 = ADVANCED_FACE ( 'NONE', ( #12191 ), #972, .F. ) ;
#29054 = CARTESIAN_POINT ( 'NONE',  ( -3.374631334790434423E-06, 69.28203230275516944, 17.49999999999999645 ) ) ;
#29055 = DIRECTION ( 'NONE',  ( 1.000000000000000000, 0.000000000000000000, 0.000000000000000000 ) ) ;
#29056 = DIRECTION ( 'NONE',  ( 0.000000000000000000, 0.000000000000000000, -1.000000000000000000 ) ) ;
#29057 =( REPRESENTATION_RELATIONSHIP ('NONE','NONE', #15268, #22738 ) REPRESENTATION_RELATIONSHIP_WITH_TRANSFORMATION ( #1975 )SHAPE_REPRESENTATION_RELATIONSHIP( ) );
#29058 = CYLINDRICAL_SURFACE ( 'NONE', #28657, 2.000000000000001776 ) ;
#29059 = ORIENTED_EDGE ( 'NONE', *, *, #1869, .T. ) ;
#29060 = DIRECTION ( 'NONE',  ( 1.000000000000000000, 0.000000000000000000, 0.000000000000000000 ) ) ;
#29061 = ADVANCED_FACE ( 'NONE', ( #4174 ), #18974, .F. ) ;
#29062 = CARTESIAN_POINT ( 'NONE',  ( -18.00000337463124467, 69.28203230275516944, -9.999999999999998224 ) ) ;
#29063 = CARTESIAN_POINT ( 'NONE',  ( -70.00000337463102085, -34.64101615137762025, 17.49999999999999645 ) ) ;
#29064 = CIRCLE ( 'NONE', #12905, 1.999999999999998224 ) ;
#29065 = EDGE_LOOP ( 'NONE', ( #23828, #9261, #35549, #19772 ) ) ;
#29066 = EDGE_CURVE ( 'NONE', #16370, #19009, #27406, .T. ) ;
#29067 = AXIS2_PLACEMENT_3D ( 'NONE', #24261, #13012, #35715 ) ;
#29068 = DIRECTION ( 'NONE',  ( 0.000000000000000000, 0.000000000000000000, 1.000000000000000000 ) ) ;
#29069 = ORIENTED_EDGE ( 'NONE', *, *, #35094, .F. ) ;
#29070 = AXIS2_PLACEMENT_3D ( 'NONE', #5980, #33977, #22853 ) ;
#29071 = CIRCLE ( 'NONE', #15324, 2.000000000000001776 ) ;
#29072 = CIRCLE ( 'NONE', #15927, 65.00000000000000000 ) ;
#29073 = CARTESIAN_POINT ( 'NONE',  ( 98.28784258492957804, -106.7731239591692116, 27.50000000000000000 ) ) ;
#29074 = CIRCLE ( 'NONE', #27881, 3.499999999999989342 ) ;
#29075 = CARTESIAN_POINT ( 'NONE',  ( 56.74224907229030634, -68.66839587347224949, -49.22241343995298024 ) ) ;
#29076 = CARTESIAN_POINT ( 'NONE',  ( 44.99999662536849598, -77.94228634059960825, 12.50000000000000000 ) ) ;
#29077 = VERTEX_POINT ( 'NONE', #1905 ) ;
#29078 = VERTEX_POINT ( 'NONE', #13328 ) ;
#29079 = LINE ( 'NONE', #3060, #27348 ) ;
#29080 = CARTESIAN_POINT ( 'NONE',  ( -70.00000337463099243, -2.428612866367529932E-14, -9.999999999999998224 ) ) ;
#29081 = AXIS2_PLACEMENT_3D ( 'NONE', #8836, #17458, #10653 ) ;
#29082 = CARTESIAN_POINT ( 'NONE',  ( 0.000000000000000000, 0.000000000000000000, -5.000000000000000000 ) ) ;
#29083 = EDGE_CURVE ( 'NONE', #19786, #19362, #31502, .T. ) ;
#29084 = EDGE_LOOP ( 'NONE', ( #30927, #2571, #21786, #18602, #24802, #29703, #27712, #26358, #6359, #24120, #22183, #17472, #46, #33690, #13128, #16732, #22054, #5049, #17170, #9933, #13183, #32033, #30041, #13892, #9182, #28241, #28494, #33750, #21739, #20459, #30177, #1880, #16559, #33252, #13896 ) ) ;
#29085 = DIRECTION ( 'NONE',  ( -0.000000000000000000, -0.000000000000000000, -1.000000000000000000 ) ) ;
#29086 = FACE_BOUND ( 'NONE', #32094, .T. ) ;
#29087 = CARTESIAN_POINT ( 'NONE',  ( -149.8799519615615736, 6.000000000001555200, 32.55002500000000509 ) ) ;
#29088 = CARTESIAN_POINT ( 'NONE',  ( 5.999999999999985789, 149.8799519615616305, 27.50000000000000000 ) ) ;
#29089 = CARTESIAN_POINT ( 'NONE',  ( 6.999996625368645198, 77.94228634059957983, -5.000000000000000000 ) ) ;
#29090 = CARTESIAN_POINT ( 'NONE',  ( 84.99999662536831124, -8.660254037844397956, -5.000000000000000000 ) ) ;
#29091 = CIRCLE ( 'NONE', #32716, 33.00000000000001421 ) ;
#29092 = FACE_OUTER_BOUND ( 'NONE', #28250, .T. ) ;
#29093 = AXIS2_PLACEMENT_3D ( 'NONE', #30947, #36766, #11441 ) ;
#29094 = PLANE ( 'NONE',  #5601 ) ;
#29095 = EDGE_LOOP ( 'NONE', ( #35365, #19719 ) ) ;
#29096 = DIRECTION ( 'NONE',  ( 0.000000000000000000, 0.000000000000000000, -1.000000000000000000 ) ) ;
#29097 = COLOUR_RGB ( '', 0.31764706, 0.68627451, 0.89019608) ;
#29098 = CARTESIAN_POINT ( 'NONE',  ( -56.67878100130369035, 27.78182860042797131, 12.49999999999999822 ) ) ;
#29099 = CARTESIAN_POINT ( 'NONE',  ( 42.99999662536850309, -60.62177826491080168, 12.50000000000000000 ) ) ;
#29100 = CIRCLE ( 'NONE', #2786, 30.00000000000000000 ) ;
#29101 = CIRCLE ( 'NONE', #10574, 27.00000000000001421 ) ;
#29102 = CIRCLE ( 'NONE', #36301, 33.00000000000001421 ) ;
#29103 = ORIENTED_EDGE ( 'NONE', *, *, #29524, .F. ) ;
#29104 = CIRCLE ( 'NONE', #1576, 33.00000000000001421 ) ;
#29105 = VERTEX_POINT ( 'NONE', #30401 ) ;
#29106 = AXIS2_PLACEMENT_3D ( 'NONE', #12185, #35103, #32276 ) ;
#29107 = ADVANCED_FACE ( 'NONE', ( #9775 ), #32644, .F. ) ;
#29108 = ORIENTED_EDGE ( 'NONE', *, *, #11468, .T. ) ;
#29109 = CARTESIAN_POINT ( 'NONE',  ( -65.00000337463104927, -25.98076211353322051, 17.49999999999999645 ) ) ;
#29110 = DIRECTION ( 'NONE',  ( 0.000000000000000000, 0.000000000000000000, -1.000000000000000000 ) ) ;
#29111 = EDGE_CURVE ( 'NONE', #31389, #18535, #21604, .T. ) ;
#29112 = DIRECTION ( 'NONE',  ( 1.000000000000000000, 0.000000000000000000, 0.000000000000000000 ) ) ;
#29113 = EDGE_LOOP ( 'NONE', ( #36299, #21400, #34388, #23435 ) ) ;
#29114 = ORIENTED_EDGE ( 'NONE', *, *, #35762, .T. ) ;
#29115 = EDGE_CURVE ( 'NONE', #7710, #34867, #36043, .T. ) ;
#29116 = CARTESIAN_POINT ( 'NONE',  ( -70.00000337463102085, -34.64101615137762025, -5.000000000000000000 ) ) ;
#29117 = ORIENTED_EDGE ( 'NONE', *, *, #26872, .T. ) ;
#29118 = FACE_OUTER_BOUND ( 'NONE', #28448, .T. ) ;
#29120 = EDGE_CURVE ( 'NONE', #26265, #34844, #2185, .T. ) ;
#29119 = ORIENTED_EDGE ( 'NONE', *, *, #22390, .F. ) ;
#29121 = DIRECTION ( 'NONE',  ( 1.000000000000000000, 0.000000000000000000, 0.000000000000000000 ) ) ;
#29122 = ORIENTED_EDGE ( 'NONE', *, *, #20359, .T. ) ;
#29123 = EDGE_CURVE ( 'NONE', #3432, #3167, #7526, .T. ) ;
#29124 = CIRCLE ( 'NONE', #28539, 2.000000000000001776 ) ;
#29125 = ORIENTED_EDGE ( 'NONE', *, *, #22942, .F. ) ;
#29126 = CARTESIAN_POINT ( 'NONE',  ( 45.00000000000000000, 5.510910596163089556E-15, -5.000000000000000888 ) ) ;
#29127 = CARTESIAN_POINT ( 'NONE',  ( 1.332830945733272987, -5.003992386592898356, -0.8603634151101718919 ) ) ;
#29128 = DIRECTION ( 'NONE',  ( 0.000000000000000000, 0.000000000000000000, -1.000000000000000000 ) ) ;
#29129 = ORIENTED_EDGE ( 'NONE', *, *, #1221, .T. ) ;
#29130 = PRODUCT_DEFINITION_FORMATION_WITH_SPECIFIED_SOURCE ( 'ANY', '', #10399, .NOT_KNOWN. ) ;
#29131 = CARTESIAN_POINT ( 'NONE',  ( -13.00000337463126066, 77.94228634059957983, 12.50000000000000000 ) ) ;
#29132 = AXIS2_PLACEMENT_3D ( 'NONE', #32558, #7264, #9702 ) ;
#29133 = ADVANCED_FACE ( 'NONE', ( #30201 ), #15605, .F. ) ;
#29134 = CIRCLE ( 'NONE', #33947, 2.000000000000001776 ) ;
#29135 = FACE_OUTER_BOUND ( 'NONE', #9053, .T. ) ;
#29136 = EDGE_CURVE ( 'NONE', #31157, #23602, #18610, .T. ) ;
#29137 = CARTESIAN_POINT ( 'NONE',  ( -5.000000000000001776, -2.068744420501230419, -4.095495254313954447 ) ) ;
#29138 = CIRCLE ( 'NONE', #30324, 2.000000000000001776 ) ;
#29139 = EDGE_CURVE ( 'NONE', #18222, #4910, #4733, .T. ) ;
#29140 = VERTEX_POINT ( 'NONE', #27026 ) ;
#29141 = DIRECTION ( 'NONE',  ( 0.000000000000000000, 0.000000000000000000, -1.000000000000000000 ) ) ;
#29142 = DIRECTION ( 'NONE',  ( 1.000000000000000000, 0.000000000000000000, 0.000000000000000000 ) ) ;
#29143 = EDGE_CURVE ( 'NONE', #20167, #20440, #16170, .T. ) ;
#29144 = ORIENTED_EDGE ( 'NONE', *, *, #36539, .F. ) ;
#29145 = DIRECTION ( 'NONE',  ( 0.000000000000000000, 0.000000000000000000, 1.000000000000000000 ) ) ;
#29146 = DIRECTION ( 'NONE',  ( 0.000000000000000000, -0.000000000000000000, -1.000000000000000000 ) ) ;
#29147 = CYLINDRICAL_SURFACE ( 'NONE', #23185, 2.000000000000001776 ) ;
#29148 = CARTESIAN_POINT ( 'NONE',  ( 0.000000000000000000, 0.000000000000000000, -5.000000000000000000 ) ) ;
#29149 = AXIS2_PLACEMENT_3D ( 'NONE', #35510, #19002, #4205 ) ;
#29150 = DIRECTION ( 'NONE',  ( 1.000000000000000000, 0.000000000000000000, 0.000000000000000000 ) ) ;
#29151 = DIRECTION ( 'NONE',  ( -1.000000000000000000, -0.000000000000000000, -0.000000000000000000 ) ) ;
#29152 = EDGE_LOOP ( 'NONE', ( #2913, #3723 ) ) ;
#29153 = DIRECTION ( 'NONE',  ( -1.000000000000000000, 0.000000000000000000, 0.000000000000000000 ) ) ;
#29154 = CARTESIAN_POINT ( 'NONE',  ( -67.00000337463102085, 25.98076211353317433, -9.999999999999998224 ) ) ;
#29155 = DIRECTION ( 'NONE',  ( 0.000000000000000000, 0.000000000000000000, 1.000000000000000000 ) ) ;
#29156 = AXIS2_PLACEMENT_3D ( 'NONE', #4343, #4530, #1513 ) ;
#29157 = EDGE_LOOP ( 'NONE', ( #35470, #3890, #16862, #22385 ) ) ;
#29158 = ORIENTED_EDGE ( 'NONE', *, *, #35203, .T. ) ;
#29159 = ORIENTED_EDGE ( 'NONE', *, *, #36790, .T. ) ;
#29160 = CIRCLE ( 'NONE', #10036, 2.000000000000001776 ) ;
#29161 = AXIS2_PLACEMENT_3D ( 'NONE', #35474, #6206, #29625 ) ;
#29162 = CARTESIAN_POINT ( 'NONE',  ( 4.451834738187385721E-15, -5.807447148981909280, -4.151008977024224222 ) ) ;
#29163 = DIRECTION ( 'NONE',  ( 0.000000000000000000, 0.000000000000000000, 1.000000000000000000 ) ) ;
#29164 = ORIENTED_EDGE ( 'NONE', *, *, #27520, .F. ) ;
#29165 = DIRECTION ( 'NONE',  ( 0.000000000000000000, 0.000000000000000000, 1.000000000000000000 ) ) ;
#29166 = VECTOR ( 'NONE', #34047, 1000.000000000000000 ) ;
#29167 = AXIS2_PLACEMENT_3D ( 'NONE', #14821, #17076, #25724 ) ;
#29168 = CIRCLE ( 'NONE', #2818, 3.500000000000003109 ) ;
#29169 = FACE_OUTER_BOUND ( 'NONE', #26758, .T. ) ;
#29170 = EDGE_LOOP ( 'NONE', ( #11055, #4219 ) ) ;
#29171 = DIRECTION ( 'NONE',  ( 0.000000000000000000, 0.000000000000000000, 1.000000000000000000 ) ) ;
#29172 = ORIENTED_EDGE ( 'NONE', *, *, #22141, .T. ) ;
#29173 = FACE_BOUND ( 'NONE', #26095, .T. ) ;
#29174 = AXIS2_PLACEMENT_3D ( 'NONE', #4261, #7431, #36121 ) ;
#29175 = AXIS2_PLACEMENT_3D ( 'NONE', #16703, #7704, #16325 ) ;
#29176 = CARTESIAN_POINT ( 'NONE',  ( -40.00000337463113453, 69.28203230275516944, 17.49999999999999645 ) ) ;
#29177 = FACE_OUTER_BOUND ( 'NONE', #8809, .T. ) ;
#29178 = EDGE_LOOP ( 'NONE', ( #27096, #26644, #22489, #10834, #4277 ) ) ;
#29179 = DIRECTION ( 'NONE',  ( 1.000000000000000000, 0.000000000000000000, 0.000000000000000000 ) ) ;
#29180 = AXIS2_PLACEMENT_3D ( 'NONE', #4943, #25025, #30795 ) ;
#29181 = SHAPE_DEFINITION_REPRESENTATION ( #5561, #33015 ) ;
#29182 = CIRCLE ( 'NONE', #18412, 2.000000000000000000 ) ;
#29183 = CARTESIAN_POINT ( 'NONE',  ( 62.19434990244976547, -52.39915983220758022, -49.22241343995298024 ) ) ;
#29184 = CYLINDRICAL_SURFACE ( 'NONE', #19783, 2.000000000000001776 ) ;
#29185 = CARTESIAN_POINT ( 'NONE',  ( 62.99999662536841072, -25.98076211353320275, -9.999999999999998224 ) ) ;
#29186 = ADVANCED_FACE ( 'NONE', ( #15971 ), #24613, .T. ) ;
#29187 = VERTEX_POINT ( 'NONE', #30591 ) ;
#29188 = CARTESIAN_POINT ( 'NONE',  ( -56.67878100130369035, 27.78182860042797131, 12.49999999999999822 ) ) ;
#29189 = DIRECTION ( 'NONE',  ( 0.000000000000000000, 0.000000000000000000, 1.000000000000000000 ) ) ;
#29190 = DIRECTION ( 'NONE',  ( 0.000000000000000000, 0.000000000000000000, 1.000000000000000000 ) ) ;
#29191 = AXIS2_PLACEMENT_3D ( 'NONE', #5432, #3151, #1231 ) ;
#29192 = EDGE_LOOP ( 'NONE', ( #10119, #4136, #27355, #33873 ) ) ;
#29193 = AXIS2_PLACEMENT_3D ( 'NONE', #36068, #21798, #10555 ) ;
#29194 = VERTEX_POINT ( 'NONE', #35859 ) ;
#29195 = ORIENTED_EDGE ( 'NONE', *, *, #33880, .F. ) ;
#29196 = DIRECTION ( 'NONE',  ( 1.000000000000000000, 0.000000000000000000, 0.000000000000000000 ) ) ;
#29197 = DIRECTION ( 'NONE',  ( -1.000000000000000000, 0.000000000000000000, 0.000000000000000000 ) ) ;
#29198 = CIRCLE ( 'NONE', #26213, 2.000000000000000000 ) ;
#29199 = DIRECTION ( 'NONE',  ( 1.000000000000000000, 0.000000000000000000, 0.000000000000000000 ) ) ;
#29200 = CARTESIAN_POINT ( 'NONE',  ( 66.50937412064257614, -41.98910420248104458, -5.000000000000000000 ) ) ;
#29201 = DIRECTION ( 'NONE',  ( 0.000000000000000000, 0.000000000000000000, 1.000000000000000000 ) ) ;
#29202 = VECTOR ( 'NONE', #28064, 1000.000000000000000 ) ;
#29203 = VECTOR ( 'NONE', #410, 1000.000000000000000 ) ;
#29204 = ADVANCED_FACE ( 'NONE', ( #4909 ), #27760, .T. ) ;
#29205 = CARTESIAN_POINT ( 'NONE',  ( 9.999996625368655856, -86.60254037844400443, -9.999999999999998224 ) ) ;
#29206 = ADVANCED_FACE ( 'NONE', ( #2075 ), #13512, .F. ) ;
#29207 = EDGE_LOOP ( 'NONE', ( #23900, #9121 ) ) ;
#29208 = AXIS2_PLACEMENT_3D ( 'NONE', #3868, #17398, #6312 ) ;
#29209 = ORIENTED_EDGE ( 'NONE', *, *, #3213, .T. ) ;
#29210 = CARTESIAN_POINT ( 'NONE',  ( -23.00000337463121980, -77.94228634059963667, 12.50000000000000000 ) ) ;
#29211 = VECTOR ( 'NONE', #35068, 1000.000000000000000 ) ;
#29212 = CARTESIAN_POINT ( 'NONE',  ( -75.00000337463097821, 8.660254037844374864, -5.000000000000000000 ) ) ;
#29213 = DIRECTION ( 'NONE',  ( -1.000000000000000000, 0.000000000000000000, -0.000000000000000000 ) ) ;
#29214 = ORIENTED_EDGE ( 'NONE', *, *, #326, .T. ) ;
#29215 = VECTOR ( 'NONE', #36565, 1000.000000000000000 ) ;
#29216 = EDGE_CURVE ( 'NONE', #34250, #15061, #22527, .T. ) ;
#29217 = FACE_BOUND ( 'NONE', #7795, .T. ) ;
#29218 = EDGE_LOOP ( 'NONE', ( #15006, #2424, #27031, #27603 ) ) ;
#29219 = ORIENTED_EDGE ( 'NONE', *, *, #30269, .F. ) ;
#29220 = CARTESIAN_POINT ( 'NONE',  ( 2.074714256722481664, -4.575665857285986959, -5.989444439476606874 ) ) ;
#29221 = ORIENTED_EDGE ( 'NONE', *, *, #29463, .F. ) ;
#29222 = VECTOR ( 'NONE', #32980, 1000.000000000000000 ) ;
#29223 =( NAMED_UNIT ( * ) SI_UNIT ( $, .STERADIAN. ) SOLID_ANGLE_UNIT ( ) );
#29224 = DIRECTION ( 'NONE',  ( 1.000000000000000000, 0.000000000000000000, 0.000000000000000000 ) ) ;
#29225 = AXIS2_PLACEMENT_3D ( 'NONE', #14300, #10918, #5492 ) ;
#29226 = DIRECTION ( 'NONE',  ( -1.000000000000000000, 0.000000000000000000, 0.000000000000000000 ) ) ;
#29227 = FACE_BOUND ( 'NONE', #32834, .T. ) ;
#29228 = EDGE_CURVE ( 'NONE', #2201, #4900, #10890, .T. ) ;
#29229 = ORIENTED_EDGE ( 'NONE', *, *, #29120, .F. ) ;
#29230 = EDGE_LOOP ( 'NONE', ( #5635, #978 ) ) ;
#29231 = CIRCLE ( 'NONE', #34052, 33.00000000000001421 ) ;
#29232 = ORIENTED_EDGE ( 'NONE', *, *, #34712, .F. ) ;
#29233 = AXIS2_PLACEMENT_3D ( 'NONE', #25248, #28048, #27846 ) ;
#29234 = ORIENTED_EDGE ( 'NONE', *, *, #8054, .F. ) ;
#29235 = AXIS2_PLACEMENT_3D ( 'NONE', #7311, #36180, #6935 ) ;
#29236 = EDGE_LOOP ( 'NONE', ( #20521, #11790, #35739 ) ) ;
#29237 = DIRECTION ( 'NONE',  ( 1.000000000000000000, 0.000000000000000000, 0.000000000000000000 ) ) ;
#29238 = DIRECTION ( 'NONE',  ( 1.000000000000000000, 0.000000000000000000, 0.000000000000000000 ) ) ;
#29239 = ORIENTED_EDGE ( 'NONE', *, *, #7657, .F. ) ;
#29240 = FACE_OUTER_BOUND ( 'NONE', #29307, .T. ) ;
#29241 = CARTESIAN_POINT ( 'NONE',  ( 11.99999662536861855, 69.28203230275516944, -9.999999999999998224 ) ) ;
#29242 = CARTESIAN_POINT ( 'NONE',  ( 49.99999662536846756, 69.28203230275516944, -9.999999999999998224 ) ) ;
#29243 = ORIENTED_EDGE ( 'NONE', *, *, #3206, .F. ) ;
#29244 = DIRECTION ( 'NONE',  ( 0.000000000000000000, 0.000000000000000000, 1.000000000000000000 ) ) ;
#29245 = AXIS2_PLACEMENT_3D ( 'NONE', #18461, #15080, #4015 ) ;
#29246 = CARTESIAN_POINT ( 'NONE',  ( 27.99999662536855993, 69.28203230275518365, 17.49999999999999645 ) ) ;
#29247 = EDGE_CURVE ( 'NONE', #8519, #36949, #24323, .T. ) ;
#29248 = CARTESIAN_POINT ( 'NONE',  ( 69.99999662536839651, -17.32050807568879947, -9.999999999999998224 ) ) ;
#29249 = EDGE_LOOP ( 'NONE', ( #12657, #27327, #14256, #21868 ) ) ;
#29250 = CARTESIAN_POINT ( 'NONE',  ( -76.71706625813334313, 9.685775882613420151, -5.000000000000000000 ) ) ;
#29251 = FACE_OUTER_BOUND ( 'NONE', #11532, .T. ) ;
#29252 = ADVANCED_FACE ( 'NONE', ( #22159 ), #19884, .F. ) ;
#29253 = EDGE_LOOP ( 'NONE', ( #17989, #27395, #15349, #28475 ) ) ;
#29254 = ORIENTED_EDGE ( 'NONE', *, *, #1950, .F. ) ;
#29255 = CARTESIAN_POINT ( 'NONE',  ( 52.99999662536844625, 60.62177826491077326, 17.49999999999999645 ) ) ;
#29256 = VECTOR ( 'NONE', #36754, 1000.000000000000000 ) ;
#29257 = CARTESIAN_POINT ( 'NONE',  ( -70.00000337463099243, 51.96152422706637708, 12.50000000000000000 ) ) ;
#29258 = DIRECTION ( 'NONE',  ( 0.000000000000000000, 0.5000000000000011102, 0.8660254037844379305 ) ) ;
#29259 = CARTESIAN_POINT ( 'NONE',  ( -58.48108235278846934, -36.97203788309005290, -4.999999999999997335 ) ) ;
#29260 = EDGE_CURVE ( 'NONE', #12727, #35025, #376, .T. ) ;
#29261 = VERTEX_POINT ( 'NONE', #28500 ) ;
#29262 = DIRECTION ( 'NONE',  ( 0.000000000000000000, 0.000000000000000000, 1.000000000000000000 ) ) ;
#29263 = DIRECTION ( 'NONE',  ( 0.000000000000000000, 0.000000000000000000, -1.000000000000000000 ) ) ;
#29264 = EDGE_CURVE ( 'NONE', #33654, #14526, #20144, .T. ) ;
#29265 = ORIENTED_EDGE ( 'NONE', *, *, #24660, .T. ) ;
#29266 = AXIS2_PLACEMENT_3D ( 'NONE', #25395, #4798, #21837 ) ;
#29267 = CARTESIAN_POINT ( 'NONE',  ( -3.000003374631308173, 77.94228634059957983, -9.999999999999998224 ) ) ;
#29268 = VERTEX_POINT ( 'NONE', #14062 ) ;
#29269 = AXIS2_PLACEMENT_3D ( 'NONE', #1494, #12929, #24389 ) ;
#29270 = DIRECTION ( 'NONE',  ( 0.000000000000000000, 0.000000000000000000, 1.000000000000000000 ) ) ;
#29271 = DIRECTION ( 'NONE',  ( 1.000000000000000000, 0.000000000000000000, 0.000000000000000000 ) ) ;
#29272 = CIRCLE ( 'NONE', #7159, 65.00000000000000000 ) ;
#29273 = DIRECTION ( 'NONE',  ( 1.000000000000000000, 0.000000000000000000, 0.000000000000000000 ) ) ;
#29274 = ORIENTED_EDGE ( 'NONE', *, *, #16539, .T. ) ;
#29275 = AXIS2_PLACEMENT_3D ( 'NONE', #14535, #34970, #832 ) ;
#29276 = ORIENTED_EDGE ( 'NONE', *, *, #13487, .T. ) ;
#29277 = FACE_OUTER_BOUND ( 'NONE', #30266, .T. ) ;
#29278 = CARTESIAN_POINT ( 'NONE',  ( -104.3561661892587722, 35.61482833294783745, 32.49999999999999289 ) ) ;
#29279 = DIRECTION ( 'NONE',  ( 0.000000000000000000, 0.000000000000000000, 1.000000000000000000 ) ) ;
#29280 = ADVANCED_FACE ( 'NONE', ( #12 ), #22713, .T. ) ;
#29281 = VERTEX_POINT ( 'NONE', #8083 ) ;
#29282 = DIRECTION ( 'NONE',  ( 0.000000000000000000, 0.000000000000000000, 1.000000000000000000 ) ) ;
#29283 = FACE_BOUND ( 'NONE', #13161, .T. ) ;
#29284 = DIRECTION ( 'NONE',  ( -0.000000000000000000, -0.000000000000000000, -1.000000000000000000 ) ) ;
#29285 = DIRECTION ( 'NONE',  ( 0.000000000000000000, -0.5000000000000013323, -0.8660254037844379305 ) ) ;
#29286 = CARTESIAN_POINT ( 'NONE',  ( 0.000000000000000000, 92.82302294027094547, 37.47964607176044183 ) ) ;
#29287 = ORIENTED_EDGE ( 'NONE', *, *, #26871, .F. ) ;
#29288 = CARTESIAN_POINT ( 'NONE',  ( -17.00000337463125533, -77.94228634059960825, -5.000000000000000000 ) ) ;
#29289 = EDGE_CURVE ( 'NONE', #31753, #8057, #20721, .T. ) ;
#29290 = CARTESIAN_POINT ( 'NONE',  ( 77.99999662536832545, -17.32050807568879591, -9.999999999999998224 ) ) ;
#29291 = AXIS2_PLACEMENT_3D ( 'NONE', #26920, #26725, #1044 ) ;
#29292 = EDGE_CURVE ( 'NONE', #8890, #33391, #8456, .T. ) ;
#29293 =( LENGTH_UNIT ( ) NAMED_UNIT ( * ) SI_UNIT ( .MILLI., .METRE. ) );
#29294 = VERTEX_POINT ( 'NONE', #2834 ) ;
#29295 = DIRECTION ( 'NONE',  ( 1.000000000000000000, 0.000000000000000000, 0.000000000000000000 ) ) ;
#29296 = CARTESIAN_POINT ( 'NONE',  ( 0.000000000000000000, 0.000000000000000000, 12.49999999999999822 ) ) ;
#29297 = CARTESIAN_POINT ( 'NONE',  ( -48.00000337463112032, -51.96152422706641971, -9.999999999999998224 ) ) ;
#29298 = AXIS2_PLACEMENT_3D ( 'NONE', #34815, #3502, #4051 ) ;
#29299 = VERTEX_POINT ( 'NONE', #33773 ) ;
#29300 = VERTEX_POINT ( 'NONE', #19338 ) ;
#29301 = VECTOR ( 'NONE', #12090, 1000.000000000000000 ) ;
#29302 = VERTEX_POINT ( 'NONE', #19523 ) ;
#29303 = CYLINDRICAL_SURFACE ( 'NONE', #982, 2.000000000000001776 ) ;
#29304 = LINE ( 'NONE', #23881, #18765 ) ;
#29305 = AXIS2_PLACEMENT_3D ( 'NONE', #4591, #7578, #19028 ) ;
#29306 = CARTESIAN_POINT ( 'NONE',  ( 25.30168577890723469, -79.91940132325416357, 12.50000000000000000 ) ) ;
#29307 = EDGE_LOOP ( 'NONE', ( #16009, #24700 ) ) ;
#29308 = ORIENTED_EDGE ( 'NONE', *, *, #2088, .F. ) ;
#29309 = VERTEX_POINT ( 'NONE', #22887 ) ;
#29310 = FACE_OUTER_BOUND ( 'NONE', #4685, .T. ) ;
#29311 = ADVANCED_FACE ( 'NONE', ( #10719 ), #5435, .F. ) ;
#29312 = ORIENTED_EDGE ( 'NONE', *, *, #26125, .F. ) ;
#29313 = CYLINDRICAL_SURFACE ( 'NONE', #17377, 3.499999999999991562 ) ;
#29314 = VERTEX_POINT ( 'NONE', #31146 ) ;
#29315 = AXIS2_PLACEMENT_3D ( 'NONE', #29974, #7109, #10844 ) ;
#29316 = LINE ( 'NONE', #26495, #26745 ) ;
#29317 = ORIENTED_EDGE ( 'NONE', *, *, #30157, .F. ) ;
#29318 = VERTEX_POINT ( 'NONE', #16891 ) ;
#29319 = CARTESIAN_POINT ( 'NONE',  ( -17.55872235085559652, 89.94802294027088863, -23.00000000000000000 ) ) ;
#29320 = FACE_BOUND ( 'NONE', #19019, .T. ) ;
#29321 = DIRECTION ( 'NONE',  ( 1.000000000000000000, 0.000000000000000000, 0.000000000000000000 ) ) ;
#29322 = ORIENTED_EDGE ( 'NONE', *, *, #17911, .T. ) ;
#29323 = VERTEX_POINT ( 'NONE', #28311 ) ;
#29324 = DIRECTION ( 'NONE',  ( 0.000000000000000000, 0.000000000000000000, 1.000000000000000000 ) ) ;
#29325 = CARTESIAN_POINT ( 'NONE',  ( 51.67316999614278217, 68.18636315956837279, -5.000000000000000000 ) ) ;
#29326 = CARTESIAN_POINT ( 'NONE',  ( -5.253687110065723864, -3.069397772387414847, -4.366238859879560508 ) ) ;
#29327 = AXIS2_PLACEMENT_3D ( 'NONE', #6582, #1139, #35637 ) ;
#29328 = ADVANCED_FACE ( 'NONE', ( #25516 ), #20995, .F. ) ;
#29329 = VERTEX_POINT ( 'NONE', #9366 ) ;
#29330 = CARTESIAN_POINT ( 'NONE',  ( 49.99999662536848177, -51.96152422706640550, -9.999999999999998224 ) ) ;
#29331 = DIRECTION ( 'NONE',  ( -1.000000000000000000, 0.000000000000000000, 0.000000000000000000 ) ) ;
#29332 = EDGE_LOOP ( 'NONE', ( #7629, #31341, #30051, #35770, #29406, #33711 ) ) ;
#29333 = AXIS2_PLACEMENT_3D ( 'NONE', #35317, #21037, #1174 ) ;
#29334 = EDGE_CURVE ( 'NONE', #14823, #1054, #32025, .T. ) ;
#29335 = DIRECTION ( 'NONE',  ( 0.000000000000000000, 0.000000000000000000, 1.000000000000000000 ) ) ;
#29336 = LINE ( 'NONE', #3477, #15999 ) ;
#29337 = DIRECTION ( 'NONE',  ( 0.000000000000000000, 0.000000000000000000, -1.000000000000000000 ) ) ;
#29338 = DIRECTION ( 'NONE',  ( -1.000000000000000000, -5.139921410301647641E-15, 0.000000000000000000 ) ) ;
#29339 = EDGE_CURVE ( 'NONE', #28759, #24614, #8769, .T. ) ;
#29340 = DIRECTION ( 'NONE',  ( -1.000000000000000000, 0.000000000000000000, 0.000000000000000000 ) ) ;
#29341 = CIRCLE ( 'NONE', #28727, 100.0000000000000142 ) ;
#29342 = CARTESIAN_POINT ( 'NONE',  ( -2.000003374631334818, 69.28203230275516944, -9.999999999999998224 ) ) ;
#29343 = EDGE_LOOP ( 'NONE', ( #14052, #25933, #33194, #28567 ) ) ;
#29344 = CARTESIAN_POINT ( 'NONE',  ( -19.13981058454750794, 60.93295298010998806, 12.49999999999999822 ) ) ;
#29345 = EDGE_CURVE ( 'NONE', #30962, #6801, #3741, .T. ) ;
#29346 = AXIS2_PLACEMENT_3D ( 'NONE', #11520, #36670, #10969 ) ;
#29347 = CARTESIAN_POINT ( 'NONE',  ( 84.99999662536831124, -8.660254037844397956, -5.000000000000000000 ) ) ;
#29348 = PLANE ( 'NONE',  #11582 ) ;
#29349 = EDGE_CURVE ( 'NONE', #35112, #35608, #18353, .T. ) ;
#29350 = ORIENTED_EDGE ( 'NONE', *, *, #2747, .T. ) ;
#29351 = ORIENTED_EDGE ( 'NONE', *, *, #24453, .F. ) ;
#29352 = ORIENTED_EDGE ( 'NONE', *, *, #23980, .T. ) ;
#29353 = DIRECTION ( 'NONE',  ( 1.000000000000000000, 0.000000000000000000, 0.000000000000000000 ) ) ;
#29354 = DIRECTION ( 'NONE',  ( 0.000000000000000000, 0.000000000000000000, -1.000000000000000000 ) ) ;
#29355 = LINE ( 'NONE', #26174, #21846 ) ;
#29356 = ADVANCED_FACE ( 'NONE', ( #3571 ), #6367, .F. ) ;
#29357 = EDGE_CURVE ( 'NONE', #31244, #22880, #16538, .T. ) ;
#29358 = DIRECTION ( 'NONE',  ( 1.000000000000000000, 0.000000000000000000, 0.000000000000000000 ) ) ;
#29359 = EDGE_CURVE ( 'NONE', #21552, #6546, #2781, .T. ) ;
#29360 = DIRECTION ( 'NONE',  ( -0.000000000000000000, -0.000000000000000000, 1.000000000000000000 ) ) ;
#29361 = EDGE_LOOP ( 'NONE', ( #1973, #7375, #12077, #27447 ) ) ;
#29362 = CIRCLE ( 'NONE', #13798, 2.000000000000001776 ) ;
#29363 = ADVANCED_FACE ( 'NONE', ( #11985 ), #23614, .T. ) ;
#29364 = CARTESIAN_POINT ( 'NONE',  ( 36.99999662536855283, -77.94228634059960825, 12.50000000000000000 ) ) ;
#29365 = ORIENTED_EDGE ( 'NONE', *, *, #15104, .T. ) ;
#29367 = CONICAL_SURFACE ( 'NONE', #14385, 4.999999999999997335, 0.9110539511682894664 ) ;
#29366 = FACE_BOUND ( 'NONE', #19359, .T. ) ;
#29368 = DIRECTION ( 'NONE',  ( 1.000000000000000000, 0.000000000000000000, 0.000000000000000000 ) ) ;
#29369 = DIRECTION ( 'NONE',  ( -1.000000000000000000, 0.000000000000000000, 0.000000000000000000 ) ) ;
#29370 = EDGE_LOOP ( 'NONE', ( #30289, #4121, #33874 ) ) ;
#29371 = LINE ( 'NONE', #6302, #10479 ) ;
#29372 = PRODUCT_CONTEXT ( 'NONE', #13462, 'mechanical' ) ;
#29373 = FACE_OUTER_BOUND ( 'NONE', #23871, .T. ) ;
#29374 = EDGE_CURVE ( 'NONE', #33050, #17955, #6179, .T. ) ;
#29375 = DIRECTION ( 'NONE',  ( -1.000000000000000000, 0.000000000000000000, 0.000000000000000000 ) ) ;
#29376 = DIRECTION ( 'NONE',  ( 0.000000000000000000, 0.000000000000000000, -1.000000000000000000 ) ) ;
#29377 = EDGE_LOOP ( 'NONE', ( #19980, #24655 ) ) ;
#29378 = FACE_OUTER_BOUND ( 'NONE', #16472, .T. ) ;
#29379 = CARTESIAN_POINT ( 'NONE',  ( -62.00000337463108480, -51.96152422706641971, -9.999999999999998224 ) ) ;
#29380 = CARTESIAN_POINT ( 'NONE',  ( -149.8799519615616873, -5.999999999998430589, 32.50000000000000000 ) ) ;
#29381 = EDGE_LOOP ( 'NONE', ( #18876, #11034 ) ) ;
#29382 = VERTEX_POINT ( 'NONE', #12150 ) ;
#29383 = AXIS2_PLACEMENT_3D ( 'NONE', #8586, #20560, #17022 ) ;
#29384 = ORIENTED_EDGE ( 'NONE', *, *, #475, .T. ) ;
#29385 = EDGE_CURVE ( 'NONE', #24271, #10050, #31531, .T. ) ;
#29386 = CARTESIAN_POINT ( 'NONE',  ( 3.000000000000000000, 1.467624384280024730, -2.542000000000001592 ) ) ;
#29387 = CARTESIAN_POINT ( 'NONE',  ( 79.99999662536832545, -34.64101615137759183, 17.49999999999999645 ) ) ;
#29388 = FACE_OUTER_BOUND ( 'NONE', #33158, .T. ) ;
#29389 = PLANE ( 'NONE',  #14598 ) ;
#29390 = CARTESIAN_POINT ( 'NONE',  ( -75.00000337463100664, -43.30127018922202353, -9.999999999999998224 ) ) ;
#29391 = CARTESIAN_POINT ( 'NONE',  ( -10.00000337463128730, 69.28203230275516944, -5.000000000000000000 ) ) ;
#29392 = ORIENTED_EDGE ( 'NONE', *, *, #32637, .T. ) ;
#29394 = ORIENTED_EDGE ( 'NONE', *, *, #943, .F. ) ;
#29393 = EDGE_CURVE ( 'NONE', #4570, #27930, #29424, .T. ) ;
#29395 = DIRECTION ( 'NONE',  ( 1.000000000000000000, 0.000000000000000000, 0.000000000000000000 ) ) ;
#29396 = EDGE_CURVE ( 'NONE', #15480, #22341, #28543, .T. ) ;
#29397 = CARTESIAN_POINT ( 'NONE',  ( 31.46585318596250502, 86.45172111230321832, 12.49999999999999822 ) ) ;
#29399 = EDGE_CURVE ( 'NONE', #4461, #10948, #6736, .T. ) ;
#29398 = ORIENTED_EDGE ( 'NONE', *, *, #8976, .F. ) ;
#29400 = DIRECTION ( 'NONE',  ( -1.000000000000000000, 0.000000000000000000, 0.000000000000000000 ) ) ;
#29401 = ORIENTED_EDGE ( 'NONE', *, *, #20194, .T. ) ;
#29402 = FACE_BOUND ( 'NONE', #31136, .T. ) ;
#29403 = ORIENTED_EDGE ( 'NONE', *, *, #4659, .T. ) ;
#29404 = ORIENTED_EDGE ( 'NONE', *, *, #461, .F. ) ;
#29405 = DIRECTION ( 'NONE',  ( 0.000000000000000000, 0.000000000000000000, 1.000000000000000000 ) ) ;
#29406 = ORIENTED_EDGE ( 'NONE', *, *, #3445, .T. ) ;
#29407 = FILL_AREA_STYLE_COLOUR ( '', #9352 ) ;
#29408 = CARTESIAN_POINT ( 'NONE',  ( -33.00000337463117006, -77.94228634059963667, -9.999999999999998224 ) ) ;
#29409 = CARTESIAN_POINT ( 'NONE',  ( 5.000000000000000000, 2.886751345948137981, -5.553418012614792509 ) ) ;
#29410 = CARTESIAN_POINT ( 'NONE',  ( -45.00000000000000711, 0.000000000000000000, 5.000000000000000000 ) ) ;
#29411 = ORIENTED_EDGE ( 'NONE', *, *, #11488, .T. ) ;
#29412 = ORIENTED_EDGE ( 'NONE', *, *, #27046, .T. ) ;
#29413 = EDGE_LOOP ( 'NONE', ( #29445, #5064 ) ) ;
#29414 = EDGE_CURVE ( 'NONE', #2651, #8103, #33348, .T. ) ;
#29415 = EDGE_LOOP ( 'NONE', ( #20627, #14189, #2296, #32555 ) ) ;
#29416 = ORIENTED_EDGE ( 'NONE', *, *, #10160, .T. ) ;
#29417 = CARTESIAN_POINT ( 'NONE',  ( -20.00000337463123756, -69.28203230275522628, -9.999999999999998224 ) ) ;
#29418 = AXIS2_PLACEMENT_3D ( 'NONE', #25798, #34407, #20500 ) ;
#29419 = LINE ( 'NONE', #3737, #7806 ) ;
#29420 = VERTEX_POINT ( 'NONE', #14445 ) ;
#29421 = AXIS2_PLACEMENT_3D ( 'NONE', #2047, #32822, #13481 ) ;
#29422 = CARTESIAN_POINT ( 'NONE',  ( 77.99999662536833966, 17.32050807568879236, 17.49999999999999645 ) ) ;
#29423 = LINE ( 'NONE', #29241, #4940 ) ;
#29424 = LINE ( 'NONE', #28858, #13588 ) ;
#29425 = ORIENTED_EDGE ( 'NONE', *, *, #32369, .F. ) ;
#29426 = DIRECTION ( 'NONE',  ( 1.000000000000000000, 0.000000000000000000, 0.000000000000000000 ) ) ;
#29427 = DIRECTION ( 'NONE',  ( 1.000000000000000000, 0.000000000000000000, 0.000000000000000000 ) ) ;
#29428 = DIRECTION ( 'NONE',  ( 0.000000000000000000, 0.000000000000000000, 1.000000000000000000 ) ) ;
#29429 = ORIENTED_EDGE ( 'NONE', *, *, #18194, .F. ) ;
#29430 = CYLINDRICAL_SURFACE ( 'NONE', #19647, 30.00000000000000000 ) ;
#29431 = LINE ( 'NONE', #32997, #8799 ) ;
#29432 = ORIENTED_EDGE ( 'NONE', *, *, #19076, .T. ) ;
#29433 = ORIENTED_EDGE ( 'NONE', *, *, #24172, .F. ) ;
#29434 = FACE_OUTER_BOUND ( 'NONE', #15810, .T. ) ;
#29435 = DIRECTION ( 'NONE',  ( -1.000000000000000000, 0.000000000000000000, 0.000000000000000000 ) ) ;
#29436 = ADVANCED_FACE ( 'NONE', ( #17607 ), #11797, .F. ) ;
#29437 = DIRECTION ( 'NONE',  ( 0.000000000000000000, 0.000000000000000000, -1.000000000000000000 ) ) ;
#29438 = LINE ( 'NONE', #11999, #16684 ) ;
#29439 = ORIENTED_EDGE ( 'NONE', *, *, #29083, .F. ) ;
#29440 = FACE_BOUND ( 'NONE', #27139, .T. ) ;
#29441 = DIRECTION ( 'NONE',  ( 1.000000000000000000, 0.000000000000000000, 0.000000000000000000 ) ) ;
#29442 = EDGE_LOOP ( 'NONE', ( #27770, #7197, #21183, #34741, #33039, #22165, #8695, #4766, #15220, #13600 ) ) ;
#29443 = VECTOR ( 'NONE', #13361, 1000.000000000000000 ) ;
#29444 = CYLINDRICAL_SURFACE ( 'NONE', #27391, 3.000000000000002665 ) ;
#29445 = ORIENTED_EDGE ( 'NONE', *, *, #33976, .T. ) ;
#29446 = CARTESIAN_POINT ( 'NONE',  ( 36.99999662536855283, 60.62177826491078747, -9.999999999999998224 ) ) ;
#29447 = CARTESIAN_POINT ( 'NONE',  ( 56.67878100130369035, -27.78182860042797131, 12.49999999999999822 ) ) ;
#29448 = FACE_OUTER_BOUND ( 'NONE', #25325, .T. ) ;
#29449 = ORIENTED_EDGE ( 'NONE', *, *, #17370, .T. ) ;
#29450 = ORIENTED_EDGE ( 'NONE', *, *, #24308, .F. ) ;
#29451 = EDGE_CURVE ( 'NONE', #8999, #36648, #21969, .T. ) ;
#29452 = CARTESIAN_POINT ( 'NONE',  ( 5.000000000000000000, 2.886751345948137981, -5.553418012614792509 ) ) ;
#29453 = ORIENTED_EDGE ( 'NONE', *, *, #2433, .T. ) ;
#29454 = CARTESIAN_POINT ( 'NONE',  ( -55.00000337463109901, -60.62177826491083010, -5.000000000000000000 ) ) ;
#29455 = PLANE ( 'NONE',  #23949 ) ;
#29456 = EDGE_CURVE ( 'NONE', #36578, #245, #4608, .T. ) ;
#29457 = CARTESIAN_POINT ( 'NONE',  ( 104.8061974404898820, 19.22934205794938478, 32.50000000000000000 ) ) ;
#29458 = CARTESIAN_POINT ( 'NONE',  ( 52.99999662536844625, 43.30127018922198801, 17.49999999999999645 ) ) ;
#29459 = DIRECTION ( 'NONE',  ( 1.000000000000000000, 0.000000000000000000, 0.000000000000000000 ) ) ;
#29460 = VERTEX_POINT ( 'NONE', #36174 ) ;
#29461 = DIRECTION ( 'NONE',  ( 0.000000000000000000, 0.000000000000000000, 1.000000000000000000 ) ) ;
#29462 = DIRECTION ( 'NONE',  ( -0.000000000000000000, 0.000000000000000000, -1.000000000000000000 ) ) ;
#29463 = EDGE_CURVE ( 'NONE', #3619, #6911, #35735, .T. ) ;
#29464 = CIRCLE ( 'NONE', #13312, 2.000000000000001776 ) ;
#29465 = VERTEX_POINT ( 'NONE', #33162 ) ;
#29466 = FACE_OUTER_BOUND ( 'NONE', #9517, .T. ) ;
#29467 = CARTESIAN_POINT ( 'NONE',  ( 31.02796211690949235, -59.29837256189548356, 12.49999999999999645 ) ) ;
#29468 = CARTESIAN_POINT ( 'NONE',  ( -45.00000337463111322, -77.94228634059960825, 17.49999999999999645 ) ) ;
#29469 = VERTEX_POINT ( 'NONE', #12912 ) ;
#29470 = ORIENTED_EDGE ( 'NONE', *, *, #3301, .T. ) ;
#29471 = CARTESIAN_POINT ( 'NONE',  ( 2.500000000000021760, -4.330127018922177662, 0.000000000000000000 ) ) ;
#29472 = ADVANCED_FACE ( 'NONE', ( #36003 ), #15563, .F. ) ;
#29473 = DIRECTION ( 'NONE',  ( 0.000000000000000000, 0.000000000000000000, 1.000000000000000000 ) ) ;
#29474 = DIRECTION ( 'NONE',  ( -0.000000000000000000, -0.000000000000000000, 1.000000000000000000 ) ) ;
#29475 = ORIENTED_EDGE ( 'NONE', *, *, #20152, .F. ) ;
#29476 = ORIENTED_EDGE ( 'NONE', *, *, #11592, .T. ) ;
#29477 = ORIENTED_EDGE ( 'NONE', *, *, #16679, .T. ) ;
#29478 = DIRECTION ( 'NONE',  ( 1.000000000000000000, 0.000000000000000000, 0.000000000000000000 ) ) ;
#29479 = AXIS2_PLACEMENT_3D ( 'NONE', #24057, #18224, #21225 ) ;
#29480 = VERTEX_POINT ( 'NONE', #27559 ) ;
#29481 = CARTESIAN_POINT ( 'NONE',  ( -17.74171217315199200, -112.6247319038655235, 32.50000000000000711 ) ) ;
#29482 = ORIENTED_EDGE ( 'NONE', *, *, #20401, .T. ) ;
#29483 = DIRECTION ( 'NONE',  ( 0.000000000000000000, 0.000000000000000000, 1.000000000000000000 ) ) ;
#29484 = ORIENTED_EDGE ( 'NONE', *, *, #5186, .T. ) ;
#29485 = VERTEX_POINT ( 'NONE', #13118 ) ;
#29486 = ADVANCED_FACE ( 'NONE', ( #33365 ), #9735, .F. ) ;
#29487 = FILL_AREA_STYLE ('',( #33393 ) ) ;
#29488 = CARTESIAN_POINT ( 'NONE',  ( 0.7207917504152147048, -5.357353380764381612, -1.325189086772950331 ) ) ;
#29489 = CIRCLE ( 'NONE', #21713, 2.000000000000001776 ) ;
#29490 = ADVANCED_FACE ( 'NONE', ( #4488 ), #30161, .F. ) ;
#29491 = CARTESIAN_POINT ( 'NONE',  ( 37.50000000000000000, 103.4105893997321743, -19.99999999999999645 ) ) ;
#29492 = VERTEX_POINT ( 'NONE', #12549 ) ;
#29493 = VECTOR ( 'NONE', #2517, 1000.000000000000000 ) ;
#29494 = ORIENTED_EDGE ( 'NONE', *, *, #25063, .T. ) ;
#29495 = DIRECTION ( 'NONE',  ( 0.000000000000000000, 0.000000000000000000, 1.000000000000000000 ) ) ;
#29496 = DIRECTION ( 'NONE',  ( -1.000000000000000000, 0.000000000000000000, 0.000000000000000000 ) ) ;
#29497 = ADVANCED_FACE ( 'NONE', ( #10126 ), #18980, .T. ) ;
#29498 = CARTESIAN_POINT ( 'NONE',  ( 68.66839587347284635, 56.74224907228958870, -49.22241343995293761 ) ) ;
#29499 = CARTESIAN_POINT ( 'NONE',  ( -40.00000337463113453, -69.28203230275519786, -5.000000000000000000 ) ) ;
#29500 = ORIENTED_EDGE ( 'NONE', *, *, #3439, .F. ) ;
#29501 = CARTESIAN_POINT ( 'NONE',  ( -80.00000337463094979, -2.428612866367529932E-14, 12.50000000000000000 ) ) ;
#29502 = CARTESIAN_POINT ( 'NONE',  ( 51.99999662536847467, 51.96152422706637708, 17.49999999999999645 ) ) ;
#29503 = VERTEX_POINT ( 'NONE', #19131 ) ;
#29504 = FACE_OUTER_BOUND ( 'NONE', #35995, .T. ) ;
#29505 = EDGE_CURVE ( 'NONE', #2973, #29420, #405, .T. ) ;
#29506 = CARTESIAN_POINT ( 'NONE',  ( -8.000003374631287301, 69.28203230275516944, 12.50000000000000000 ) ) ;
#29507 = CARTESIAN_POINT ( 'NONE',  ( 44.99999662536851019, 77.94228634059959404, 12.50000000000000000 ) ) ;
#29508 = LINE ( 'NONE', #18261, #35030 ) ;
#29509 = CIRCLE ( 'NONE', #34317, 33.00000000000001421 ) ;
#29510 = CARTESIAN_POINT ( 'NONE',  ( 145.0000000000000568, -5.056524707326808249E-13, 32.55002500000000509 ) ) ;
#29511 = EDGE_CURVE ( 'NONE', #23723, #15799, #33938, .T. ) ;
#29512 = CARTESIAN_POINT ( 'NONE',  ( 5.000000000000000000, 1.352381405509861523, -0.8629530094790043293 ) ) ;
#29513 = EDGE_LOOP ( 'NONE', ( #6631, #6180 ) ) ;
#29514 = CARTESIAN_POINT ( 'NONE',  ( 34.99999662536855283, 60.62177826491078747, -5.000000000000000000 ) ) ;
#29515 = DIRECTION ( 'NONE',  ( -0.000000000000000000, -0.000000000000000000, 1.000000000000000000 ) ) ;
#29516 = DIRECTION ( 'NONE',  ( -3.554796214472773777E-16, -1.000000000000000000, 0.000000000000000000 ) ) ;
#29517 = ORIENTED_EDGE ( 'NONE', *, *, #25628, .T. ) ;
#29518 = EDGE_LOOP ( 'NONE', ( #12070, #11507 ) ) ;
#29519 = EDGE_LOOP ( 'NONE', ( #11098, #17664, #31746, #4571, #25397 ) ) ;
#29520 = LINE ( 'NONE', #12650, #34399 ) ;
#29521 = DIRECTION ( 'NONE',  ( 0.000000000000000000, 0.000000000000000000, 1.000000000000000000 ) ) ;
#29522 = CARTESIAN_POINT ( 'NONE',  ( -20.00000337463124112, 69.28203230275516944, 17.49999999999999645 ) ) ;
#29523 = CARTESIAN_POINT ( 'NONE',  ( 56.67878100130369035, -27.78182860042797131, 12.49999999999999822 ) ) ;
#29524 = EDGE_CURVE ( 'NONE', #2400, #24065, #27959, .T. ) ;
#29525 = CARTESIAN_POINT ( 'NONE',  ( 46.99999662536851019, 77.94228634059959404, -9.999999999999998224 ) ) ;
#29526 = ORIENTED_EDGE ( 'NONE', *, *, #7262, .T. ) ;
#29527 = CARTESIAN_POINT ( 'NONE',  ( 35.44550000000001688, 0.000000000000000000, 3.000000000000001332 ) ) ;
#29528 = EDGE_LOOP ( 'NONE', ( #22149, #23173, #2457, #24771 ) ) ;
#29529 = FACE_BOUND ( 'NONE', #9250, .T. ) ;
#29530 = CIRCLE ( 'NONE', #17548, 2.000000000000001776 ) ;
#29531 = EDGE_CURVE ( 'NONE', #9530, #7637, #17755, .T. ) ;
#29532 = AXIS2_PLACEMENT_3D ( 'NONE', #20179, #3342, #26026 ) ;
#29533 = LINE ( 'NONE', #18292, #10159 ) ;
#29534 = EDGE_CURVE ( 'NONE', #16822, #27152, #1007, .T. ) ;
#29535 = LINE ( 'NONE', #23750, #20567 ) ;
#29536 = ADVANCED_FACE ( 'NONE', ( #24171 ), #18370, .F. ) ;
#29537 = ORIENTED_EDGE ( 'NONE', *, *, #22651, .F. ) ;
#29538 = DIRECTION ( 'NONE',  ( 0.000000000000000000, -1.000000000000000000, 0.000000000000000000 ) ) ;
#29539 = CARTESIAN_POINT ( 'NONE',  ( 29.99999662536857770, -69.28203230275519786, -9.999999999999998224 ) ) ;
#29540 = CIRCLE ( 'NONE', #32521, 2.000000000000001776 ) ;
#29541 = DIRECTION ( 'NONE',  ( 1.000000000000000000, 0.000000000000000000, 0.000000000000000000 ) ) ;
#29542 = CARTESIAN_POINT ( 'NONE',  ( -70.00000337463099243, 17.32050807568877460, 12.50000000000000000 ) ) ;
#29543 = EDGE_LOOP ( 'NONE', ( #512, #13733 ) ) ;
#29544 = DIRECTION ( 'NONE',  ( 1.000000000000000000, 0.000000000000000000, 0.000000000000000000 ) ) ;
#29545 = CARTESIAN_POINT ( 'NONE',  ( -35.00000337463116296, 60.62177826491077326, 12.50000000000000000 ) ) ;
#29546 = DIRECTION ( 'NONE',  ( 0.000000000000000000, 0.000000000000000000, 1.000000000000000000 ) ) ;
#29547 = ORIENTED_EDGE ( 'NONE', *, *, #8422, .T. ) ;
#29548 = ORIENTED_EDGE ( 'NONE', *, *, #30284, .T. ) ;
#29549 = EDGE_CURVE ( 'NONE', #4453, #2973, #26810, .T. ) ;
#29550 = ORIENTED_EDGE ( 'NONE', *, *, #21076, .F. ) ;
#29551 = CARTESIAN_POINT ( 'NONE',  ( 42.97377950131529190, 96.90768712682505281, -19.99999999999999645 ) ) ;
#29552 = DIRECTION ( 'NONE',  ( 1.000000000000000000, 0.000000000000000000, 0.000000000000000000 ) ) ;
#29553 = CIRCLE ( 'NONE', #30154, 2.000000000000001776 ) ;
#29554 = CARTESIAN_POINT ( 'NONE',  ( 61.53067111003264955, -72.28378166041994746, -49.22241343995298024 ) ) ;
#29555 = DIRECTION ( 'NONE',  ( 0.000000000000000000, 0.000000000000000000, 1.000000000000000000 ) ) ;
#29556 = FACE_OUTER_BOUND ( 'NONE', #2610, .T. ) ;
#29557 = PLANE ( 'NONE',  #30557 ) ;
#29558 = ORIENTED_EDGE ( 'NONE', *, *, #23082, .F. ) ;
#29559 = VECTOR ( 'NONE', #31876, 1000.000000000000000 ) ;
#29560 = ORIENTED_EDGE ( 'NONE', *, *, #10829, .F. ) ;
#29561 = DIRECTION ( 'NONE',  ( 1.000000000000000000, 0.000000000000000000, 0.000000000000000000 ) ) ;
#29562 = EDGE_CURVE ( 'NONE', #6282, #10243, #34551, .T. ) ;
#29563 =( GEOMETRIC_REPRESENTATION_CONTEXT ( 3 ) GLOBAL_UNCERTAINTY_ASSIGNED_CONTEXT ( ( #30573 ) ) GLOBAL_UNIT_ASSIGNED_CONTEXT ( ( #33209, #10526, #7728 ) ) REPRESENTATION_CONTEXT ( 'NONE', 'WORKASPACE' ) );
#29564 = CARTESIAN_POINT ( 'NONE',  ( 106.7731239591688848, 98.28784258492994752, 32.50000000000000000 ) ) ;
#29565 = ORIENTED_EDGE ( 'NONE', *, *, #16696, .F. ) ;
#29566 = EDGE_CURVE ( 'NONE', #15386, #14472, #14760, .T. ) ;
#29567 = CARTESIAN_POINT ( 'NONE',  ( 0.000000000000000000, 0.000000000000000000, -5.000000000000000000 ) ) ;
#29568 = VERTEX_POINT ( 'NONE', #35623 ) ;
#29569 = ADVANCED_FACE ( 'NONE', ( #9920 ), #21365, .F. ) ;
#29570 = LINE ( 'NONE', #35604, #11923 ) ;
#29571 = ORIENTED_EDGE ( 'NONE', *, *, #6303, .F. ) ;
#29572 = ORIENTED_EDGE ( 'NONE', *, *, #29111, .F. ) ;
#29573 = EDGE_CURVE ( 'NONE', #34610, #17931, #8791, .T. ) ;
#29574 = FACE_OUTER_BOUND ( 'NONE', #11253, .T. ) ;
#29575 = ORIENTED_EDGE ( 'NONE', *, *, #14603, .T. ) ;
#29576 = EDGE_CURVE ( 'NONE', #22308, #11341, #27340, .T. ) ;
#29577 = CIRCLE ( 'NONE', #12797, 2.000000000000001776 ) ;
#29578 = DIRECTION ( 'NONE',  ( 0.000000000000000000, 0.000000000000000000, 1.000000000000000000 ) ) ;
#29579 = CYLINDRICAL_SURFACE ( 'NONE', #9544, 2.000000000000001776 ) ;
#29580 = CARTESIAN_POINT ( 'NONE',  ( 69.99999662536841072, 51.96152422706640550, 17.49999999999999645 ) ) ;
#29581 = EDGE_LOOP ( 'NONE', ( #10456, #25752, #20505, #17473 ) ) ;
#29582 = EDGE_LOOP ( 'NONE', ( #12406, #33171 ) ) ;
#29583 = ADVANCED_BREP_SHAPE_REPRESENTATION ( '', ( #32134, #21385 ), #25533 ) ;
#29584 = EDGE_CURVE ( 'NONE', #4310, #33855, #21378, .T. ) ;
#29585 = VERTEX_POINT ( 'NONE', #16674 ) ;
#29586 = VECTOR ( 'NONE', #32219, 1000.000000000000000 ) ;
#29587 = CIRCLE ( 'NONE', #2058, 27.00000000000001421 ) ;
#29588 = EDGE_CURVE ( 'NONE', #33302, #18995, #9379, .T. ) ;
#29589 = VERTEX_POINT ( 'NONE', #31268 ) ;
#29590 = VERTEX_POINT ( 'NONE', #11905 ) ;
#29591 = EDGE_CURVE ( 'NONE', #14042, #12472, #12360, .T. ) ;
#29592 = DIRECTION ( 'NONE',  ( 0.000000000000000000, -0.000000000000000000, -1.000000000000000000 ) ) ;
#29593 = CIRCLE ( 'NONE', #3855, 33.00000000000001421 ) ;
#29594 = ADVANCED_FACE ( 'NONE', ( #19668 ), #17530, .F. ) ;
#29595 = FACE_OUTER_BOUND ( 'NONE', #16741, .T. ) ;
#29596 = VERTEX_POINT ( 'NONE', #22462 ) ;
#29597 = LINE ( 'NONE', #18167, #35258 ) ;
#29598 = CARTESIAN_POINT ( 'NONE',  ( 101.4252628994511980, 31.43180897937319784, 32.50001250000000397 ) ) ;
#29599 = DIRECTION ( 'NONE',  ( -0.000000000000000000, -0.000000000000000000, 1.000000000000000000 ) ) ;
#29600 = ORIENTED_EDGE ( 'NONE', *, *, #1913, .F. ) ;
#29601 = DIRECTION ( 'NONE',  ( 0.000000000000000000, 0.000000000000000000, 1.000000000000000000 ) ) ;
#29602 = CARTESIAN_POINT ( 'NONE',  ( -55.00000337463107059, 60.62177826491078747, 12.50000000000000000 ) ) ;
#29603 = VECTOR ( 'NONE', #5632, 1000.000000000000000 ) ;
#29604 = DIRECTION ( 'NONE',  ( 1.000000000000000000, 0.000000000000000000, 0.000000000000000000 ) ) ;
#29605 = VERTEX_POINT ( 'NONE', #5035 ) ;
#29606 = CYLINDRICAL_SURFACE ( 'NONE', #16677, 2.000000000000001776 ) ;
#29607 = AXIS2_PLACEMENT_3D ( 'NONE', #8811, #14438, #733 ) ;
#29608 = DIRECTION ( 'NONE',  ( 0.000000000000000000, 0.000000000000000000, 1.000000000000000000 ) ) ;
#29609 = VERTEX_POINT ( 'NONE', #19847 ) ;
#29610 = AXIS2_PLACEMENT_3D ( 'NONE', #6380, #27001, #6747 ) ;
#29611 = VERTEX_POINT ( 'NONE', #33915 ) ;
#29612 = DIRECTION ( 'NONE',  ( -0.000000000000000000, -0.000000000000000000, -1.000000000000000000 ) ) ;
#29613 = DIRECTION ( 'NONE',  ( 1.000000000000000000, 0.000000000000000000, 0.000000000000000000 ) ) ;
#29614 = DIRECTION ( 'NONE',  ( -1.000000000000000000, 0.000000000000000000, 0.000000000000000000 ) ) ;
#29615 = CARTESIAN_POINT ( 'NONE',  ( 0.000000000000000000, 101.4480229402710592, -24.99999999999999645 ) ) ;
#29616 = ORIENTED_EDGE ( 'NONE', *, *, #799, .T. ) ;
#29617 = CIRCLE ( 'NONE', #5092, 2.000000000000001776 ) ;
#29618 = CARTESIAN_POINT ( 'NONE',  ( -25.00000337463121980, -77.94228634059963667, -5.000000000000000000 ) ) ;
#29619 = AXIS2_PLACEMENT_3D ( 'NONE', #21444, #21799, #18453 ) ;
#29620 = DIRECTION ( 'NONE',  ( 1.000000000000000000, 0.000000000000000000, 0.000000000000000000 ) ) ;
#29621 = VECTOR ( 'NONE', #25986, 1000.000000000000000 ) ;
#29622 = ORIENTED_EDGE ( 'NONE', *, *, #4082, .F. ) ;
#29623 = DIRECTION ( 'NONE',  ( 0.000000000000000000, 0.000000000000000000, 1.000000000000000000 ) ) ;
#29624 = VERTEX_POINT ( 'NONE', #2035 ) ;
#29625 = DIRECTION ( 'NONE',  ( -1.051347561198064495E-14, -1.000000000000000000, 0.000000000000000000 ) ) ;
#29626 = CARTESIAN_POINT ( 'NONE',  ( 72.99999662536836809, -8.660254037844401509, 17.49999999999999645 ) ) ;
#29627 = VECTOR ( 'NONE', #29538, 1000.000000000000000 ) ;
#29628 = CARTESIAN_POINT ( 'NONE',  ( 51.13139720814419320, 27.49999999999988987, -15.00000000000000000 ) ) ;
#29629 = ORIENTED_EDGE ( 'NONE', *, *, #32909, .F. ) ;
#29630 = CIRCLE ( 'NONE', #3305, 2.000000000000000000 ) ;
#29631 = VERTEX_POINT ( 'NONE', #24927 ) ;
#29632 = CIRCLE ( 'NONE', #923, 2.000000000000001776 ) ;
#29633 = DIRECTION ( 'NONE',  ( -0.1391731009600657432, 0.000000000000000000, 0.9902680687415703620 ) ) ;
#29634 = AXIS2_PLACEMENT_3D ( 'NONE', #23781, #20966, #3717 ) ;
#29635 = ORIENTED_EDGE ( 'NONE', *, *, #17001, .F. ) ;
#29636 = DIRECTION ( 'NONE',  ( 1.000000000000000000, 0.000000000000000000, 0.000000000000000000 ) ) ;
#29637 = EDGE_CURVE ( 'NONE', #24803, #29568, #10677, .T. ) ;
#29638 = DIRECTION ( 'NONE',  ( 0.000000000000000000, 0.000000000000000000, 1.000000000000000000 ) ) ;
#29639 = CARTESIAN_POINT ( 'NONE',  ( 90.60231327712337190, 15.97563234535636134, 12.49999999999999822 ) ) ;
#29640 = DIRECTION ( 'NONE',  ( 1.000000000000000000, 0.000000000000000000, 0.000000000000000000 ) ) ;
#29641 = DIRECTION ( 'NONE',  ( 0.000000000000000000, 0.000000000000000000, -1.000000000000000000 ) ) ;
#29642 = ORIENTED_EDGE ( 'NONE', *, *, #16263, .F. ) ;
#29643 = CARTESIAN_POINT ( 'NONE',  ( 69.99999662536839651, 34.64101615137758472, 17.49999999999999645 ) ) ;
#29644 = CIRCLE ( 'NONE', #17109, 2.000000000000001776 ) ;
#29645 = AXIS2_PLACEMENT_3D ( 'NONE', #254, #12052, #9457 ) ;
#29646 = CARTESIAN_POINT ( 'NONE',  ( 47.63139720814418610, 27.49999999999988987, -10.00000000000000178 ) ) ;
#29647 = ORIENTED_EDGE ( 'NONE', *, *, #31504, .T. ) ;
#29648 = DIRECTION ( 'NONE',  ( 0.000000000000000000, -0.000000000000000000, 1.000000000000000000 ) ) ;
#29649 = LINE ( 'NONE', #4354, #22563 ) ;
#29650 = LINE ( 'NONE', #3981, #28762 ) ;
#29651 = ORIENTED_EDGE ( 'NONE', *, *, #33732, .F. ) ;
#29652 = EDGE_LOOP ( 'NONE', ( #28896, #9980 ) ) ;
#29653 = VECTOR ( 'NONE', #35751, 1000.000000000000000 ) ;
#29654 = DIRECTION ( 'NONE',  ( 0.000000000000000000, 0.000000000000000000, 1.000000000000000000 ) ) ;
#29655 = DIRECTION ( 'NONE',  ( 0.000000000000000000, 0.000000000000000000, 1.000000000000000000 ) ) ;
#29656 = CIRCLE ( 'NONE', #15894, 3.500000000000003109 ) ;
#29657 = FACE_OUTER_BOUND ( 'NONE', #28660, .T. ) ;
#29658 = EDGE_LOOP ( 'NONE', ( #13982, #14906, #12728, #18843 ) ) ;
#29659 = ORIENTED_EDGE ( 'NONE', *, *, #19618, .T. ) ;
#29660 = VERTEX_POINT ( 'NONE', #25469 ) ;
#29661 = EDGE_CURVE ( 'NONE', #35979, #10417, #22554, .T. ) ;
#29662 = AXIS2_PLACEMENT_3D ( 'NONE', #34180, #8648, #14468 ) ;
#29663 = AXIS2_PLACEMENT_3D ( 'NONE', #29618, #20621, #32259 ) ;
#29664 = EDGE_CURVE ( 'NONE', #27343, #32462, #31099, .T. ) ;
#29665 = CARTESIAN_POINT ( 'NONE',  ( -61.53067111003215217, 72.28378166042038799, -4.999999999999997335 ) ) ;
#29666 = EDGE_LOOP ( 'NONE', ( #27353, #13904, #1229, #11596, #31553 ) ) ;
#29667 = EDGE_LOOP ( 'NONE', ( #10620, #35875 ) ) ;
#29668 = CARTESIAN_POINT ( 'NONE',  ( -55.00000337463110611, -43.30127018922202353, -5.000000000000000000 ) ) ;
#29669 = ORIENTED_EDGE ( 'NONE', *, *, #12629, .T. ) ;
#29670 = ORIENTED_EDGE ( 'NONE', *, *, #8035, .T. ) ;
#29671 = CONICAL_SURFACE ( 'NONE', #18907, 4.999999999999997335, 0.9110539511682894664 ) ;
#29672 = EDGE_CURVE ( 'NONE', #35319, #20996, #17184, .T. ) ;
#29673 = CARTESIAN_POINT ( 'NONE',  ( 64.99999662536839651, 60.62177826491078747, 17.49999999999999645 ) ) ;
#29674 = CARTESIAN_POINT ( 'NONE',  ( 70.47608876694671665, 59.13646009116074964, -49.22241343995293761 ) ) ;
#29675 = EDGE_LOOP ( 'NONE', ( #26449, #17288, #19041, #5605 ) ) ;
#29676 = ORIENTED_EDGE ( 'NONE', *, *, #257, .F. ) ;
#29677 = CARTESIAN_POINT ( 'NONE',  ( 3.000000000000000888, 0.000000000000000000, -25.03750572909317285 ) ) ;
#29678 = CARTESIAN_POINT ( 'NONE',  ( -35.00000337463116296, -60.62177826491080168, 17.49999999999999645 ) ) ;
#29679 = CIRCLE ( 'NONE', #975, 2.000000000000001776 ) ;
#29680 = CYLINDRICAL_SURFACE ( 'NONE', #30037, 45.00000000000000000 ) ;
#29681 = CARTESIAN_POINT ( 'NONE',  ( -73.00000337463097821, 43.30127018922197379, 17.49999999999999645 ) ) ;
#29682 = AXIS2_PLACEMENT_3D ( 'NONE', #22014, #19217, #7219 ) ;
#29683 = VERTEX_POINT ( 'NONE', #9092 ) ;
#29684 = DIRECTION ( 'NONE',  ( 0.000000000000000000, 0.000000000000000000, -1.000000000000000000 ) ) ;
#29685 = CARTESIAN_POINT ( 'NONE',  ( 28.99999999999998934, 103.4105893997321743, 18.49999999999999645 ) ) ;
#29686 = ORIENTED_EDGE ( 'NONE', *, *, #19421, .T. ) ;
#29687 = EDGE_CURVE ( 'NONE', #34734, #14264, #30338, .T. ) ;
#29688 = DIRECTION ( 'NONE',  ( 0.000000000000000000, 0.000000000000000000, 1.000000000000000000 ) ) ;
#29689 = CIRCLE ( 'NONE', #6325, 3.000000000000005773 ) ;
#29690 = STYLED_ITEM ( 'NONE', ( #31470 ), #29583 ) ;
#29691 = DIRECTION ( 'NONE',  ( -0.000000000000000000, -0.000000000000000000, 1.000000000000000000 ) ) ;
#29692 = DIRECTION ( 'NONE',  ( -1.000000000000000000, 0.000000000000000000, 0.000000000000000000 ) ) ;
#29693 = CIRCLE ( 'NONE', #24332, 6.000000000000005329 ) ;
#29694 = CARTESIAN_POINT ( 'NONE',  ( -55.00000337463109901, -60.62177826491083010, -9.999999999999998224 ) ) ;
#29695 = AXIS2_PLACEMENT_3D ( 'NONE', #31942, #6280, #1582 ) ;
#29696 = CIRCLE ( 'NONE', #4590, 33.00000000000001421 ) ;
#29697 = FACE_OUTER_BOUND ( 'NONE', #19173, .T. ) ;
#29698 = CARTESIAN_POINT ( 'NONE',  ( -2.778182860043012958, -66.86787810013035482, -4.999999999999997335 ) ) ;
#29699 = ORIENTED_EDGE ( 'NONE', *, *, #25134, .T. ) ;
#29700 = CARTESIAN_POINT ( 'NONE',  ( -80.00000337463094979, 34.64101615137757051, -5.000000000000000000 ) ) ;
#29701 = CARTESIAN_POINT ( 'NONE',  ( -48.00000337463109190, 51.96152422706637708, -9.999999999999998224 ) ) ;
#29702 = DIRECTION ( 'NONE',  ( 0.000000000000000000, 0.000000000000000000, 1.000000000000000000 ) ) ;
#29703 = ORIENTED_EDGE ( 'NONE', *, *, #9812, .F. ) ;
#29704 = CIRCLE ( 'NONE', #25519, 2.000000000000001776 ) ;
#29705 = VERTEX_POINT ( 'NONE', #13670 ) ;
#29706 = ORIENTED_EDGE ( 'NONE', *, *, #7833, .F. ) ;
#29707 = ADVANCED_FACE ( 'NONE', ( #33735 ), #5237, .F. ) ;
#29708 = DIRECTION ( 'NONE',  ( -1.000000000000000000, 0.000000000000000000, 0.000000000000000000 ) ) ;
#29709 = CARTESIAN_POINT ( 'NONE',  ( 64.99999662536841072, -25.98076211353320275, 17.49999999999999645 ) ) ;
#29710 = CARTESIAN_POINT ( 'NONE',  ( 70.47608876694671665, 59.13646009116074964, 12.49999999999999822 ) ) ;
#29711 = CIRCLE ( 'NONE', #2181, 2.000000000000001776 ) ;
#29712 = CARTESIAN_POINT ( 'NONE',  ( 74.99999662536835388, -43.30127018922199511, -9.999999999999998224 ) ) ;
#29713 = AXIS2_PLACEMENT_3D ( 'NONE', #11605, #26608, #739 ) ;
#29714 = FACE_OUTER_BOUND ( 'NONE', #7405, .T. ) ;
#29715 = VERTEX_POINT ( 'NONE', #30553 ) ;
#29716 = LINE ( 'NONE', #3849, #22737 ) ;
#29717 = ADVANCED_FACE ( 'NONE', ( #36904 ), #33564, .F. ) ;
#29718 = EDGE_LOOP ( 'NONE', ( #30021, #5653 ) ) ;
#29719 = FACE_BOUND ( 'NONE', #1397, .T. ) ;
#29720 = AXIS2_PLACEMENT_3D ( 'NONE', #1786, #33085, #4958 ) ;
#29721 = CIRCLE ( 'NONE', #384, 2.000000000000001776 ) ;
#29722 = CIRCLE ( 'NONE', #17187, 3.500000000000003109 ) ;
#29723 = AXIS2_PLACEMENT_3D ( 'NONE', #33609, #8463, #7911 ) ;
#29724 = EDGE_CURVE ( 'NONE', #22792, #17282, #29160, .T. ) ;
#29725 = CARTESIAN_POINT ( 'NONE',  ( -5.000000000000000888, -2.886751345948162406, -3.984345921091775100 ) ) ;
#29726 = DIRECTION ( 'NONE',  ( 0.000000000000000000, 0.000000000000000000, -1.000000000000000000 ) ) ;
#29727 = DIRECTION ( 'NONE',  ( -0.000000000000000000, 1.000000000000000000, 0.000000000000000000 ) ) ;
#29728 = ORIENTED_EDGE ( 'NONE', *, *, #24949, .T. ) ;
#29729 = DIRECTION ( 'NONE',  ( -0.000000000000000000, -0.000000000000000000, 1.000000000000000000 ) ) ;
#29730 = CONTEXT_DEPENDENT_SHAPE_REPRESENTATION ( #28584, #33481 ) ;
#29731 = LINE ( 'NONE', #9691, #18906 ) ;
#29732 = CYLINDRICAL_SURFACE ( 'NONE', #36540, 2.000000000000001776 ) ;
#29733 = CARTESIAN_POINT ( 'NONE',  ( 42.97377950131527058, 96.90768712682506703, 18.49999999999999645 ) ) ;
#29734 = ORIENTED_EDGE ( 'NONE', *, *, #9003, .T. ) ;
#29735 = CARTESIAN_POINT ( 'NONE',  ( 44.99999662536851019, -60.62177826491080168, 12.50000000000000000 ) ) ;
#29736 = DIRECTION ( 'NONE',  ( 0.000000000000000000, 0.000000000000000000, 1.000000000000000000 ) ) ;
#29737 = LINE ( 'NONE', #24129, #36945 ) ;
#29738 = CIRCLE ( 'NONE', #16591, 2.000000000000001776 ) ;
#29739 = ORIENTED_EDGE ( 'NONE', *, *, #17239, .T. ) ;
#29740 = ADVANCED_FACE ( 'NONE', ( #8032 ), #16302, .F. ) ;
#29741 = ORIENTED_EDGE ( 'NONE', *, *, #23623, .T. ) ;
#29742 = AXIS2_PLACEMENT_3D ( 'NONE', #3283, #27906, #8419 ) ;
#29743 = ORIENTED_EDGE ( 'NONE', *, *, #16320, .F. ) ;
#29744 = CARTESIAN_POINT ( 'NONE',  ( -47.00000337463111322, 60.62177826491077326, 12.50000000000000000 ) ) ;
#29745 = FACE_OUTER_BOUND ( 'NONE', #17507, .T. ) ;
#29746 = CIRCLE ( 'NONE', #23181, 2.000000000000001776 ) ;
#29747 = EDGE_CURVE ( 'NONE', #29309, #20458, #21265, .T. ) ;
#29748 = VECTOR ( 'NONE', #4315, 1000.000000000000000 ) ;
#29749 = CARTESIAN_POINT ( 'NONE',  ( 52.39915983220795681, 35.19434990244919703, -4.999999999999997335 ) ) ;
#29750 = CIRCLE ( 'NONE', #16601, 2.000000000000001776 ) ;
#29751 = CIRCLE ( 'NONE', #34566, 2.000000000000001776 ) ;
#29752 = EDGE_CURVE ( 'NONE', #8095, #32403, #36966, .T. ) ;
#29753 = CARTESIAN_POINT ( 'NONE',  ( 56.67878100130369035, -27.78182860042797131, -49.86348611802629449 ) ) ;
#29754 = FACE_OUTER_BOUND ( 'NONE', #684, .T. ) ;
#29755 = CIRCLE ( 'NONE', #13602, 2.000000000000001776 ) ;
#29756 = CARTESIAN_POINT ( 'NONE',  ( -106.7731239591695669, -98.28784258492920856, 32.50000000000000000 ) ) ;
#29757 = ORIENTED_EDGE ( 'NONE', *, *, #31974, .T. ) ;
#29758 = ORIENTED_EDGE ( 'NONE', *, *, #33113, .F. ) ;
#29759 = CYLINDRICAL_SURFACE ( 'NONE', #25481, 2.000000000000001776 ) ;
#29760 = CARTESIAN_POINT ( 'NONE',  ( -5.000003374631269537, -77.94228634059960825, 12.50000000000000000 ) ) ;
#29761 = ORIENTED_EDGE ( 'NONE', *, *, #37060, .F. ) ;
#29762 = CARTESIAN_POINT ( 'NONE',  ( -43.00000337463111322, 77.94228634059959404, 12.50000000000000000 ) ) ;
#29763 = ORIENTED_EDGE ( 'NONE', *, *, #17756, .T. ) ;
#29764 = VECTOR ( 'NONE', #21812, 1000.000000000000000 ) ;
#29765 = CYLINDRICAL_SURFACE ( 'NONE', #5125, 2.000000000000001776 ) ;
#29766 = CIRCLE ( 'NONE', #17778, 2.000000000000001776 ) ;
#29767 = ADVANCED_FACE ( 'NONE', ( #662 ), #9661, .F. ) ;
#29768 = AXIS2_PLACEMENT_3D ( 'NONE', #16221, #4950, #16388 ) ;
#29769 = CARTESIAN_POINT ( 'NONE',  ( 0.000000000000000000, 0.000000000000000000, -5.000000000000000000 ) ) ;
#29770 = ORIENTED_EDGE ( 'NONE', *, *, #27714, .F. ) ;
#29771 = VERTEX_POINT ( 'NONE', #21086 ) ;
#29772 = DIRECTION ( 'NONE',  ( 1.000000000000000000, 0.000000000000000000, 0.000000000000000000 ) ) ;
#29773 = ORIENTED_EDGE ( 'NONE', *, *, #36728, .T. ) ;
#29775 =( GEOMETRIC_REPRESENTATION_CONTEXT ( 3 ) GLOBAL_UNCERTAINTY_ASSIGNED_CONTEXT ( ( #34299 ) ) GLOBAL_UNIT_ASSIGNED_CONTEXT ( ( #8062, #14248, #14043 ) ) REPRESENTATION_CONTEXT ( 'NONE', 'WORKASPACE' ) );
#29774 = SURFACE_STYLE_USAGE ( .BOTH. , #35249 ) ;
#29776 = CIRCLE ( 'NONE', #2253, 2.000000000000001776 ) ;
#29777 = CARTESIAN_POINT ( 'NONE',  ( -3.357433326862113265, 3.835087656846187798, -0.07080520455421240866 ) ) ;
#29778 = VECTOR ( 'NONE', #9072, 1000.000000000000000 ) ;
#29779 = CARTESIAN_POINT ( 'NONE',  ( 29.99999662536857770, -69.28203230275519786, -9.999999999999998224 ) ) ;
#29780 = CARTESIAN_POINT ( 'NONE',  ( -34.00000000000027711, -58.88972745734168512, -4.999999999999997335 ) ) ;
#29781 = ORIENTED_EDGE ( 'NONE', *, *, #4034, .F. ) ;
#29782 = ORIENTED_EDGE ( 'NONE', *, *, #28216, .F. ) ;
#29783 = AXIS2_PLACEMENT_3D ( 'NONE', #3866, #8953, #14754 ) ;
#29784 = EDGE_LOOP ( 'NONE', ( #25074, #10541 ) ) ;
#29785 = VERTEX_POINT ( 'NONE', #35537 ) ;
#29786 = EDGE_CURVE ( 'NONE', #35919, #29281, #11803, .T. ) ;
#29787 = VERTEX_POINT ( 'NONE', #15659 ) ;
#29788 = CARTESIAN_POINT ( 'NONE',  ( 89.99999662536828282, 0.000000000000000000, -9.999999999999998224 ) ) ;
#29789 = AXIS2_PLACEMENT_3D ( 'NONE', #27422, #30420, #16739 ) ;
#29790 = CARTESIAN_POINT ( 'NONE',  ( -12.00000337463125000, -86.60254037844400443, -5.000000000000000000 ) ) ;
#29791 = EDGE_CURVE ( 'NONE', #24619, #28688, #13617, .T. ) ;
#29792 = EDGE_LOOP ( 'NONE', ( #6910, #1989, #28067, #20553, #26793 ) ) ;
#29793 = CIRCLE ( 'NONE', #13640, 2.000000000000001776 ) ;
#29795 = AXIS2_PLACEMENT_3D ( 'NONE', #6055, #14857, #9213 ) ;
#29794 = CARTESIAN_POINT ( 'NONE',  ( -9.999999999999971578, -3.946495907847236140E-14, -5.700000000000000178 ) ) ;
#29796 = DIRECTION ( 'NONE',  ( -1.000000000000000000, 0.000000000000000000, 0.000000000000000000 ) ) ;
#29797 = DIRECTION ( 'NONE',  ( -1.000000000000000000, 0.000000000000000000, 0.000000000000000000 ) ) ;
#29798 = VERTEX_POINT ( 'NONE', #7030 ) ;
#29799 = CYLINDRICAL_SURFACE ( 'NONE', #30223, 2.000000000000001776 ) ;
#29800 = VECTOR ( 'NONE', #12900, 1000.000000000000000 ) ;
#29801 = EDGE_CURVE ( 'NONE', #25394, #31695, #15409, .T. ) ;
#29802 = CYLINDRICAL_SURFACE ( 'NONE', #28184, 27.00000000000001066 ) ;
#29803 = CIRCLE ( 'NONE', #14846, 2.000000000000001776 ) ;
#29804 = CARTESIAN_POINT ( 'NONE',  ( 102.5304832720496080, 102.5304832720492527, 32.50000000000000000 ) ) ;
#29805 = ORIENTED_EDGE ( 'NONE', *, *, #4738, .F. ) ;
#29806 = CARTESIAN_POINT ( 'NONE',  ( 87.83969979969882047, 14.80603122773025504, -49.86561046011506448 ) ) ;
#29807 = ADVANCED_FACE ( 'NONE', ( #12815 ), #34975, .F. ) ;
#29808 = CARTESIAN_POINT ( 'NONE',  ( 5.999999999999998224, 0.000000000000000000, 0.000000000000000000 ) ) ;
#29809 = EDGE_CURVE ( 'NONE', #30112, #25842, #8216, .T. ) ;
#29810 = ORIENTED_EDGE ( 'NONE', *, *, #5029, .F. ) ;
#29811 = ORIENTED_EDGE ( 'NONE', *, *, #20060, .T. ) ;
#29812 = VECTOR ( 'NONE', #14299, 1000.000000000000000 ) ;
#29813 = DIRECTION ( 'NONE',  ( 1.000000000000000000, 0.000000000000000000, 0.000000000000000000 ) ) ;
#29814 = DIRECTION ( 'NONE',  ( -0.000000000000000000, -0.000000000000000000, 1.000000000000000000 ) ) ;
#29815 = CARTESIAN_POINT ( 'NONE',  ( -69.61831313460106685, -36.60425647305652319, -5.000000000000000000 ) ) ;
#29816 = CARTESIAN_POINT ( 'NONE',  ( 70.80619744048946984, -84.18124734178287838, 32.50000000000000000 ) ) ;
#29817 = VERTEX_POINT ( 'NONE', #4030 ) ;
#29818 = AXIS2_PLACEMENT_3D ( 'NONE', #13611, #19422, #5178 ) ;
#29819 = ADVANCED_FACE ( 'NONE', ( #9272 ), #3665, .T. ) ;
#29820 = CARTESIAN_POINT ( 'NONE',  ( 54.99999662536844625, 43.30127018922198801, -9.999999999999998224 ) ) ;
#29821 = EDGE_CURVE ( 'NONE', #24381, #7306, #29901, .T. ) ;
#29822 = DIRECTION ( 'NONE',  ( 0.000000000000000000, 0.000000000000000000, 1.000000000000000000 ) ) ;
#29823 = ADVANCED_FACE ( 'NONE', ( #12456 ), #35173, .T. ) ;
#29824 = VERTEX_POINT ( 'NONE', #6278 ) ;
#29825 = EDGE_CURVE ( 'NONE', #34239, #24664, #12990, .T. ) ;
#29826 = EDGE_CURVE ( 'NONE', #33879, #24561, #23790, .T. ) ;
#29827 = VECTOR ( 'NONE', #24666, 1000.000000000000000 ) ;
#29828 = AXIS2_PLACEMENT_3D ( 'NONE', #31487, #5825, #6017 ) ;
#29829 = CARTESIAN_POINT ( 'NONE',  ( 19.99999662536858835, 69.28203230275516944, -9.999999999999998224 ) ) ;
#29830 = ORIENTED_EDGE ( 'NONE', *, *, #9460, .F. ) ;
#29831 = AXIS2_PLACEMENT_3D ( 'NONE', #22841, #33722, #2417 ) ;
#29832 = DIRECTION ( 'NONE',  ( -1.000000000000000000, 0.000000000000000000, 0.000000000000000000 ) ) ;
#29833 = CARTESIAN_POINT ( 'NONE',  ( -48.00000337463109190, 69.28203230275518365, -9.999999999999998224 ) ) ;
#29834 = CIRCLE ( 'NONE', #2303, 6.532899837730827386 ) ;
#29835 = DIRECTION ( 'NONE',  ( -1.000000000000000000, 0.000000000000000000, 0.000000000000000000 ) ) ;
#29836 = VERTEX_POINT ( 'NONE', #26712 ) ;
#29837 = ORIENTED_EDGE ( 'NONE', *, *, #11274, .F. ) ;
#29838 = VECTOR ( 'NONE', #15815, 1000.000000000000000 ) ;
#29839 = ORIENTED_EDGE ( 'NONE', *, *, #12379, .T. ) ;
#29840 = CARTESIAN_POINT ( 'NONE',  ( -6.123233995736731770E-16, 145.0000000000000568, 32.55002500000000509 ) ) ;
#29841 = CARTESIAN_POINT ( 'NONE',  ( 84.99999662536831124, -8.660254037844397956, 12.50000000000000000 ) ) ;
#29842 = FACE_OUTER_BOUND ( 'NONE', #19845, .T. ) ;
#29843 = DIRECTION ( 'NONE',  ( 0.000000000000000000, 0.000000000000000000, -1.000000000000000000 ) ) ;
#29844 = AXIS2_PLACEMENT_3D ( 'NONE', #23472, #28893, #25914 ) ;
#29845 = DIRECTION ( 'NONE',  ( -0.000000000000000000, -0.000000000000000000, 1.000000000000000000 ) ) ;
#29846 = ORIENTED_EDGE ( 'NONE', *, *, #32885, .F. ) ;
#29847 = DIRECTION ( 'NONE',  ( 0.000000000000000000, 0.000000000000000000, 1.000000000000000000 ) ) ;
#29848 = PRODUCT_DEFINITION_SHAPE ( 'NONE', 'NONE',  #37137 ) ;
#29849 = CARTESIAN_POINT ( 'NONE',  ( 108.3061974404897825, -19.22934205795014151, 32.50000000000000000 ) ) ;
#29850 = VECTOR ( 'NONE', #31668, 1000.000000000000000 ) ;
#29851 = PRESENTATION_STYLE_ASSIGNMENT (( #18425 ) ) ;
#29852 = ORIENTED_EDGE ( 'NONE', *, *, #4764, .F. ) ;
#29853 = DIRECTION ( 'NONE',  ( 0.000000000000000000, 0.000000000000000000, -1.000000000000000000 ) ) ;
#29854 = CIRCLE ( 'NONE', #35288, 2.000000000000001776 ) ;
#29855 = FACE_OUTER_BOUND ( 'NONE', #36533, .T. ) ;
#29856 = CARTESIAN_POINT ( 'NONE',  ( -8.000003374631287301, 69.28203230275516944, -9.999999999999998224 ) ) ;
#29857 = ORIENTED_EDGE ( 'NONE', *, *, #2060, .F. ) ;
#29858 = EDGE_LOOP ( 'NONE', ( #18564, #31137, #5836, #20522, #8601, #18363, #8389, #9551, #5207, #35315, #1017, #20172, #13988, #13434, #8022, #26359 ) ) ;
#29859 = CIRCLE ( 'NONE', #4120, 2.000000000000001776 ) ;
#29860 = AXIS2_PLACEMENT_3D ( 'NONE', #8886, #17335, #28760 ) ;
#29861 = CARTESIAN_POINT ( 'NONE',  ( 0.000000000000000000, 0.000000000000000000, -10.00000000000000000 ) ) ;
#29862 = CARTESIAN_POINT ( 'NONE',  ( -6.000000000000000000, 145.0000000000000568, 32.50000000000000000 ) ) ;
#29863 = DIRECTION ( 'NONE',  ( 1.000000000000000000, 0.000000000000000000, 0.000000000000000000 ) ) ;
#29864 = ORIENTED_EDGE ( 'NONE', *, *, #7872, .F. ) ;
#29865 = EDGE_LOOP ( 'NONE', ( #15663, #11128, #14262, #1115 ) ) ;
#29866 = ORIENTED_EDGE ( 'NONE', *, *, #3802, .T. ) ;
#29867 = CIRCLE ( 'NONE', #2957, 33.00000000000001421 ) ;
#29868 = EDGE_CURVE ( 'NONE', #21598, #7182, #23724, .T. ) ;
#29869 = CARTESIAN_POINT ( 'NONE',  ( 9.999996625368625658, 86.60254037844397601, -9.999999999999998224 ) ) ;
#29870 = ORIENTED_EDGE ( 'NONE', *, *, #4867, .F. ) ;
#29871 = EDGE_CURVE ( 'NONE', #8170, #17344, #4039, .T. ) ;
#29872 = ORIENTED_EDGE ( 'NONE', *, *, #15793, .T. ) ;
#29873 = DIRECTION ( 'NONE',  ( 0.000000000000000000, 0.000000000000000000, -1.000000000000000000 ) ) ;
#29874 = VERTEX_POINT ( 'NONE', #20917 ) ;
#29875 = VERTEX_POINT ( 'NONE', #1030 ) ;
#29876 = CARTESIAN_POINT ( 'NONE',  ( -67.00000337463104927, -25.98076211353322051, 17.49999999999999645 ) ) ;
#29877 = AXIS2_PLACEMENT_3D ( 'NONE', #36353, #8021, #1850 ) ;
#29878 = DIRECTION ( 'NONE',  ( 1.000000000000000000, 0.000000000000000000, 0.000000000000000000 ) ) ;
#29879 = ORIENTED_EDGE ( 'NONE', *, *, #10057, .F. ) ;
#29880 = ORIENTED_EDGE ( 'NONE', *, *, #13549, .T. ) ;
#29881 = CARTESIAN_POINT ( 'NONE',  ( 19.99999662536861678, -69.28203230275519786, -9.999999999999998224 ) ) ;
#29882 = AXIS2_PLACEMENT_3D ( 'NONE', #2666, #36251, #28345 ) ;
#29883 = DIRECTION ( 'NONE',  ( -1.000000000000000000, 0.000000000000000000, 0.000000000000000000 ) ) ;
#29884 = LINE ( 'NONE', #18073, #5508 ) ;
#29885 = CARTESIAN_POINT ( 'NONE',  ( -5.000000000000000888, -3.083558429163938630, -4.289113568008026789 ) ) ;
#29886 = ORIENTED_EDGE ( 'NONE', *, *, #13552, .T. ) ;
#29887 = DIRECTION ( 'NONE',  ( 1.000000000000000000, 0.000000000000000000, 0.000000000000000000 ) ) ;
#29888 = AXIS2_PLACEMENT_3D ( 'NONE', #18492, #16046, #29915 ) ;
#29889 = ORIENTED_EDGE ( 'NONE', *, *, #20828, .F. ) ;
#29890 = CARTESIAN_POINT ( 'NONE',  ( -51.68138994340220904, 113.8157894736842053, 32.50000000000000000 ) ) ;
#29891 = DIRECTION ( 'NONE',  ( 1.000000000000000000, 0.000000000000000000, 0.000000000000000000 ) ) ;
#29892 = CARTESIAN_POINT ( 'NONE',  ( 59.13646009116148150, -70.47608876694609137, 12.49999999999999822 ) ) ;
#29893 = CARTESIAN_POINT ( 'NONE',  ( -52.39915983220772233, -35.19434990244957362, 12.49999999999999822 ) ) ;
#29894 = VECTOR ( 'NONE', #25441, 1000.000000000000000 ) ;
#29895 = EDGE_CURVE ( 'NONE', #35112, #13025, #19223, .T. ) ;
#29896 = FACE_OUTER_BOUND ( 'NONE', #37061, .T. ) ;
#29897 = CARTESIAN_POINT ( 'NONE',  ( 63.10544158860312081, 59.98094972882071829, 12.50000000000000000 ) ) ;
#29898 = CARTESIAN_POINT ( 'NONE',  ( 64.99999662536841072, 25.98076211353318854, 12.50000000000000000 ) ) ;
#29899 = CIRCLE ( 'NONE', #22708, 3.000000000000002665 ) ;
#29900 = VERTEX_POINT ( 'NONE', #10386 ) ;
#29901 = LINE ( 'NONE', #20516, #3418 ) ;
#29902 = DIRECTION ( 'NONE',  ( 0.000000000000000000, 0.000000000000000000, 1.000000000000000000 ) ) ;
#29903 = FACE_OUTER_BOUND ( 'NONE', #31210, .T. ) ;
#29904 = VERTEX_POINT ( 'NONE', #32906 ) ;
#29905 = EDGE_CURVE ( 'NONE', #25059, #16555, #1947, .T. ) ;
#29906 = ORIENTED_EDGE ( 'NONE', *, *, #36925, .F. ) ;
#29907 = AXIS2_PLACEMENT_3D ( 'NONE', #33757, #22871, #22693 ) ;
#29908 = ORIENTED_EDGE ( 'NONE', *, *, #34515, .T. ) ;
#29909 = VECTOR ( 'NONE', #2967, 1000.000000000000000 ) ;
#29910 = DIRECTION ( 'NONE',  ( 0.000000000000000000, 1.224646799147351482E-16, 1.000000000000000000 ) ) ;
#29911 = CARTESIAN_POINT ( 'NONE',  ( -13.89091430021420237, -62.33939050065180254, 12.49999999999999822 ) ) ;
#29912 = DIRECTION ( 'NONE',  ( -1.000000000000000000, -0.000000000000000000, -0.000000000000000000 ) ) ;
#29913 = VECTOR ( 'NONE', #36545, 1000.000000000000000 ) ;
#29914 = EDGE_LOOP ( 'NONE', ( #4317, #22573, #36403, #32801 ) ) ;
#29915 = DIRECTION ( 'NONE',  ( 1.000000000000000000, 0.000000000000000000, 0.000000000000000000 ) ) ;
#29916 = DIRECTION ( 'NONE',  ( 3.554796214472773777E-16, 1.000000000000000000, -0.000000000000000000 ) ) ;
#29917 = ORIENTED_EDGE ( 'NONE', *, *, #33103, .T. ) ;
#29918 = EDGE_CURVE ( 'NONE', #6451, #16018, #1038, .T. ) ;
#29919 = LINE ( 'NONE', #19236, #13168 ) ;
#29920 = ORIENTED_EDGE ( 'NONE', *, *, #5711, .T. ) ;
#29921 = FACE_BOUND ( 'NONE', #18938, .T. ) ;
#29922 = AXIS2_PLACEMENT_3D ( 'NONE', #9844, #18673, #15674 ) ;
#29923 = CIRCLE ( 'NONE', #34117, 3.000000000000002665 ) ;
#29924 = DIRECTION ( 'NONE',  ( 0.000000000000000000, 0.000000000000000000, 1.000000000000000000 ) ) ;
#29925 = CARTESIAN_POINT ( 'NONE',  ( -7.000003374631269537, -77.94228634059960825, -5.000000000000000000 ) ) ;
#29926 = CARTESIAN_POINT ( 'NONE',  ( -47.63139720814380951, 27.50000000000055422, -10.00000000000000178 ) ) ;
#29927 = AXIS2_PLACEMENT_3D ( 'NONE', #11114, #29462, #8867 ) ;
#29928 = ORIENTED_EDGE ( 'NONE', *, *, #19887, .T. ) ;
#29929 = DIRECTION ( 'NONE',  ( -1.000000000000000000, -2.492861883996299315E-14, 0.000000000000000000 ) ) ;
#29930 = CONTEXT_DEPENDENT_SHAPE_REPRESENTATION ( #16377, #18491 ) ;
#29931 = PLANE ( 'NONE',  #15880 ) ;
#29932 = CIRCLE ( 'NONE', #5407, 2.000000000000001776 ) ;
#29933 = DIRECTION ( 'NONE',  ( 0.000000000000000000, 0.000000000000000000, 1.000000000000000000 ) ) ;
#29934 = FACE_OUTER_BOUND ( 'NONE', #11894, .T. ) ;
#29935 = EDGE_CURVE ( 'NONE', #20586, #18237, #8821, .T. ) ;
#29936 = VERTEX_POINT ( 'NONE', #13376 ) ;
#29937 = DIRECTION ( 'NONE',  ( 1.000000000000000000, 0.000000000000000000, 0.000000000000000000 ) ) ;
#29938 = CIRCLE ( 'NONE', #7819, 0.2500000000000002220 ) ;
#29939 = CARTESIAN_POINT ( 'NONE',  ( -12.00000337463125000, -86.60254037844400443, -9.999999999999998224 ) ) ;
#29940 = CARTESIAN_POINT ( 'NONE',  ( -3.000003374631308173, 77.94228634059957983, -9.999999999999998224 ) ) ;
#29941 = EDGE_CURVE ( 'NONE', #24063, #31658, #1779, .T. ) ;
#29942 = ORIENTED_EDGE ( 'NONE', *, *, #26855, .F. ) ;
#29943 = ORIENTED_EDGE ( 'NONE', *, *, #14019, .F. ) ;
#29944 = EDGE_CURVE ( 'NONE', #32725, #18729, #16007, .T. ) ;
#29945 = CARTESIAN_POINT ( 'NONE',  ( -41.00000000000000000, 103.4105893997321886, 27.49999999999999645 ) ) ;
#29946 = DIRECTION ( 'NONE',  ( 0.000000000000000000, 0.000000000000000000, 1.000000000000000000 ) ) ;
#29947 = CIRCLE ( 'NONE', #16796, 2.000000000000001776 ) ;
#29948 = CARTESIAN_POINT ( 'NONE',  ( -5.000000000000000000, 25.00000000000000000, -15.00000000000000000 ) ) ;
#29949 = ADVANCED_FACE ( 'NONE', ( #2130 ), #16579, .T. ) ;
#29950 = ORIENTED_EDGE ( 'NONE', *, *, #19934, .T. ) ;
#29951 = CIRCLE ( 'NONE', #12593, 3.000000000000002665 ) ;
#29952 = FACE_OUTER_BOUND ( 'NONE', #33686, .T. ) ;
#29953 = CARTESIAN_POINT ( 'NONE',  ( 0.000000000000000000, 85.61789592134881843, -27.49999999999990408 ) ) ;
#29954 = DIRECTION ( 'NONE',  ( 1.000000000000000000, 0.000000000000000000, 0.000000000000000000 ) ) ;
#29955 = DIRECTION ( 'NONE',  ( 0.000000000000000000, 0.000000000000000000, -1.000000000000000000 ) ) ;
#29956 = ORIENTED_EDGE ( 'NONE', *, *, #30741, .F. ) ;
#29957 = ORIENTED_EDGE ( 'NONE', *, *, #16666, .F. ) ;
#29958 = LINE ( 'NONE', #10267, #1544 ) ;
#29959 = DIRECTION ( 'NONE',  ( 0.000000000000000000, 0.000000000000000000, -1.000000000000000000 ) ) ;
#29960 = ORIENTED_EDGE ( 'NONE', *, *, #15211, .T. ) ;
#29961 = EDGE_CURVE ( 'NONE', #26137, #2878, #17779, .T. ) ;
#29962 = FACE_OUTER_BOUND ( 'NONE', #11872, .T. ) ;
#29963 = EDGE_LOOP ( 'NONE', ( #31677, #11254 ) ) ;
#29964 = CARTESIAN_POINT ( 'NONE',  ( -98.28784258492883907, 106.7731239591698937, 27.50000000000000000 ) ) ;
#29965 = EDGE_CURVE ( 'NONE', #20237, #23192, #10627, .T. ) ;
#29966 = FACE_BOUND ( 'NONE', #28055, .T. ) ;
#29967 = EDGE_LOOP ( 'NONE', ( #6087, #426 ) ) ;
#29968 = VERTEX_POINT ( 'NONE', #10775 ) ;
#29969 = DIRECTION ( 'NONE',  ( 0.000000000000000000, 0.000000000000000000, -1.000000000000000000 ) ) ;
#29970 = ORIENTED_EDGE ( 'NONE', *, *, #31171, .T. ) ;
#29971 = CARTESIAN_POINT ( 'NONE',  ( 0.000000000000000000, 0.000000000000000000, 0.000000000000000000 ) ) ;
#29972 = EDGE_CURVE ( 'NONE', #32493, #21629, #22209, .T. ) ;
#29973 = CARTESIAN_POINT ( 'NONE',  ( 106.7731239591688848, 98.28784258492994752, 32.55002500000000509 ) ) ;
#29974 = CARTESIAN_POINT ( 'NONE',  ( 33.99999999999986500, -58.88972745734191250, -4.999999999999997335 ) ) ;
#29975 = PLANE ( 'NONE',  #20888 ) ;
#29976 = EDGE_CURVE ( 'NONE', #32183, #29787, #17497, .T. ) ;
#29977 = AXIS2_PLACEMENT_3D ( 'NONE', #5428, #27560, #33737 ) ;
#29978 = ORIENTED_EDGE ( 'NONE', *, *, #17980, .T. ) ;
#29979 = DIRECTION ( 'NONE',  ( 0.000000000000000000, 0.000000000000000000, 1.000000000000000000 ) ) ;
#29980 = CARTESIAN_POINT ( 'NONE',  ( 79.99999662536832545, -17.32050807568879591, 12.50000000000000000 ) ) ;
#29981 = VERTEX_POINT ( 'NONE', #30078 ) ;
#29982 = ORIENTED_EDGE ( 'NONE', *, *, #23922, .F. ) ;
#29983 = ORIENTED_EDGE ( 'NONE', *, *, #1129, .F. ) ;
#29984 = CARTESIAN_POINT ( 'NONE',  ( -10.00000337463125000, -86.60254037844400443, -5.000000000000000000 ) ) ;
#29985 = CYLINDRICAL_SURFACE ( 'NONE', #13802, 2.000000000000001776 ) ;
#29986 = ORIENTED_EDGE ( 'NONE', *, *, #32210, .F. ) ;
#29987 = EDGE_CURVE ( 'NONE', #28791, #19268, #16623, .T. ) ;
#29988 = LINE ( 'NONE', #36002, #1369 ) ;
#29989 = DIRECTION ( 'NONE',  ( 0.000000000000000000, 0.000000000000000000, 1.000000000000000000 ) ) ;
#29990 = ORIENTED_EDGE ( 'NONE', *, *, #15312, .F. ) ;
#29991 = DIRECTION ( 'NONE',  ( 0.000000000000000000, 0.000000000000000000, 1.000000000000000000 ) ) ;
#29992 = DIRECTION ( 'NONE',  ( 1.000000000000000000, 0.000000000000000000, 0.000000000000000000 ) ) ;
#29993 = ADVANCED_FACE ( 'NONE', ( #13770 ), #27257, .F. ) ;
#29994 = CARTESIAN_POINT ( 'NONE',  ( -60.00000337463104216, 51.96152422706639129, 17.49999999999999645 ) ) ;
#29995 = DIRECTION ( 'NONE',  ( 0.000000000000000000, 0.000000000000000000, 1.000000000000000000 ) ) ;
#29996 = CARTESIAN_POINT ( 'NONE',  ( -65.00000337463106348, -60.62177826491083010, -5.000000000000000000 ) ) ;
#29997 = DIRECTION ( 'NONE',  ( 1.000000000000000000, 0.000000000000000000, 0.000000000000000000 ) ) ;
#29998 = EDGE_LOOP ( 'NONE', ( #21574, #27178 ) ) ;
#29999 = ORIENTED_EDGE ( 'NONE', *, *, #25158, .T. ) ;
#30000 = CARTESIAN_POINT ( 'NONE',  ( -52.39915983220772233, -35.19434990244957362, 12.49999999999999822 ) ) ;
#30001 = DIRECTION ( 'NONE',  ( 0.000000000000000000, 0.000000000000000000, 1.000000000000000000 ) ) ;
#30002 = AXIS2_PLACEMENT_3D ( 'NONE', #23018, #34467, #11758 ) ;
#30003 = DIRECTION ( 'NONE',  ( 0.000000000000000000, 0.000000000000000000, 1.000000000000000000 ) ) ;
#30004 = CARTESIAN_POINT ( 'NONE',  ( -5.000000000000000000, 2.488344183252603870, -1.689918788536291405 ) ) ;
#30005 = ORIENTED_EDGE ( 'NONE', *, *, #10772, .F. ) ;
#30006 = DIRECTION ( 'NONE',  ( 0.000000000000000000, 0.000000000000000000, 1.000000000000000000 ) ) ;
#30007 = CARTESIAN_POINT ( 'NONE',  ( 0.000000000000000000, 0.000000000000000000, -10.00000000000000000 ) ) ;
#30008 = EDGE_CURVE ( 'NONE', #23662, #6894, #5251, .T. ) ;
#30009 = EDGE_LOOP ( 'NONE', ( #15231, #8924 ) ) ;
#30010 = DIRECTION ( 'NONE',  ( 0.000000000000000000, 0.000000000000000000, 1.000000000000000000 ) ) ;
#30011 = ORIENTED_EDGE ( 'NONE', *, *, #32164, .T. ) ;
#30012 = DIRECTION ( 'NONE',  ( 0.000000000000000000, 0.000000000000000000, 1.000000000000000000 ) ) ;
#30013 = EDGE_CURVE ( 'NONE', #6156, #17794, #9998, .T. ) ;
#30014 = CARTESIAN_POINT ( 'NONE',  ( -46.74666114985175369, -61.59604035298635694, -5.000000000000000000 ) ) ;
#30015 = DIRECTION ( 'NONE',  ( -1.000000000000000000, 0.000000000000000000, 0.000000000000000000 ) ) ;
#30016 = EDGE_CURVE ( 'NONE', #6890, #603, #24476, .T. ) ;
#30017 = ORIENTED_EDGE ( 'NONE', *, *, #11189, .F. ) ;
#30018 = EDGE_LOOP ( 'NONE', ( #11231, #33889, #3178, #20146, #8099 ) ) ;
#30019 = ADVANCED_FACE ( 'NONE', ( #35916 ), #10222, .T. ) ;
#30020 = AXIS2_PLACEMENT_3D ( 'NONE', #15754, #16316, #36017 ) ;
#30021 = ORIENTED_EDGE ( 'NONE', *, *, #27072, .T. ) ;
#30022 = FACE_OUTER_BOUND ( 'NONE', #33000, .T. ) ;
#30023 = CARTESIAN_POINT ( 'NONE',  ( 79.99999662536833966, 17.32050807568879236, 17.49999999999999645 ) ) ;
#30024 = CARTESIAN_POINT ( 'NONE',  ( 81.99999662536833966, -3.469446951953614189E-15, 17.49999999999999645 ) ) ;
#30025 = DIRECTION ( 'NONE',  ( 0.000000000000000000, 0.000000000000000000, 1.000000000000000000 ) ) ;
#30026 = DIRECTION ( 'NONE',  ( 0.000000000000000000, 0.000000000000000000, 1.000000000000000000 ) ) ;
#30027 = ORIENTED_EDGE ( 'NONE', *, *, #915, .T. ) ;
#30028 = CARTESIAN_POINT ( 'NONE',  ( 9.999996625368618552, 69.28203230275516944, 12.50000000000000000 ) ) ;
#30029 = DIRECTION ( 'NONE',  ( 0.000000000000000000, 0.000000000000000000, -1.000000000000000000 ) ) ;
#30030 = ADVANCED_FACE ( 'NONE', ( #33823 ), #20774, .T. ) ;
#30031 = DIRECTION ( 'NONE',  ( 1.000000000000000000, 0.000000000000000000, 0.000000000000000000 ) ) ;
#30032 = EDGE_LOOP ( 'NONE', ( #32001, #26958 ) ) ;
#30033 = CARTESIAN_POINT ( 'NONE',  ( 69.99999662536839651, -17.32050807568879947, -9.999999999999998224 ) ) ;
#30034 = FACE_BOUND ( 'NONE', #9728, .T. ) ;
#30035 = EDGE_LOOP ( 'NONE', ( #557, #9431, #28878, #34178, #16863 ) ) ;
#30036 = EDGE_LOOP ( 'NONE', ( #29957, #481, #36503, #22778 ) ) ;
#30037 = AXIS2_PLACEMENT_3D ( 'NONE', #18460, #30239, #26509 ) ;
#30038 = CARTESIAN_POINT ( 'NONE',  ( 47.04203867989577503, -43.19957991610382919, 12.49999999999999822 ) ) ;
#30039 = CARTESIAN_POINT ( 'NONE',  ( -72.00000337463100664, -17.32050807568882078, -5.000000000000000000 ) ) ;
#30040 = CARTESIAN_POINT ( 'NONE',  ( 124.4080600076931375, 12.15049814296589226, 32.50000000000000000 ) ) ;
#30041 = ORIENTED_EDGE ( 'NONE', *, *, #9671, .F. ) ;
#30042 = AXIS2_PLACEMENT_3D ( 'NONE', #25347, #20078, #28514 ) ;
#30043 = ORIENTED_EDGE ( 'NONE', *, *, #16320, .T. ) ;
#30044 = ORIENTED_EDGE ( 'NONE', *, *, #9126, .T. ) ;
#30045 = CARTESIAN_POINT ( 'NONE',  ( 0.000000000000000000, 0.000000000000000000, 12.49999999999999822 ) ) ;
#30046 = EDGE_CURVE ( 'NONE', #598, #32017, #25589, .T. ) ;
#30047 = ORIENTED_EDGE ( 'NONE', *, *, #14594, .T. ) ;
#30048 = EDGE_CURVE ( 'NONE', #1072, #22136, #8679, .T. ) ;
#30049 = ORIENTED_EDGE ( 'NONE', *, *, #14435, .T. ) ;
#30050 = FACE_BOUND ( 'NONE', #34397, .T. ) ;
#30051 = ORIENTED_EDGE ( 'NONE', *, *, #26492, .F. ) ;
#30052 = ORIENTED_EDGE ( 'NONE', *, *, #10293, .T. ) ;
#30053 = PLANE ( 'NONE',  #2254 ) ;
#30054 = DIRECTION ( 'NONE',  ( -0.000000000000000000, -0.000000000000000000, 1.000000000000000000 ) ) ;
#30055 = VERTEX_POINT ( 'NONE', #14321 ) ;
#30056 = EDGE_LOOP ( 'NONE', ( #11662, #26459, #27811, #15792 ) ) ;
#30057 = EDGE_CURVE ( 'NONE', #32725, #29300, #28910, .T. ) ;
#30058 = CARTESIAN_POINT ( 'NONE',  ( -61.06482292022059255, 72.77422209630346117, -5.000000000000000000 ) ) ;
#30059 = DIRECTION ( 'NONE',  ( 0.000000000000000000, 0.000000000000000000, 1.000000000000000000 ) ) ;
#30060 = DIRECTION ( 'NONE',  ( 1.000000000000000000, 0.000000000000000000, 0.000000000000000000 ) ) ;
#30061 = DIRECTION ( 'NONE',  ( 1.000000000000000000, 0.000000000000000000, 0.000000000000000000 ) ) ;
#30062 = VERTEX_POINT ( 'NONE', #28557 ) ;
#30063 = DIRECTION ( 'NONE',  ( 1.000000000000000000, 0.000000000000000000, 0.000000000000000000 ) ) ;
#30064 = AXIS2_PLACEMENT_3D ( 'NONE', #7720, #27952, #19171 ) ;
#30065 = ORIENTED_EDGE ( 'NONE', *, *, #36910, .T. ) ;
#30066 = FACE_OUTER_BOUND ( 'NONE', #13530, .T. ) ;
#30067 = DIRECTION ( 'NONE',  ( 0.000000000000000000, -0.000000000000000000, -1.000000000000000000 ) ) ;
#30068 = CARTESIAN_POINT ( 'NONE',  ( 51.99999662536847467, 51.96152422706637708, 12.50000000000000000 ) ) ;
#30069 = CARTESIAN_POINT ( 'NONE',  ( 84.99999662536831124, -25.98076211353319565, -5.000000000000000000 ) ) ;
#30070 = EDGE_CURVE ( 'NONE', #3159, #3670, #20231, .T. ) ;
#30071 = CARTESIAN_POINT ( 'NONE',  ( -4.279621169095561228, 62.97617850287782915, 12.49999999999999822 ) ) ;
#30072 = EDGE_CURVE ( 'NONE', #34695, #12950, #2890, .T. ) ;
#30073 = DIRECTION ( 'NONE',  ( -1.000000000000000000, -0.000000000000000000, -0.000000000000000000 ) ) ;
#30074 = EDGE_CURVE ( 'NONE', #18017, #24720, #3452, .T. ) ;
#30075 = EDGE_CURVE ( 'NONE', #36125, #6234, #19935, .T. ) ;
#30076 = CARTESIAN_POINT ( 'NONE',  ( -77.00000337463097821, -8.660254037844422825, 12.50000000000000000 ) ) ;
#30077 = EDGE_LOOP ( 'NONE', ( #130, #30328 ) ) ;
#30078 = CARTESIAN_POINT ( 'NONE',  ( -87.00000337463093558, -25.98076211353322051, 12.50000000000000000 ) ) ;
#30079 = CARTESIAN_POINT ( 'NONE',  ( 61.99999662536842493, -51.96152422706639840, -5.000000000000000000 ) ) ;
#30080 = DIRECTION ( 'NONE',  ( 1.000000000000000000, 0.000000000000000000, 0.000000000000000000 ) ) ;
#30081 = ORIENTED_EDGE ( 'NONE', *, *, #1622, .T. ) ;
#30082 = CIRCLE ( 'NONE', #12695, 2.000000000000001776 ) ;
#30083 = CIRCLE ( 'NONE', #8547, 3.000000000000002665 ) ;
#30084 = EDGE_LOOP ( 'NONE', ( #21971, #23131 ) ) ;
#30085 = VERTEX_POINT ( 'NONE', #8872 ) ;
#30086 = DIRECTION ( 'NONE',  ( 0.000000000000000000, 0.000000000000000000, 1.000000000000000000 ) ) ;
#30087 = DIRECTION ( 'NONE',  ( -1.000000000000000000, 0.000000000000000000, 0.000000000000000000 ) ) ;
#30088 = DIRECTION ( 'NONE',  ( 1.000000000000000000, 0.000000000000000000, 0.000000000000000000 ) ) ;
#30089 = ORIENTED_EDGE ( 'NONE', *, *, #8302, .T. ) ;
#30090 = CARTESIAN_POINT ( 'NONE',  ( 41.99999662536853151, 69.28203230275518365, -9.999999999999998224 ) ) ;
#30091 = CIRCLE ( 'NONE', #13355, 2.000000000000001776 ) ;
#30092 = DIRECTION ( 'NONE',  ( 0.000000000000000000, 0.000000000000000000, 1.000000000000000000 ) ) ;
#30093 = EDGE_LOOP ( 'NONE', ( #15340, #4029, #25, #6035 ) ) ;
#30094 = CARTESIAN_POINT ( 'NONE',  ( 0.000000000000000000, 0.000000000000000000, 27.50000000000000000 ) ) ;
#30095 = ORIENTED_EDGE ( 'NONE', *, *, #31864, .F. ) ;
#30096 = DIRECTION ( 'NONE',  ( 0.000000000000000000, 0.000000000000000000, 1.000000000000000000 ) ) ;
#30097 = EDGE_CURVE ( 'NONE', #29465, #15238, #17322, .T. ) ;
#30098 = DIRECTION ( 'NONE',  ( 0.000000000000000000, 0.000000000000000000, 1.000000000000000000 ) ) ;
#30099 = DIRECTION ( 'NONE',  ( -1.000000000000000000, 0.000000000000000000, 0.000000000000000000 ) ) ;
#30100 = CARTESIAN_POINT ( 'NONE',  ( 23.49154088336464241, 103.5526315789473699, 32.50000000000000000 ) ) ;
#30101 = ORIENTED_EDGE ( 'NONE', *, *, #7868, .F. ) ;
#30102 = DIRECTION ( 'NONE',  ( -0.7071067811865514585, -0.7071067811865435759, 0.000000000000000000 ) ) ;
#30103 = CARTESIAN_POINT ( 'NONE',  ( 9.999996625368625658, 86.60254037844397601, -5.000000000000000000 ) ) ;
#30104 = DIRECTION ( 'NONE',  ( 0.000000000000000000, 0.000000000000000000, 1.000000000000000000 ) ) ;
#30105 = CIRCLE ( 'NONE', #36116, 33.00000000000001421 ) ;
#30106 = CARTESIAN_POINT ( 'NONE',  ( -85.00000337463092137, 8.660254037844389075, 12.50000000000000000 ) ) ;
#30107 = CYLINDRICAL_SURFACE ( 'NONE', #34128, 2.000000000000001776 ) ;
#30108 = VERTEX_POINT ( 'NONE', #8505 ) ;
#30109 = DIRECTION ( 'NONE',  ( 1.000000000000000000, 0.000000000000000000, 0.000000000000000000 ) ) ;
#30110 = CARTESIAN_POINT ( 'NONE',  ( -53.00000337463109190, -60.62177826491083010, -9.999999999999998224 ) ) ;
#30111 = DIRECTION ( 'NONE',  ( 1.000000000000000000, 0.000000000000000000, 0.000000000000000000 ) ) ;
#30112 = VERTEX_POINT ( 'NONE', #20310 ) ;
#30113 = AXIS2_PLACEMENT_3D ( 'NONE', #36721, #20514, #26352 ) ;
#30114 = EDGE_CURVE ( 'NONE', #11413, #2754, #29803, .T. ) ;
#30115 = ORIENTED_EDGE ( 'NONE', *, *, #32475, .F. ) ;
#30116 = CYLINDRICAL_SURFACE ( 'NONE', #19573, 33.00000000000001421 ) ;
#30117 = DIRECTION ( 'NONE',  ( 0.000000000000000000, 0.000000000000000000, 1.000000000000000000 ) ) ;
#30118 = CARTESIAN_POINT ( 'NONE',  ( 54.99999662536844625, 43.30127018922198801, -9.999999999999998224 ) ) ;
#30119 = ORIENTED_EDGE ( 'NONE', *, *, #11581, .T. ) ;
#30120 = CARTESIAN_POINT ( 'NONE',  ( -52.39915983220772233, -35.19434990244957362, -4.999999999999997335 ) ) ;
#30121 = CARTESIAN_POINT ( 'NONE',  ( -83.00000337463092137, -8.660254037844422825, -9.999999999999998224 ) ) ;
#30122 = CARTESIAN_POINT ( 'NONE',  ( -15.00000337463125710, -77.94228634059960825, 17.49999999999999645 ) ) ;
#30123 = AXIS2_PLACEMENT_3D ( 'NONE', #28757, #25779, #3081 ) ;
#30124 = CARTESIAN_POINT ( 'NONE',  ( 62.97617850287784336, 4.279621169095339184, -4.999999999999997335 ) ) ;
#30125 = ORIENTED_EDGE ( 'NONE', *, *, #2930, .T. ) ;
#30126 = VERTEX_POINT ( 'NONE', #16941 ) ;
#30127 = CIRCLE ( 'NONE', #21164, 3.499999999999989342 ) ;
#30128 = DIRECTION ( 'NONE',  ( 0.000000000000000000, 0.000000000000000000, -1.000000000000000000 ) ) ;
#30129 = CARTESIAN_POINT ( 'NONE',  ( 0.000000000000000000, 0.000000000000000000, 2.266666666666999674 ) ) ;
#30130 = VERTEX_POINT ( 'NONE', #13935 ) ;
#30131 = FACE_BOUND ( 'NONE', #35724, .T. ) ;
#30132 = ORIENTED_EDGE ( 'NONE', *, *, #26163, .T. ) ;
#30133 = CARTESIAN_POINT ( 'NONE',  ( 14.99999662536863632, -77.94228634059960825, -9.999999999999998224 ) ) ;
#30134 = ADVANCED_FACE ( 'NONE', ( #22936 ), #25384, .F. ) ;
#30135 = AXIS2_PLACEMENT_3D ( 'NONE', #14702, #19609, #31221 ) ;
#30136 = CARTESIAN_POINT ( 'NONE',  ( 0.000000000000000000, 0.000000000000000000, 15.00000000000000000 ) ) ;
#30137 = ORIENTED_EDGE ( 'NONE', *, *, #2824, .F. ) ;
#30138 = VECTOR ( 'NONE', #13374, 999.9999999999998863 ) ;
#30139 = VERTEX_POINT ( 'NONE', #14495 ) ;
#30140 = DIRECTION ( 'NONE',  ( 0.000000000000000000, 0.000000000000000000, 1.000000000000000000 ) ) ;
#30141 = VERTEX_POINT ( 'NONE', #28364 ) ;
#30142 = CARTESIAN_POINT ( 'NONE',  ( 0.000000000000000000, 0.000000000000000000, 0.000000000000000000 ) ) ;
#30143 = AXIS2_PLACEMENT_3D ( 'NONE', #8551, #3489, #31406 ) ;
#30144 = PRODUCT_DEFINITION_SHAPE ( 'NONE', 'NONE',  #37109 ) ;
#30145 = DIRECTION ( 'NONE',  ( 0.000000000000000000, 0.000000000000000000, 1.000000000000000000 ) ) ;
#30146 = EDGE_CURVE ( 'NONE', #28337, #16532, #4666, .T. ) ;
#30147 = DIRECTION ( 'NONE',  ( 0.000000000000000000, 0.000000000000000000, 1.000000000000000000 ) ) ;
#30148 = DIRECTION ( 'NONE',  ( 1.000000000000000000, 0.000000000000000000, 0.000000000000000000 ) ) ;
#30149 = VERTEX_POINT ( 'NONE', #23116 ) ;
#30150 = CARTESIAN_POINT ( 'NONE',  ( 69.99999662536839651, 34.64101615137758472, -5.000000000000000000 ) ) ;
#30151 = DIRECTION ( 'NONE',  ( 1.000000000000000000, 0.000000000000000000, 0.000000000000000000 ) ) ;
#30152 = ORIENTED_EDGE ( 'NONE', *, *, #33143, .T. ) ;
#30153 = VERTEX_POINT ( 'NONE', #34570 ) ;
#30154 = AXIS2_PLACEMENT_3D ( 'NONE', #35968, #33122, #7442 ) ;
#30155 = ORIENTED_EDGE ( 'NONE', *, *, #1277, .T. ) ;
#30156 = DIRECTION ( 'NONE',  ( 0.000000000000000000, 0.000000000000000000, 1.000000000000000000 ) ) ;
#30157 = EDGE_CURVE ( 'NONE', #15837, #2273, #7066, .T. ) ;
#30158 = FACE_OUTER_BOUND ( 'NONE', #32187, .T. ) ;
#30159 = ORIENTED_EDGE ( 'NONE', *, *, #16844, .F. ) ;
#30160 = DIRECTION ( 'NONE',  ( -1.000000000000000000, 0.000000000000000000, 0.000000000000000000 ) ) ;
#30161 = CYLINDRICAL_SURFACE ( 'NONE', #20175, 2.000000000000001776 ) ;
#30162 = ORIENTED_EDGE ( 'NONE', *, *, #18929, .F. ) ;
#30163 = CARTESIAN_POINT ( 'NONE',  ( 54.99999662536844625, -60.62177826491080168, 17.49999999999999645 ) ) ;
#30164 = AXIS2_PLACEMENT_3D ( 'NONE', #206, #4620, #4810 ) ;
#30165 = CARTESIAN_POINT ( 'NONE',  ( -50.00000337463109190, 69.28203230275518365, 17.49999999999999645 ) ) ;
#30166 = CARTESIAN_POINT ( 'NONE',  ( -52.39915983220772233, -35.19434990244957362, -4.999999999999997335 ) ) ;
#30167 = CARTESIAN_POINT ( 'NONE',  ( 102.9785387920993003, -33.47425447865018810, 32.49999999999999289 ) ) ;
#30168 = CARTESIAN_POINT ( 'NONE',  ( 6.999996625368676284, -77.94228634059960825, -9.999999999999998224 ) ) ;
#30169 = CARTESIAN_POINT ( 'NONE',  ( -35.00000337463117717, -77.94228634059963667, 17.49999999999999645 ) ) ;
#30170 = EDGE_LOOP ( 'NONE', ( #1874, #17643, #17702 ) ) ;
#30171 = EDGE_LOOP ( 'NONE', ( #15173, #25583, #15013, #31227 ) ) ;
#30172 = CARTESIAN_POINT ( 'NONE',  ( 59.99999662536842493, 51.96152422706639129, -5.000000000000000000 ) ) ;
#30173 = ADVANCED_FACE ( 'NONE', ( #22568 ), #25573, .T. ) ;
#30174 = DIRECTION ( 'NONE',  ( 0.000000000000000000, 0.000000000000000000, 1.000000000000000000 ) ) ;
#30175 = DIRECTION ( 'NONE',  ( 0.000000000000000000, 0.000000000000000000, 1.000000000000000000 ) ) ;
#30176 = DIRECTION ( 'NONE',  ( 0.000000000000000000, 0.000000000000000000, 1.000000000000000000 ) ) ;
#30177 = ORIENTED_EDGE ( 'NONE', *, *, #23387, .F. ) ;
#30178 = UNCERTAINTY_MEASURE_WITH_UNIT (LENGTH_MEASURE( 1.000000000000000082E-05 ), #18348, 'distance_accuracy_value', 'NONE');
#30179 = DIRECTION ( 'NONE',  ( 0.000000000000000000, 0.000000000000000000, -1.000000000000000000 ) ) ;
#30180 = LINE ( 'NONE', #21584, #5754 ) ;
#30181 = AXIS2_PLACEMENT_3D ( 'NONE', #21478, #15840, #2090 ) ;
#30182 = CARTESIAN_POINT ( 'NONE',  ( -62.97617850287781494, -4.279621169095772615, -49.86561046011506448 ) ) ;
#30183 = VERTEX_POINT ( 'NONE', #11322 ) ;
#30184 = EDGE_CURVE ( 'NONE', #7360, #25770, #13645, .T. ) ;
#30185 = DIRECTION ( 'NONE',  ( 1.000000000000000000, 0.000000000000000000, 0.000000000000000000 ) ) ;
#30186 = ORIENTED_EDGE ( 'NONE', *, *, #6698, .T. ) ;
#30187 = CARTESIAN_POINT ( 'NONE',  ( 84.99999662536832545, 25.98076211353319565, -9.999999999999998224 ) ) ;
#30188 = VECTOR ( 'NONE', #12577, 1000.000000000000000 ) ;
#30189 = LINE ( 'NONE', #30582, #15825 ) ;
#30190 = ADVANCED_FACE ( 'NONE', ( #979 ), #35495, .F. ) ;
#30191 = VECTOR ( 'NONE', #7310, 1000.000000000000000 ) ;
#30192 = DIRECTION ( 'NONE',  ( -0.8660254037844449249, -0.4999999999999888978, 0.000000000000000000 ) ) ;
#30193 = ORIENTED_EDGE ( 'NONE', *, *, #4288, .T. ) ;
#30194 = ORIENTED_EDGE ( 'NONE', *, *, #9959, .T. ) ;
#30195 = EDGE_LOOP ( 'NONE', ( #1302, #36120 ) ) ;
#30196 = CYLINDRICAL_SURFACE ( 'NONE', #29156, 5.750000000000002665 ) ;
#30197 = DIRECTION ( 'NONE',  ( 0.000000000000000000, 0.000000000000000000, 1.000000000000000000 ) ) ;
#30198 = AXIS2_PLACEMENT_3D ( 'NONE', #26800, #23809, #24167 ) ;
#30199 = FACE_OUTER_BOUND ( 'NONE', #7413, .T. ) ;
#30200 = CARTESIAN_POINT ( 'NONE',  ( 0.000000000000000000, 0.000000000000000000, -5.000000000000000000 ) ) ;
#30201 = FACE_OUTER_BOUND ( 'NONE', #12144, .T. ) ;
#30202 = EDGE_LOOP ( 'NONE', ( #14608, #30379, #19583, #13723 ) ) ;
#30203 = DIRECTION ( 'NONE',  ( 0.000000000000000000, 0.000000000000000000, 1.000000000000000000 ) ) ;
#30204 = AXIS2_PLACEMENT_3D ( 'NONE', #22898, #2478, #19536 ) ;
#30205 = EDGE_CURVE ( 'NONE', #29817, #8784, #8847, .T. ) ;
#30206 = DIRECTION ( 'NONE',  ( 1.000000000000000000, 0.000000000000000000, 0.000000000000000000 ) ) ;
#30207 = CYLINDRICAL_SURFACE ( 'NONE', #32573, 2.000000000000001776 ) ;
#30208 = ORIENTED_EDGE ( 'NONE', *, *, #10977, .T. ) ;
#30209 = DIRECTION ( 'NONE',  ( 1.000000000000000000, 0.000000000000000000, 0.000000000000000000 ) ) ;
#30210 = CARTESIAN_POINT ( 'NONE',  ( -42.97377950131527058, 96.90768712682508124, 27.49999999999999645 ) ) ;
#30211 = ORIENTED_EDGE ( 'NONE', *, *, #19302, .T. ) ;
#30212 = EDGE_CURVE ( 'NONE', #30829, #1410, #5281, .T. ) ;
#30213 = ORIENTED_EDGE ( 'NONE', *, *, #1024, .T. ) ;
#30214 = AXIS2_PLACEMENT_3D ( 'NONE', #28106, #31103, #5429 ) ;
#30215 = ADVANCED_FACE ( 'NONE', ( #20858 ), #12401, .F. ) ;
#30216 = CARTESIAN_POINT ( 'NONE',  ( -55.00000337463107059, 43.30127018922197379, -9.999999999999998224 ) ) ;
#30217 = CARTESIAN_POINT ( 'NONE',  ( 0.7030283904595543421, -5.367609061415079097, -4.096693167836665594 ) ) ;
#30218 = CARTESIAN_POINT ( 'NONE',  ( -4.084562121000262280, -3.415279651815011253, -1.156968425231159614 ) ) ;
#30219 = VERTEX_POINT ( 'NONE', #9222 ) ;
#30220 = ORIENTED_EDGE ( 'NONE', *, *, #12616, .T. ) ;
#30221 = VERTEX_POINT ( 'NONE', #9427 ) ;
#30222 = DIRECTION ( 'NONE',  ( 1.000000000000000000, 0.000000000000000000, 0.000000000000000000 ) ) ;
#30223 = AXIS2_PLACEMENT_3D ( 'NONE', #35625, #12916, #6930 ) ;
#30224 = ORIENTED_EDGE ( 'NONE', *, *, #2468, .T. ) ;
#30225 = CIRCLE ( 'NONE', #14059, 6.000000000000005329 ) ;
#30226 = ORIENTED_EDGE ( 'NONE', *, *, #17225, .T. ) ;
#30227 = PLANE ( 'NONE',  #11192 ) ;
#30228 = VERTEX_POINT ( 'NONE', #20655 ) ;
#30229 = VERTEX_POINT ( 'NONE', #23314 ) ;
#30230 = AXIS2_PLACEMENT_3D ( 'NONE', #16864, #2800, #5600 ) ;
#30231 = DIRECTION ( 'NONE',  ( 0.000000000000000000, 0.000000000000000000, 1.000000000000000000 ) ) ;
#30232 = ADVANCED_FACE ( 'NONE', ( #29466 ), #23488, .F. ) ;
#30233 = DIRECTION ( 'NONE',  ( 0.000000000000000000, 0.000000000000000000, -1.000000000000000000 ) ) ;
#30234 = EDGE_LOOP ( 'NONE', ( #7895, #2342 ) ) ;
#30235 = EDGE_LOOP ( 'NONE', ( #10539, #24244, #14477, #2628 ) ) ;
#30236 = DIRECTION ( 'NONE',  ( 1.000000000000000000, 0.000000000000000000, 0.000000000000000000 ) ) ;
#30237 = DIRECTION ( 'NONE',  ( -1.000000000000000000, 0.000000000000000000, 0.000000000000000000 ) ) ;
#30238 = VECTOR ( 'NONE', #27104, 1000.000000000000000 ) ;
#30239 = DIRECTION ( 'NONE',  ( -0.000000000000000000, -0.000000000000000000, -1.000000000000000000 ) ) ;
#30240 = CIRCLE ( 'NONE', #14662, 2.000000000000001776 ) ;
#30241 = FACE_OUTER_BOUND ( 'NONE', #26883, .T. ) ;
#30242 = ORIENTED_EDGE ( 'NONE', *, *, #24751, .F. ) ;
#30243 = CARTESIAN_POINT ( 'NONE',  ( -74.30619744049063513, -84.18124734178186941, 32.50000000000000000 ) ) ;
#30244 = VERTEX_POINT ( 'NONE', #6617 ) ;
#30245 = DIRECTION ( 'NONE',  ( 0.000000000000000000, 0.000000000000000000, 1.000000000000000000 ) ) ;
#30246 = FACE_OUTER_BOUND ( 'NONE', #23141, .T. ) ;
#30247 = DIRECTION ( 'NONE',  ( 0.000000000000000000, 0.000000000000000000, -1.000000000000000000 ) ) ;
#30248 = DIRECTION ( 'NONE',  ( 0.5000000000000039968, 0.8660254037844363761, 0.000000000000000000 ) ) ;
#30249 = DIRECTION ( 'NONE',  ( 0.000000000000000000, 0.000000000000000000, 1.000000000000000000 ) ) ;
#30250 = EDGE_CURVE ( 'NONE', #1539, #36932, #9617, .T. ) ;
#30251 = DIRECTION ( 'NONE',  ( -0.000000000000000000, -0.000000000000000000, 1.000000000000000000 ) ) ;
#30252 = CIRCLE ( 'NONE', #23673, 2.000000000000001776 ) ;
#30253 = CARTESIAN_POINT ( 'NONE',  ( -27.78182860042817026, -56.67878100130359087, 12.49999999999999822 ) ) ;
#30254 = VERTEX_POINT ( 'NONE', #26862 ) ;
#30255 = EDGE_CURVE ( 'NONE', #13946, #19982, #22615, .T. ) ;
#30257 = CIRCLE ( 'NONE', #9917, 95.00000000000001421 ) ;
#30256 = DIRECTION ( 'NONE',  ( 0.000000000000000000, -1.000000000000000000, 0.000000000000000000 ) ) ;
#30258 = CARTESIAN_POINT ( 'NONE',  ( 74.99999662536836809, 8.660254037844394404, -5.000000000000000000 ) ) ;
#30259 = CARTESIAN_POINT ( 'NONE',  ( 56.99999662536844625, 43.30127018922198801, 12.50000000000000000 ) ) ;
#30260 = AXIS2_PLACEMENT_3D ( 'NONE', #27047, #1545, #9988 ) ;
#30261 = AXIS2_PLACEMENT_3D ( 'NONE', #34085, #19638, #22263 ) ;
#30262 = ORIENTED_EDGE ( 'NONE', *, *, #22448, .F. ) ;
#30263 = EDGE_CURVE ( 'NONE', #20675, #6890, #17240, .T. ) ;
#30264 = CIRCLE ( 'NONE', #17098, 3.500000000000003109 ) ;
#30265 = VERTEX_POINT ( 'NONE', #32469 ) ;
#30266 = EDGE_LOOP ( 'NONE', ( #8367, #34964, #21524, #8973 ) ) ;
#30267 = DIRECTION ( 'NONE',  ( 0.000000000000000000, 0.000000000000000000, 1.000000000000000000 ) ) ;
#30268 = FACE_OUTER_BOUND ( 'NONE', #25942, .T. ) ;
#30269 = EDGE_CURVE ( 'NONE', #26676, #15417, #18445, .T. ) ;
#30270 = EDGE_LOOP ( 'NONE', ( #2065, #10616, #34109, #35024 ) ) ;
#30271 = EDGE_CURVE ( 'NONE', #7029, #3626, #22032, .T. ) ;
#30272 = CIRCLE ( 'NONE', #23692, 30.00000000000000000 ) ;
#30273 = VECTOR ( 'NONE', #24698, 1000.000000000000000 ) ;
#30274 = DIRECTION ( 'NONE',  ( 0.000000000000000000, 0.000000000000000000, 1.000000000000000000 ) ) ;
#30275 = CARTESIAN_POINT ( 'NONE',  ( -20.00000337463124112, 69.28203230275516944, -9.999999999999998224 ) ) ;
#30276 = ORIENTED_EDGE ( 'NONE', *, *, #10882, .T. ) ;
#30277 = DIRECTION ( 'NONE',  ( 0.000000000000000000, 0.000000000000000000, -1.000000000000000000 ) ) ;
#30278 = ORIENTED_EDGE ( 'NONE', *, *, #36622, .F. ) ;
#30279 = FACE_BOUND ( 'NONE', #8653, .T. ) ;
#30280 = ADVANCED_FACE ( 'NONE', ( #6229 ), #12596, .F. ) ;
#30281 = EDGE_CURVE ( 'NONE', #695, #11751, #3620, .T. ) ;
#30282 = DIRECTION ( 'NONE',  ( 0.000000000000000000, 0.000000000000000000, 1.000000000000000000 ) ) ;
#30283 = DIRECTION ( 'NONE',  ( 1.000000000000000000, 0.000000000000000000, 0.000000000000000000 ) ) ;
#30284 = EDGE_CURVE ( 'NONE', #16882, #37014, #26664, .T. ) ;
#30285 = CIRCLE ( 'NONE', #29682, 1.999999999999998224 ) ;
#30286 = EDGE_CURVE ( 'NONE', #4050, #28376, #32175, .T. ) ;
#30287 = DIRECTION ( 'NONE',  ( 1.000000000000000000, 0.000000000000000000, 0.000000000000000000 ) ) ;
#30288 = AXIS2_PLACEMENT_3D ( 'NONE', #1521, #26857, #1172 ) ;
#30289 = ORIENTED_EDGE ( 'NONE', *, *, #27213, .F. ) ;
#30290 = CARTESIAN_POINT ( 'NONE',  ( 54.99999662536844625, 60.62177826491077326, 12.50000000000000000 ) ) ;
#30291 = AXIS2_PLACEMENT_3D ( 'NONE', #14410, #25849, #17410 ) ;
#30292 = CIRCLE ( 'NONE', #25504, 2.000000000000001776 ) ;
#30293 = PRODUCT_CONTEXT ( 'NONE', #1266, 'mechanical' ) ;
#30294 = AXIS2_PLACEMENT_3D ( 'NONE', #4964, #20083, #33660 ) ;
#30295 = AXIS2_PLACEMENT_3D ( 'NONE', #22772, #25574, #13937 ) ;
#30296 = CARTESIAN_POINT ( 'NONE',  ( -72.00000337463100664, -2.404119930384582903E-14, 12.50000000000000000 ) ) ;
#30297 = DIRECTION ( 'NONE',  ( -0.000000000000000000, -0.000000000000000000, -1.000000000000000000 ) ) ;
#30298 = VECTOR ( 'NONE', #10467, 999.9999999999998863 ) ;
#30299 = CARTESIAN_POINT ( 'NONE',  ( 4.279621169095998212, -62.97617850287780072, 12.49999999999999822 ) ) ;
#30300 = CARTESIAN_POINT ( 'NONE',  ( 49.99999662536846756, 51.96152422706637708, -5.000000000000000000 ) ) ;
#30301 = ORIENTED_EDGE ( 'NONE', *, *, #24954, .T. ) ;
#30302 = CARTESIAN_POINT ( 'NONE',  ( -5.000003374631307729, 77.94228634059957983, 17.49999999999999645 ) ) ;
#30303 = AXIS2_PLACEMENT_3D ( 'NONE', #30310, #24697, #33519 ) ;
#30304 = DIRECTION ( 'NONE',  ( 1.000000000000000000, 0.000000000000000000, 0.000000000000000000 ) ) ;
#30305 = DIRECTION ( 'NONE',  ( 0.000000000000000000, 0.000000000000000000, 1.000000000000000000 ) ) ;
#30306 = AXIS2_PLACEMENT_3D ( 'NONE', #8473, #34344, #29060 ) ;
#30307 = EDGE_LOOP ( 'NONE', ( #10236, #34805 ) ) ;
#30308 = ORIENTED_EDGE ( 'NONE', *, *, #19084, .F. ) ;
#30309 = CARTESIAN_POINT ( 'NONE',  ( 82.99999662536831124, -8.660254037844397956, -9.999999999999998224 ) ) ;
#30310 = CARTESIAN_POINT ( 'NONE',  ( 69.99999662536838230, -34.64101615137759183, -5.000000000000000000 ) ) ;
#30311 = DIRECTION ( 'NONE',  ( 1.000000000000000000, 0.000000000000000000, 0.000000000000000000 ) ) ;
#30312 = ORIENTED_EDGE ( 'NONE', *, *, #20658, .F. ) ;
#30313 = AXIS2_PLACEMENT_3D ( 'NONE', #920, #26431, #17998 ) ;
#30314 = DIRECTION ( 'NONE',  ( 0.000000000000000000, 0.000000000000000000, 1.000000000000000000 ) ) ;
#30315 = CARTESIAN_POINT ( 'NONE',  ( 64.99999662536839651, -60.62177826491080168, -5.000000000000000000 ) ) ;
#30316 = CARTESIAN_POINT ( 'NONE',  ( 0.000000000000000000, 0.000000000000000000, 0.000000000000000000 ) ) ;
#30317 = VECTOR ( 'NONE', #2900, 1000.000000000000000 ) ;
#30318 = AXIS2_PLACEMENT_3D ( 'NONE', #29678, #27441, #32684 ) ;
#30319 = DIRECTION ( 'NONE',  ( 0.000000000000000000, 0.000000000000000000, -1.000000000000000000 ) ) ;
#30320 = CIRCLE ( 'NONE', #31511, 1.999999999999998224 ) ;
#30321 = ORIENTED_EDGE ( 'NONE', *, *, #27526, .F. ) ;
#30322 = ORIENTED_EDGE ( 'NONE', *, *, #16762, .F. ) ;
#30323 = CARTESIAN_POINT ( 'NONE',  ( 0.000000000000000000, 0.000000000000000000, -5.000000000000000000 ) ) ;
#30324 = AXIS2_PLACEMENT_3D ( 'NONE', #19424, #36312, #10424 ) ;
#30325 = DIRECTION ( 'NONE',  ( 1.000000000000000000, 0.000000000000000000, 0.000000000000000000 ) ) ;
#30326 = ORIENTED_EDGE ( 'NONE', *, *, #33639, .T. ) ;
#30327 = DIRECTION ( 'NONE',  ( -1.000000000000000000, 0.000000000000000000, -0.000000000000000000 ) ) ;
#30328 = ORIENTED_EDGE ( 'NONE', *, *, #3208, .T. ) ;
#30329 = DIRECTION ( 'NONE',  ( -0.000000000000000000, -0.000000000000000000, -1.000000000000000000 ) ) ;
#30330 = CARTESIAN_POINT ( 'NONE',  ( 14.99999662536859901, 77.94228634059957983, 12.50000000000000000 ) ) ;
#30331 = ORIENTED_EDGE ( 'NONE', *, *, #29026, .T. ) ;
#30332 = EDGE_CURVE ( 'NONE', #2053, #34151, #13026, .T. ) ;
#30333 = CYLINDRICAL_SURFACE ( 'NONE', #12261, 2.000000000000001776 ) ;
#30334 = ORIENTED_EDGE ( 'NONE', *, *, #165, .F. ) ;
#30335 = FILL_AREA_STYLE_COLOUR ( '', #35152 ) ;
#30336 = CIRCLE ( 'NONE', #36929, 27.00000000000001421 ) ;
#30337 = CARTESIAN_POINT ( 'NONE',  ( 14.99999662536859901, 77.94228634059957983, 17.49999999999999645 ) ) ;
#30338 = CIRCLE ( 'NONE', #14174, 2.000000000000000000 ) ;
#30339 = DIRECTION ( 'NONE',  ( 0.000000000000000000, 0.000000000000000000, 1.000000000000000000 ) ) ;
#30340 = DIRECTION ( 'NONE',  ( -1.000000000000000000, 0.000000000000000000, 0.000000000000000000 ) ) ;
#30341 = ORIENTED_EDGE ( 'NONE', *, *, #26492, .T. ) ;
#30342 = CARTESIAN_POINT ( 'NONE',  ( 40.99999999999999289, 103.4105893997321743, 32.50000000000000000 ) ) ;
#30343 = CARTESIAN_POINT ( 'NONE',  ( 31.46585318596250502, 86.45172111230321832, -49.86348611802629449 ) ) ;
#30344 = CARTESIAN_POINT ( 'NONE',  ( -2.712167343862821323, -4.207632145829752979, -6.000000000000000888 ) ) ;
#30345 = EDGE_LOOP ( 'NONE', ( #9276, #6336, #18054, #34001 ) ) ;
#30346 = ORIENTED_EDGE ( 'NONE', *, *, #9835, .T. ) ;
#30347 = CONICAL_SURFACE ( 'NONE', #22564, 3.000000000000000000, 0.9599310885968762586 ) ;
#30348 = VERTEX_POINT ( 'NONE', #3433 ) ;
#30349 = DIRECTION ( 'NONE',  ( -1.000000000000000000, 0.000000000000000000, 0.000000000000000000 ) ) ;
#30350 = VERTEX_POINT ( 'NONE', #14868 ) ;
#30351 = DIRECTION ( 'NONE',  ( -1.000000000000000000, 0.000000000000000000, 0.000000000000000000 ) ) ;
#30352 = DIRECTION ( 'NONE',  ( -1.000000000000000000, 0.000000000000000000, 0.000000000000000000 ) ) ;
#30353 = EDGE_CURVE ( 'NONE', #28869, #2447, #26307, .T. ) ;
#30354 = EDGE_CURVE ( 'NONE', #35698, #30350, #33036, .T. ) ;
#30355 = AXIS2_PLACEMENT_3D ( 'NONE', #952, #12371, #1502 ) ;
#30356 = CARTESIAN_POINT ( 'NONE',  ( 21.99999662536862033, -69.28203230275519786, -9.999999999999998224 ) ) ;
#30357 = CARTESIAN_POINT ( 'NONE',  ( -75.00000337463097821, -8.660254037844422825, -9.999999999999998224 ) ) ;
#30358 = DIRECTION ( 'NONE',  ( 0.000000000000000000, 0.000000000000000000, 1.000000000000000000 ) ) ;
#30359 = DIRECTION ( 'NONE',  ( 1.000000000000000000, 0.000000000000000000, 0.000000000000000000 ) ) ;
#30360 = CIRCLE ( 'NONE', #31644, 2.000000000000001776 ) ;
#30361 = AXIS2_PLACEMENT_3D ( 'NONE', #30122, #10086, #4275 ) ;
#30362 = CARTESIAN_POINT ( 'NONE',  ( 76.99999662536836809, 25.98076211353319565, -9.999999999999998224 ) ) ;
#30363 = VERTEX_POINT ( 'NONE', #32860 ) ;
#30364 = CIRCLE ( 'NONE', #14198, 2.000000000000001776 ) ;
#30365 = ORIENTED_EDGE ( 'NONE', *, *, #1170, .T. ) ;
#30366 = EDGE_CURVE ( 'NONE', #22384, #2691, #12422, .T. ) ;
#30367 = DIRECTION ( 'NONE',  ( 0.000000000000000000, 0.000000000000000000, 1.000000000000000000 ) ) ;
#30368 = VECTOR ( 'NONE', #34026, 1000.000000000000000 ) ;
#30369 = CARTESIAN_POINT ( 'NONE',  ( 56.56138580058825482, 61.87160379013676703, 12.50000000000000000 ) ) ;
#30370 = CARTESIAN_POINT ( 'NONE',  ( -77.00000337463097821, 25.98076211353318854, -9.999999999999998224 ) ) ;
#30371 = DIRECTION ( 'NONE',  ( 1.000000000000000000, 0.000000000000000000, 0.000000000000000000 ) ) ;
#30372 = VERTEX_POINT ( 'NONE', #29126 ) ;
#30373 = ORIENTED_EDGE ( 'NONE', *, *, #36938, .F. ) ;
#30375 = AXIS2_PLACEMENT_3D ( 'NONE', #31273, #20025, #140 ) ;
#30374 = CYLINDRICAL_SURFACE ( 'NONE', #15326, 3.000000000000002665 ) ;
#30376 = DIRECTION ( 'NONE',  ( 0.4415113423096792000, 5.406954521468000113E-17, -0.8972556684757725387 ) ) ;
#30377 = AXIS2_PLACEMENT_3D ( 'NONE', #3660, #1023, #15266 ) ;
#30378 = CARTESIAN_POINT ( 'NONE',  ( 64.99999662536839651, 60.62177826491078747, -9.999999999999998224 ) ) ;
#30379 = ORIENTED_EDGE ( 'NONE', *, *, #4941, .T. ) ;
#30380 = EDGE_CURVE ( 'NONE', #36171, #27334, #471, .T. ) ;
#30381 = DIRECTION ( 'NONE',  ( 0.000000000000000000, -1.000000000000000000, 1.625241993126352989E-15 ) ) ;
#30382 = ORIENTED_EDGE ( 'NONE', *, *, #21456, .F. ) ;
#30383 = VECTOR ( 'NONE', #32379, 1000.000000000000000 ) ;
#30384 = DIRECTION ( 'NONE',  ( 0.000000000000000000, 0.000000000000000000, 1.000000000000000000 ) ) ;
#30385 = FACE_OUTER_BOUND ( 'NONE', #18633, .T. ) ;
#30386 = DIRECTION ( 'NONE',  ( 0.000000000000000000, -0.000000000000000000, -1.000000000000000000 ) ) ;
#30387 = CIRCLE ( 'NONE', #15430, 30.00000000000000000 ) ;
#30388 = DIRECTION ( 'NONE',  ( 1.000000000000000000, 0.000000000000000000, 0.000000000000000000 ) ) ;
#30389 = ORIENTED_EDGE ( 'NONE', *, *, #30542, .T. ) ;
#30390 = VERTEX_POINT ( 'NONE', #1348 ) ;
#30391 = VECTOR ( 'NONE', #36870, 999.9999999999998863 ) ;
#30392 = AXIS2_PLACEMENT_3D ( 'NONE', #4393, #13008, #22369 ) ;
#30393 = CIRCLE ( 'NONE', #34585, 2.000000000000001776 ) ;
#30394 = DIRECTION ( 'NONE',  ( 0.000000000000000000, 0.000000000000000000, 1.000000000000000000 ) ) ;
#30395 = EDGE_LOOP ( 'NONE', ( #23892, #4441, #33429, #34025 ) ) ;
#30396 = DIRECTION ( 'NONE',  ( -1.224646799147353207E-16, 1.000000000000000000, 0.000000000000000000 ) ) ;
#30397 = EDGE_CURVE ( 'NONE', #21619, #19686, #27399, .T. ) ;
#30398 = FACE_OUTER_BOUND ( 'NONE', #5909, .T. ) ;
#30399 = CARTESIAN_POINT ( 'NONE',  ( 0.8333333333333367010, -5.292377467571611760, -3.818275046351177870 ) ) ;
#30400 = LINE ( 'NONE', #27594, #27092 ) ;
#30401 = CARTESIAN_POINT ( 'NONE',  ( -26.97173872511423198, 77.60723454213314199, -5.000000000000000000 ) ) ;
#30402 = EDGE_CURVE ( 'NONE', #33336, #15570, #34003, .T. ) ;
#30403 = EDGE_LOOP ( 'NONE', ( #16809, #17921, #23580, #17770 ) ) ;
#30404 = DIRECTION ( 'NONE',  ( 1.000000000000000000, 0.000000000000000000, 0.000000000000000000 ) ) ;
#30405 = CIRCLE ( 'NONE', #34594, 2.000000000000001776 ) ;
#30406 = CIRCLE ( 'NONE', #16045, 2.000000000000001776 ) ;
#30407 = LINE ( 'NONE', #15976, #1802 ) ;
#30408 = CYLINDRICAL_SURFACE ( 'NONE', #15204, 3.499999999999996003 ) ;
#30409 = ORIENTED_EDGE ( 'NONE', *, *, #30046, .F. ) ;
#30410 = DIRECTION ( 'NONE',  ( 0.000000000000000000, 0.000000000000000000, 1.000000000000000000 ) ) ;
#30411 = ADVANCED_FACE ( 'NONE', ( #7730 ), #1732, .F. ) ;
#30412 = FACE_BOUND ( 'NONE', #25320, .T. ) ;
#30413 = AXIS2_PLACEMENT_3D ( 'NONE', #12445, #21457, #12634 ) ;
#30414 = EDGE_LOOP ( 'NONE', ( #5280, #17369, #551, #6147 ) ) ;
#30415 = EDGE_LOOP ( 'NONE', ( #23078, #23418 ) ) ;
#30416 = ADVANCED_FACE ( 'NONE', ( #36420 ), #16177, .F. ) ;
#30417 = AXIS2_PLACEMENT_3D ( 'NONE', #17640, #3411, #14847 ) ;
#30418 = DIRECTION ( 'NONE',  ( -1.000000000000000000, 0.000000000000000000, 0.000000000000000000 ) ) ;
#30419 = CARTESIAN_POINT ( 'NONE',  ( -25.00000000000000000, 0.000000000000000000, 15.00000000000000000 ) ) ;
#30420 = DIRECTION ( 'NONE',  ( 0.000000000000000000, -0.8660254037844388186, -0.4999999999999997224 ) ) ;
#30421 = EDGE_LOOP ( 'NONE', ( #27192, #34224 ) ) ;
#30422 = ORIENTED_EDGE ( 'NONE', *, *, #29747, .F. ) ;
#30423 = AXIS2_PLACEMENT_3D ( 'NONE', #32523, #23934, #26533 ) ;
#30424 = CIRCLE ( 'NONE', #29795, 2.000000000000001776 ) ;
#30425 = ORIENTED_EDGE ( 'NONE', *, *, #27435, .T. ) ;
#30426 = AXIS2_PLACEMENT_3D ( 'NONE', #514, #29189, #3523 ) ;
#30427 = FACE_BOUND ( 'NONE', #18420, .T. ) ;
#30428 = CIRCLE ( 'NONE', #8880, 45.00000000000000000 ) ;
#30429 = ORIENTED_EDGE ( 'NONE', *, *, #20174, .F. ) ;
#30430 = CARTESIAN_POINT ( 'NONE',  ( -4.242640687119211051, 4.242640687119288323, 32.50000000000000000 ) ) ;
#30431 = VERTEX_POINT ( 'NONE', #7533 ) ;
#30432 = EDGE_LOOP ( 'NONE', ( #7355, #4008 ) ) ;
#30433 = CIRCLE ( 'NONE', #14272, 2.000000000000001776 ) ;
#30434 = EDGE_CURVE ( 'NONE', #20671, #26912, #35208, .T. ) ;
#30435 = CARTESIAN_POINT ( 'NONE',  ( 59.13646009116148150, -70.47608876694609137, -4.999999999999997335 ) ) ;
#30436 = DIRECTION ( 'NONE',  ( 1.000000000000000000, 0.000000000000000000, 0.000000000000000000 ) ) ;
#30437 = ORIENTED_EDGE ( 'NONE', *, *, #17525, .T. ) ;
#30438 = ORIENTED_EDGE ( 'NONE', *, *, #16995, .F. ) ;
#30439 = CARTESIAN_POINT ( 'NONE',  ( 72.99999662536835388, -43.30127018922199511, 12.50000000000000000 ) ) ;
#30440 = CIRCLE ( 'NONE', #35248, 3.500000000000003109 ) ;
#30441 = CARTESIAN_POINT ( 'NONE',  ( -17.00000337463126243, 77.94228634059957983, -5.000000000000000000 ) ) ;
#30442 = EDGE_CURVE ( 'NONE', #13981, #2623, #5864, .T. ) ;
#30443 = DIRECTION ( 'NONE',  ( 0.000000000000000000, 0.000000000000000000, 1.000000000000000000 ) ) ;
#30444 = CARTESIAN_POINT ( 'NONE',  ( -35.19434990244938888, 52.39915983220783602, 12.49999999999999822 ) ) ;
#30445 = ORIENTED_EDGE ( 'NONE', *, *, #24791, .F. ) ;
#30446 = LINE ( 'NONE', #15645, #3943 ) ;
#30447 = AXIS2_PLACEMENT_3D ( 'NONE', #20245, #5816, #17255 ) ;
#30448 = EDGE_CURVE ( 'NONE', #29302, #550, #31596, .T. ) ;
#30449 = FACE_BOUND ( 'NONE', #29381, .T. ) ;
#30450 = AXIS2_PLACEMENT_3D ( 'NONE', #11264, #14808, #29036 ) ;
#30451 = DIRECTION ( 'NONE',  ( -0.000000000000000000, -0.000000000000000000, -1.000000000000000000 ) ) ;
#30452 = LINE ( 'NONE', #16571, #16602 ) ;
#30453 = DIRECTION ( 'NONE',  ( -1.000000000000000000, 0.000000000000000000, 0.000000000000000000 ) ) ;
#30455 = VECTOR ( 'NONE', #8718, 1000.000000000000000 ) ;
#30454 = DIRECTION ( 'NONE',  ( 0.000000000000000000, 0.000000000000000000, 1.000000000000000000 ) ) ;
#30456 = CARTESIAN_POINT ( 'NONE',  ( 81.99999662536832545, -17.32050807568879591, -9.999999999999998224 ) ) ;
#30457 = VECTOR ( 'NONE', #11409, 1000.000000000000114 ) ;
#30458 = CARTESIAN_POINT ( 'NONE',  ( 62.99999662536842493, 43.30127018922200222, -9.999999999999998224 ) ) ;
#30459 = VERTEX_POINT ( 'NONE', #15981 ) ;
#30460 = CARTESIAN_POINT ( 'NONE',  ( -62.00000337463104927, 34.64101615137757051, -9.999999999999998224 ) ) ;
#30461 = FACE_OUTER_BOUND ( 'NONE', #18663, .T. ) ;
#30462 = DIRECTION ( 'NONE',  ( 0.000000000000000000, 0.000000000000000000, -1.000000000000000000 ) ) ;
#30463 = AXIS2_PLACEMENT_3D ( 'NONE', #31506, #2854, #2650 ) ;
#30464 = VERTEX_POINT ( 'NONE', #30598 ) ;
#30465 = CIRCLE ( 'NONE', #28661, 2.000000000000000000 ) ;
#30466 = ORIENTED_EDGE ( 'NONE', *, *, #28585, .F. ) ;
#30467 = ORIENTED_EDGE ( 'NONE', *, *, #12494, .F. ) ;
#30468 = EDGE_CURVE ( 'NONE', #8340, #34827, #10679, .T. ) ;
#30469 = DIRECTION ( 'NONE',  ( 0.000000000000000000, 0.000000000000000000, -1.000000000000000000 ) ) ;
#30470 = CARTESIAN_POINT ( 'NONE',  ( -5.999999999999947597, 2.132877728683645235E-15, 32.50000000000000000 ) ) ;
#30471 = ORIENTED_EDGE ( 'NONE', *, *, #14446, .F. ) ;
#30472 = LINE ( 'NONE', #19591, #4153 ) ;
#30473 = AXIS2_PLACEMENT_3D ( 'NONE', #2413, #8406, #10662 ) ;
#30474 = CARTESIAN_POINT ( 'NONE',  ( -44.13139720814437794, -27.49999999999955591, -5.000000000000000888 ) ) ;
#30475 = ORIENTED_EDGE ( 'NONE', *, *, #23477, .F. ) ;
#30476 = DIRECTION ( 'NONE',  ( -1.000000000000000000, 0.000000000000000000, 0.000000000000000000 ) ) ;
#30477 = ADVANCED_BREP_SHAPE_REPRESENTATION ( '', ( #7743, #21385 ), #33942 ) ;
#30478 = ORIENTED_EDGE ( 'NONE', *, *, #18033, .T. ) ;
#30479 = AXIS2_PLACEMENT_3D ( 'NONE', #3130, #6299, #34644 ) ;
#30480 = CARTESIAN_POINT ( 'NONE',  ( 0.000000000000000000, 0.000000000000000000, 17.49999999999999645 ) ) ;
#30481 = EDGE_CURVE ( 'NONE', #24583, #7532, #14263, .T. ) ;
#30482 = CARTESIAN_POINT ( 'NONE',  ( -50.00000337463110611, -69.28203230275519786, 12.50000000000000000 ) ) ;
#30483 = DIRECTION ( 'NONE',  ( 0.000000000000000000, 0.000000000000000000, 1.000000000000000000 ) ) ;
#30484 = CARTESIAN_POINT ( 'NONE',  ( -70.00000337463102085, -34.64101615137762025, -5.000000000000000000 ) ) ;
#30485 = ADVANCED_FACE ( 'NONE', ( #33608 ), #1527, .F. ) ;
#30486 = EDGE_LOOP ( 'NONE', ( #37073, #1363, #34653, #7272, #32579 ) ) ;
#30487 = DIRECTION ( 'NONE',  ( 0.000000000000000000, 0.000000000000000000, 1.000000000000000000 ) ) ;
#30488 = ITEM_DEFINED_TRANSFORMATION ( 'NONE', 'NONE', #3979,  #21385 ) ;
#30489 = VECTOR ( 'NONE', #14035, 1000.000000000000000 ) ;
#30490 = EDGE_CURVE ( 'NONE', #8464, #28764, #6480, .T. ) ;
#30491 = DIRECTION ( 'NONE',  ( 1.000000000000000000, 0.000000000000000000, 0.000000000000000000 ) ) ;
#30492 = DIRECTION ( 'NONE',  ( 0.000000000000000000, 0.000000000000000000, 1.000000000000000000 ) ) ;
#30493 = CIRCLE ( 'NONE', #14328, 2.000000000000000000 ) ;
#30494 = ORIENTED_EDGE ( 'NONE', *, *, #33765, .F. ) ;
#30495 = CARTESIAN_POINT ( 'NONE',  ( -77.00000337463097821, 25.98076211353318854, -9.999999999999998224 ) ) ;
#30496 = DIRECTION ( 'NONE',  ( 0.000000000000000000, 0.000000000000000000, 1.000000000000000000 ) ) ;
#30497 = ORIENTED_EDGE ( 'NONE', *, *, #5423, .F. ) ;
#30498 = CIRCLE ( 'NONE', #25796, 3.000000000000002665 ) ;
#30499 = CARTESIAN_POINT ( 'NONE',  ( -8.000003374631249997, -86.60254037844400443, -9.999999999999998224 ) ) ;
#30500 = EDGE_CURVE ( 'NONE', #31944, #25427, #30428, .T. ) ;
#30501 = CARTESIAN_POINT ( 'NONE',  ( 0.000000000000000000, 0.000000000000000000, 27.50000000000000000 ) ) ;
#30502 = CARTESIAN_POINT ( 'NONE',  ( 82.99999662536832545, 8.660254037844394404, -9.999999999999998224 ) ) ;
#30503 = EDGE_CURVE ( 'NONE', #1195, #23444, #2083, .T. ) ;
#30504 = VERTEX_POINT ( 'NONE', #10179 ) ;
#30505 = CIRCLE ( 'NONE', #13154, 2.000000000000001776 ) ;
#30506 = ORIENTED_EDGE ( 'NONE', *, *, #33023, .F. ) ;
#30507 = CIRCLE ( 'NONE', #10146, 2.000000000000001776 ) ;
#30508 = DIRECTION ( 'NONE',  ( -1.000000000000000000, -0.000000000000000000, -0.000000000000000000 ) ) ;
#30509 = DIRECTION ( 'NONE',  ( 1.000000000000000000, 0.000000000000000000, 0.000000000000000000 ) ) ;
#30510 = EDGE_CURVE ( 'NONE', #2177, #20675, #34642, .T. ) ;
#30511 = ADVANCED_FACE ( 'NONE', ( #17075 ), #5471, .F. ) ;
#30512 = CARTESIAN_POINT ( 'NONE',  ( 47.63139720814400846, -27.50000000000022737, -5.000000000000000000 ) ) ;
#30513 = ORIENTED_EDGE ( 'NONE', *, *, #17219, .T. ) ;
#30514 = ORIENTED_EDGE ( 'NONE', *, *, #29976, .T. ) ;
#30515 = EDGE_CURVE ( 'NONE', #34980, #1135, #17278, .T. ) ;
#30516 = CARTESIAN_POINT ( 'NONE',  ( 145.0000000000000284, -6.000000000000504485, 32.55002500000000509 ) ) ;
#30517 = DIRECTION ( 'NONE',  ( -1.000000000000000000, 0.000000000000000000, 0.000000000000000000 ) ) ;
#30518 =( REPRESENTATION_RELATIONSHIP ('NONE','NONE', #15268, #35440 ) REPRESENTATION_RELATIONSHIP_WITH_TRANSFORMATION ( #27103 )SHAPE_REPRESENTATION_RELATIONSHIP( ) );
#30519 = EDGE_CURVE ( 'NONE', #24412, #2691, #7092, .T. ) ;
#30520 = DIRECTION ( 'NONE',  ( 1.000000000000000000, 0.000000000000000000, 0.000000000000000000 ) ) ;
#30522 = CARTESIAN_POINT ( 'NONE',  ( -106.8619802314695306, 52.03961299853113331, 32.50000000000000000 ) ) ;
#30521 = CIRCLE ( 'NONE', #35323, 1.999999999999998224 ) ;
#30523 = ORIENTED_EDGE ( 'NONE', *, *, #16075, .F. ) ;
#30524 = ORIENTED_EDGE ( 'NONE', *, *, #19451, .F. ) ;
#30525 = CARTESIAN_POINT ( 'NONE',  ( 4.999999999999999112, 2.886751345948153968, -0.5999999999999998668 ) ) ;
#30526 = VECTOR ( 'NONE', #13398, 1000.000000000000000 ) ;
#30527 = CARTESIAN_POINT ( 'NONE',  ( 49.99999662536846756, 69.28203230275516944, -5.000000000000000000 ) ) ;
#30528 = ORIENTED_EDGE ( 'NONE', *, *, #24552, .T. ) ;
#30529 = FACE_BOUND ( 'NONE', #209, .T. ) ;
#30530 = EDGE_LOOP ( 'NONE', ( #22531, #21942, #21322, #30638 ) ) ;
#30532 = AXIS2_PLACEMENT_3D ( 'NONE', #18971, #4730, #22326 ) ;
#30531 = DIRECTION ( 'NONE',  ( 0.000000000000000000, -0.5000000000000011102, -0.8660254037844379305 ) ) ;
#30533 = ADVANCED_FACE ( 'NONE', ( #27962 ), #25178, .F. ) ;
#30534 = DIRECTION ( 'NONE',  ( 0.000000000000000000, 0.000000000000000000, -1.000000000000000000 ) ) ;
#30535 = DIRECTION ( 'NONE',  ( 0.000000000000000000, 0.000000000000000000, 1.000000000000000000 ) ) ;
#30536 = EDGE_LOOP ( 'NONE', ( #1463, #34497, #21708, #13315, #17934 ) ) ;
#30537 = DIRECTION ( 'NONE',  ( -1.000000000000000000, 0.000000000000000000, 0.000000000000000000 ) ) ;
#30538 = CARTESIAN_POINT ( 'NONE',  ( -5.000003374631307729, 77.94228634059957983, -9.999999999999998224 ) ) ;
#30539 = CARTESIAN_POINT ( 'NONE',  ( -6.123233995736731770E-16, 145.0000000000000568, 32.50000000000000000 ) ) ;
#30540 = ORIENTED_EDGE ( 'NONE', *, *, #33249, .T. ) ;
#30541 = DIRECTION ( 'NONE',  ( -1.000000000000000000, 0.000000000000000000, -0.000000000000000000 ) ) ;
#30542 = EDGE_CURVE ( 'NONE', #12595, #21994, #8632, .T. ) ;
#30543 = CARTESIAN_POINT ( 'NONE',  ( -101.8947913453489349, 31.99226454438814571, 32.50000000000000711 ) ) ;
#30544 = CARTESIAN_POINT ( 'NONE',  ( -5.854691731421723944E-14, -5.773502691896269745, -0.5999999999999998668 ) ) ;
#30545 = AXIS2_PLACEMENT_3D ( 'NONE', #15850, #27277, #30476 ) ;
#30546 = ORIENTED_EDGE ( 'NONE', *, *, #25449, .T. ) ;
#30547 = VERTEX_POINT ( 'NONE', #25340 ) ;
#30548 = ORIENTED_EDGE ( 'NONE', *, *, #22476, .F. ) ;
#30549 = AXIS2_PLACEMENT_3D ( 'NONE', #32288, #9219, #14491 ) ;
#30550 = CARTESIAN_POINT ( 'NONE',  ( 74.99999662536835388, -43.30127018922199511, 17.49999999999999645 ) ) ;
#30551 = ORIENTED_EDGE ( 'NONE', *, *, #5728, .T. ) ;
#30552 = DIRECTION ( 'NONE',  ( 0.000000000000000000, 0.000000000000000000, -1.000000000000000000 ) ) ;
#30553 = CARTESIAN_POINT ( 'NONE',  ( -5.000000000000000888, -2.886751345948150860, -0.5999999999999998668 ) ) ;
#30554 = EDGE_CURVE ( 'NONE', #10919, #20978, #23067, .T. ) ;
#30555 = CARTESIAN_POINT ( 'NONE',  ( 1.432312439535579074, 4.946556719366745014, -0.1121614189353384305 ) ) ;
#30556 = EDGE_CURVE ( 'NONE', #10919, #8273, #20252, .T. ) ;
#30557 = AXIS2_PLACEMENT_3D ( 'NONE', #18326, #3883, #14773 ) ;
#30558 = EDGE_CURVE ( 'NONE', #21666, #16670, #183, .T. ) ;
#30559 = DIRECTION ( 'NONE',  ( -1.000000000000000000, 0.000000000000000000, 0.000000000000000000 ) ) ;
#30560 = CARTESIAN_POINT ( 'NONE',  ( -19.31922176934808633, 76.99660315353983719, -11.00000000000000000 ) ) ;
#30561 = CARTESIAN_POINT ( 'NONE',  ( -3.374631334790434423E-06, 69.28203230275516944, -5.000000000000000000 ) ) ;
#30562 = CIRCLE ( 'NONE', #18579, 2.000000000000001776 ) ;
#30563 = DIRECTION ( 'NONE',  ( -0.000000000000000000, -0.000000000000000000, -1.000000000000000000 ) ) ;
#30564 = CARTESIAN_POINT ( 'NONE',  ( -32.00000337463119848, -69.28203230275522628, -9.999999999999998224 ) ) ;
#30565 = ORIENTED_EDGE ( 'NONE', *, *, #35889, .T. ) ;
#30566 = ORIENTED_EDGE ( 'NONE', *, *, #4999, .F. ) ;
#30567 =( NAMED_UNIT ( * ) PLANE_ANGLE_UNIT ( ) SI_UNIT ( $, .RADIAN. ) );
#30568 = DIRECTION ( 'NONE',  ( -1.000000000000000000, 0.000000000000000000, 0.000000000000000000 ) ) ;
#30569 = DIRECTION ( 'NONE',  ( 1.000000000000000000, 0.000000000000000000, 0.000000000000000000 ) ) ;
#30570 = AXIS2_PLACEMENT_3D ( 'NONE', #8681, #20121, #31549 ) ;
#30571 = DIRECTION ( 'NONE',  ( 1.000000000000000000, 0.000000000000000000, 0.000000000000000000 ) ) ;
#30572 = ORIENTED_EDGE ( 'NONE', *, *, #34824, .T. ) ;
#30573 = UNCERTAINTY_MEASURE_WITH_UNIT (LENGTH_MEASURE( 1.000000000000000082E-05 ), #33209, 'distance_accuracy_value', 'NONE');
#30574 = DIRECTION ( 'NONE',  ( 1.000000000000000000, 0.000000000000000000, 0.000000000000000000 ) ) ;
#30575 = DIRECTION ( 'NONE',  ( 1.000000000000000000, 0.000000000000000000, 0.000000000000000000 ) ) ;
#30576 = ORIENTED_EDGE ( 'NONE', *, *, #7829, .T. ) ;
#30577 = CYLINDRICAL_SURFACE ( 'NONE', #21222, 2.000000000000001776 ) ;
#30578 = CIRCLE ( 'NONE', #13124, 2.000000000000001776 ) ;
#30579 = VERTEX_POINT ( 'NONE', #28704 ) ;
#30580 = EDGE_CURVE ( 'NONE', #3218, #23996, #29834, .T. ) ;
#30581 = PLANE ( 'NONE',  #25302 ) ;
#30582 = CARTESIAN_POINT ( 'NONE',  ( 44.13139720814401556, -27.50000000000022737, -10.00000000000000000 ) ) ;
#30583 = CARTESIAN_POINT ( 'NONE',  ( -48.00000337463110611, -69.28203230275519786, -5.000000000000000000 ) ) ;
#30584 = ORIENTED_EDGE ( 'NONE', *, *, #10425, .F. ) ;
#30585 = ORIENTED_EDGE ( 'NONE', *, *, #32068, .T. ) ;
#30586 = EDGE_LOOP ( 'NONE', ( #12174, #19679 ) ) ;
#30587 = CARTESIAN_POINT ( 'NONE',  ( -82.00000337463094979, -17.32050807568882078, -9.999999999999998224 ) ) ;
#30588 = CARTESIAN_POINT ( 'NONE',  ( 41.99999662536853151, 69.28203230275518365, -5.000000000000000000 ) ) ;
#30589 = DIRECTION ( 'NONE',  ( -1.000000000000000000, 0.000000000000000000, 0.000000000000000000 ) ) ;
#30590 = DIRECTION ( 'NONE',  ( 0.000000000000000000, 0.000000000000000000, 1.000000000000000000 ) ) ;
#30591 = CARTESIAN_POINT ( 'NONE',  ( 16.49657687835809128, -93.55673653615983199, -5.000000000000000000 ) ) ;
#30592 = ORIENTED_EDGE ( 'NONE', *, *, #32863, .F. ) ;
#30593 = CARTESIAN_POINT ( 'NONE',  ( 64.99999662536839651, -60.62177826491080168, 12.50000000000000000 ) ) ;
#30594 = CARTESIAN_POINT ( 'NONE',  ( 4.654160418576254177E-15, -6.066067634115602125, -4.359491423763670603 ) ) ;
#30595 = ADVANCED_FACE ( 'NONE', ( #5837 ), #3032, .F. ) ;
#30596 = LINE ( 'NONE', #18787, #9203 ) ;
#30597 = EDGE_LOOP ( 'NONE', ( #3573, #27761, #28511, #7997 ) ) ;
#30598 = CARTESIAN_POINT ( 'NONE',  ( 45.00000000000000000, 5.510910596163089556E-15, -15.00000000000000000 ) ) ;
#30599 = DIRECTION ( 'NONE',  ( 1.000000000000000000, 0.000000000000000000, 0.000000000000000000 ) ) ;
#30600 = VERTEX_POINT ( 'NONE', #33975 ) ;
#30601 = VERTEX_POINT ( 'NONE', #20266 ) ;
#30602 = DIRECTION ( 'NONE',  ( 0.000000000000000000, 0.000000000000000000, -1.000000000000000000 ) ) ;
#30603 = DIRECTION ( 'NONE',  ( 1.000000000000000000, 0.000000000000000000, 0.000000000000000000 ) ) ;
#30604 = DIRECTION ( 'NONE',  ( 0.000000000000000000, 0.000000000000000000, 1.000000000000000000 ) ) ;
#30605 = ORIENTED_EDGE ( 'NONE', *, *, #11488, .F. ) ;
#30606 = EDGE_LOOP ( 'NONE', ( #10361, #30839 ) ) ;
#30607 = CARTESIAN_POINT ( 'NONE',  ( -5.000003374631307729, 77.94228634059957983, -9.999999999999998224 ) ) ;
#30608 = ORIENTED_EDGE ( 'NONE', *, *, #6139, .F. ) ;
#30609 = CIRCLE ( 'NONE', #36035, 2.000000000000001776 ) ;
#30610 = LINE ( 'NONE', #11294, #1026 ) ;
#30611 = EDGE_LOOP ( 'NONE', ( #19585, #15705, #4826, #18965 ) ) ;
#30612 = EDGE_CURVE ( 'NONE', #7366, #17904, #14070, .T. ) ;
#30613 = ORIENTED_EDGE ( 'NONE', *, *, #37020, .T. ) ;
#30614 = DIRECTION ( 'NONE',  ( -1.000000000000000000, 0.000000000000000000, -0.000000000000000000 ) ) ;
#30615 = FACE_BOUND ( 'NONE', #24155, .T. ) ;
#30616 = ORIENTED_EDGE ( 'NONE', *, *, #4118, .T. ) ;
#30617 = VERTEX_POINT ( 'NONE', #2641 ) ;
#30618 = FACE_OUTER_BOUND ( 'NONE', #35943, .T. ) ;
#30619 = DIRECTION ( 'NONE',  ( 1.000000000000000000, 0.000000000000000000, 0.000000000000000000 ) ) ;
#30620 = LINE ( 'NONE', #33806, #28248 ) ;
#30621 = DIRECTION ( 'NONE',  ( 0.000000000000000000, 0.000000000000000000, 1.000000000000000000 ) ) ;
#30622 = ADVANCED_FACE ( 'NONE', ( #16729 ), #8824, .T. ) ;
#30623 = VERTEX_POINT ( 'NONE', #8462 ) ;
#30624 = FACE_OUTER_BOUND ( 'NONE', #5987, .T. ) ;
#30625 = CARTESIAN_POINT ( 'NONE',  ( -85.00000337463092137, -25.98076211353322051, -9.999999999999998224 ) ) ;
#30626 = CARTESIAN_POINT ( 'NONE',  ( 74.99999662536836809, 8.660254037844394404, -5.000000000000000000 ) ) ;
#30627 = CARTESIAN_POINT ( 'NONE',  ( 74.99999662536835388, -43.30127018922199511, -9.999999999999998224 ) ) ;
#30628 = FACE_OUTER_BOUND ( 'NONE', #3073, .T. ) ;
#30629 = CARTESIAN_POINT ( 'NONE',  ( -63.00000337463106348, -60.62177826491083010, 17.49999999999999645 ) ) ;
#30630 = CARTESIAN_POINT ( 'NONE',  ( 18.28331374579376956, 112.2394282457694459, 27.49998799999999832 ) ) ;
#30631 = ADVANCED_FACE ( 'NONE', ( #2474 ), #5089, .T. ) ;
#30632 = LINE ( 'NONE', #30458, #19950 ) ;
#30633 = ORIENTED_EDGE ( 'NONE', *, *, #1069, .T. ) ;
#30634 = DIRECTION ( 'NONE',  ( 0.000000000000000000, 0.000000000000000000, 1.000000000000000000 ) ) ;
#30635 = AXIS2_PLACEMENT_3D ( 'NONE', #31162, #31505, #6033 ) ;
#30636 = DIRECTION ( 'NONE',  ( 1.000000000000000000, 0.000000000000000000, 0.000000000000000000 ) ) ;
#30637 = DIRECTION ( 'NONE',  ( 0.000000000000000000, 0.000000000000000000, 1.000000000000000000 ) ) ;
#30638 = ORIENTED_EDGE ( 'NONE', *, *, #21309, .T. ) ;
#30639 = ORIENTED_EDGE ( 'NONE', *, *, #22437, .T. ) ;
#30640 = EDGE_LOOP ( 'NONE', ( #19993, #26132, #21986, #30186 ) ) ;
#30641 = DIRECTION ( 'NONE',  ( 1.000000000000000000, 0.000000000000000000, 0.000000000000000000 ) ) ;
#30642 = DIRECTION ( 'NONE',  ( 0.000000000000000000, 0.000000000000000000, 1.000000000000000000 ) ) ;
#30643 = VERTEX_POINT ( 'NONE', #13720 ) ;
#30644 = ADVANCED_FACE ( 'NONE', ( #20 ), #22338, .F. ) ;
#30645 = CARTESIAN_POINT ( 'NONE',  ( -17.55872235085559652, 89.94802294027088863, -24.99999999999999645 ) ) ;
#30646 = LINE ( 'NONE', #34898, #3924 ) ;
#30647 = EDGE_LOOP ( 'NONE', ( #36597, #13949 ) ) ;
#30648 = EDGE_CURVE ( 'NONE', #6013, #12103, #22521, .T. ) ;
#30649 = FACE_BOUND ( 'NONE', #30077, .T. ) ;
#30650 = VERTEX_POINT ( 'NONE', #34715 ) ;
#30651 = LINE ( 'NONE', #36487, #995 ) ;
#30652 = ADVANCED_FACE ( 'NONE', ( #571 ), #29606, .F. ) ;
#30653 = CARTESIAN_POINT ( 'NONE',  ( 86.99999662536831124, -25.98076211353319565, -5.000000000000000000 ) ) ;
#30654 = DIRECTION ( 'NONE',  ( 0.000000000000000000, 0.000000000000000000, 1.000000000000000000 ) ) ;
#30655 = AXIS2_PLACEMENT_3D ( 'NONE', #31351, #31190, #20302 ) ;
#30656 = ADVANCED_FACE ( 'NONE', ( #14820 ), #29430, .T. ) ;
#30657 = ORIENTED_EDGE ( 'NONE', *, *, #22844, .F. ) ;
#30658 = FACE_OUTER_BOUND ( 'NONE', #21028, .T. ) ;
#30659 = CONTEXT_DEPENDENT_SHAPE_REPRESENTATION ( #23344, #32525 ) ;
#30660 = DIRECTION ( 'NONE',  ( 1.000000000000000000, 0.000000000000000000, 0.000000000000000000 ) ) ;
#30661 = DIRECTION ( 'NONE',  ( 0.000000000000000000, 0.000000000000000000, 1.000000000000000000 ) ) ;
#30662 = ADVANCED_FACE ( 'NONE', ( #23265 ), #931, .F. ) ;
#30663 = VERTEX_POINT ( 'NONE', #3749 ) ;
#30664 = CARTESIAN_POINT ( 'NONE',  ( -87.00000337463093558, 25.98076211353317433, 17.49999999999999645 ) ) ;
#30665 = CARTESIAN_POINT ( 'NONE',  ( -20.00000000000001066, 89.94802294027088863, -19.99999999999999645 ) ) ;
#30666 = ORIENTED_EDGE ( 'NONE', *, *, #10739, .F. ) ;
#30667 = CYLINDRICAL_SURFACE ( 'NONE', #452, 2.000000000000001776 ) ;
#30668 = LINE ( 'NONE', #11354, #19096 ) ;
#30669 = CARTESIAN_POINT ( 'NONE',  ( 69.99999662536838230, -34.64101615137759183, -9.999999999999998224 ) ) ;
#30670 = AXIS2_PLACEMENT_3D ( 'NONE', #36229, #12973, #24431 ) ;
#30671 = ORIENTED_EDGE ( 'NONE', *, *, #29868, .F. ) ;
#30672 = ORIENTED_EDGE ( 'NONE', *, *, #3019, .F. ) ;
#30673 = DIRECTION ( 'NONE',  ( 0.000000000000000000, 0.000000000000000000, 1.000000000000000000 ) ) ;
#30674 = CARTESIAN_POINT ( 'NONE',  ( -55.00000337463107059, 43.30127018922197379, 17.49999999999999645 ) ) ;
#30675 = CARTESIAN_POINT ( 'NONE',  ( 72.28378166042060116, 61.53067111003190348, 12.49999999999999822 ) ) ;
#30676 = EDGE_CURVE ( 'NONE', #5735, #9729, #13673, .T. ) ;
#30677 = ORIENTED_EDGE ( 'NONE', *, *, #6856, .F. ) ;
#30678 = ORIENTED_EDGE ( 'NONE', *, *, #18493, .T. ) ;
#30679 = AXIS2_PLACEMENT_3D ( 'NONE', #4875, #30552, #27158 ) ;
#30680 = CARTESIAN_POINT ( 'NONE',  ( 44.13139720814420031, 27.49999999999988987, -5.000000000000000000 ) ) ;
#30681 = CARTESIAN_POINT ( 'NONE',  ( -4.829002333675109782, 2.985476894631601485, -1.879366290983708110 ) ) ;
#30682 = CARTESIAN_POINT ( 'NONE',  ( 40.98360655737705116, 111.1639425680974398, -19.99999999999999645 ) ) ;
#30683 = CARTESIAN_POINT ( 'NONE',  ( 34.99999662536853862, 77.94228634059959404, -9.999999999999998224 ) ) ;
#30684 = ORIENTED_EDGE ( 'NONE', *, *, #22199, .T. ) ;
#30685 = EDGE_CURVE ( 'NONE', #9891, #33338, #21465, .T. ) ;
#30686 = ORIENTED_EDGE ( 'NONE', *, *, #24375, .T. ) ;
#30687 = DIRECTION ( 'NONE',  ( 1.000000000000000000, 0.000000000000000000, 0.000000000000000000 ) ) ;
#30688 = ORIENTED_EDGE ( 'NONE', *, *, #2564, .F. ) ;
#30689 = ADVANCED_FACE ( 'NONE', ( #24010 ), #11992, .T. ) ;
#30690 = FACE_OUTER_BOUND ( 'NONE', #13478, .T. ) ;
#30691 = ORIENTED_EDGE ( 'NONE', *, *, #22659, .F. ) ;
#30692 = DIRECTION ( 'NONE',  ( 1.000000000000000000, 0.000000000000000000, 0.000000000000000000 ) ) ;
#30693 = VECTOR ( 'NONE', #8638, 1000.000000000000000 ) ;
#30694 = DIRECTION ( 'NONE',  ( 0.000000000000000000, 0.000000000000000000, 1.000000000000000000 ) ) ;
#30695 = B_SPLINE_CURVE_WITH_KNOTS ( 'NONE', 3,
 ( #18914, #30543, #16293, #32069, #29278, #15035, #26461, #21720, #35101, #1667, #13104, #32981 ),
 .UNSPECIFIED., .F., .F.,
 ( 4, 2, 1, 2, 2, 1, 4 ),
 ( 0.05563282717590184445, 0.06951991305345063543, 0.08340699893099942641, 0.1111811706860971471, 0.1250682565636460630, 0.1389553424411949512, 0.1667295141962928384 ),
 .UNSPECIFIED. ) ;
#30696 = CARTESIAN_POINT ( 'NONE',  ( 5.211749180171790563, 2.764497899775259171, -4.027903350935051030 ) ) ;
#30697 = VERTEX_POINT ( 'NONE', #29250 ) ;
#30698 = B_SPLINE_CURVE_WITH_KNOTS ( 'NONE', 3,
 ( #20120, #31896, #31548, #26309, #17323, #28749, #620, #3075, #14496, #18217 ),
 .UNSPECIFIED., .F., .F.,
 ( 4, 2, 2, 2, 4 ),
 ( 0.000000000000000000, 0.001528561485809837783, 0.003057122971619675132, 0.004585684457429512265, 0.006114245943239348530 ),
 .UNSPECIFIED. ) ;
#30699 =( NAMED_UNIT ( * ) PLANE_ANGLE_UNIT ( ) SI_UNIT ( $, .RADIAN. ) );
#30700 = CARTESIAN_POINT ( 'NONE',  ( 72.99999662536836809, 25.98076211353319565, 12.50000000000000000 ) ) ;
#30701 = EDGE_CURVE ( 'NONE', #12539, #27066, #28042, .T. ) ;
#30702 = AXIS2_PLACEMENT_3D ( 'NONE', #11024, #22461, #17020 ) ;
#30703 = FACE_OUTER_BOUND ( 'NONE', #15187, .T. ) ;
#30704 = FACE_OUTER_BOUND ( 'NONE', #16512, .T. ) ;
#30705 = ORIENTED_EDGE ( 'NONE', *, *, #27169, .F. ) ;
#30706 = AXIS2_PLACEMENT_3D ( 'NONE', #8876, #34573, #17324 ) ;
#30707 = FACE_OUTER_BOUND ( 'NONE', #6665, .T. ) ;
#30708 = CARTESIAN_POINT ( 'NONE',  ( 86.99999662536832545, 8.660254037844394404, 17.49999999999999645 ) ) ;
#30709 = CARTESIAN_POINT ( 'NONE',  ( -48.00000337463110611, -69.28203230275519786, 12.50000000000000000 ) ) ;
#30710 = VERTEX_POINT ( 'NONE', #3383 ) ;
#30711 = ORIENTED_EDGE ( 'NONE', *, *, #11855, .T. ) ;
#30712 = CARTESIAN_POINT ( 'NONE',  ( 79.99999662536832545, -17.32050807568879591, -5.000000000000000000 ) ) ;
#30713 = EDGE_LOOP ( 'NONE', ( #6000, #31174 ) ) ;
#30714 = DIRECTION ( 'NONE',  ( 0.000000000000000000, 0.000000000000000000, -1.000000000000000000 ) ) ;
#30715 = CIRCLE ( 'NONE', #25937, 2.000000000000001776 ) ;
#30716 = CARTESIAN_POINT ( 'NONE',  ( 84.99999662536832545, 8.660254037844394404, -9.999999999999998224 ) ) ;
#30717 = AXIS2_PLACEMENT_3D ( 'NONE', #36016, #10308, #32438 ) ;
#30718 = DIRECTION ( 'NONE',  ( 0.8660254037844344888, -0.5000000000000069944, 0.000000000000000000 ) ) ;
#30719 = EDGE_CURVE ( 'NONE', #35067, #36125, #24441, .T. ) ;
#30720 = DIRECTION ( 'NONE',  ( 1.000000000000000000, 0.000000000000000000, 0.000000000000000000 ) ) ;
#30721 = FACE_OUTER_BOUND ( 'NONE', #6466, .T. ) ;
#30722 = CYLINDRICAL_SURFACE ( 'NONE', #4555, 2.000000000000000000 ) ;
#30723 = EDGE_CURVE ( 'NONE', #2483, #31393, #4694, .T. ) ;
#30724 = DIRECTION ( 'NONE',  ( 1.000000000000000000, 0.000000000000000000, 0.000000000000000000 ) ) ;
#30725 = CARTESIAN_POINT ( 'NONE',  ( 74.99999662536836809, 25.98076211353319565, -9.999999999999998224 ) ) ;
#30726 = ORIENTED_EDGE ( 'NONE', *, *, #8510, .F. ) ;
#30727 = EDGE_CURVE ( 'NONE', #25733, #15477, #6026, .T. ) ;
#30728 = ORIENTED_EDGE ( 'NONE', *, *, #3575, .T. ) ;
#30729 = FILL_AREA_STYLE_COLOUR ( '', #33864 ) ;
#30730 = CIRCLE ( 'NONE', #6797, 1.999999999999998224 ) ;
#30731 = DIRECTION ( 'NONE',  ( 1.000000000000000000, 0.000000000000000000, 0.000000000000000000 ) ) ;
#30732 = CYLINDRICAL_SURFACE ( 'NONE', #29421, 2.000000000000001776 ) ;
#30733 = LINE ( 'NONE', #21744, #24563 ) ;
#30734 = ADVANCED_FACE ( 'NONE', ( #9743 ), #12556, .F. ) ;
#30735 = EDGE_LOOP ( 'NONE', ( #13519, #32831, #2228, #13818 ) ) ;
#30736 = EDGE_CURVE ( 'NONE', #4, #5148, #11865, .T. ) ;
#30737 = CARTESIAN_POINT ( 'NONE',  ( 4.999999999999999112, -0.1416384297035287454, -0.5080592402122392492 ) ) ;
#30738 = VERTEX_POINT ( 'NONE', #9177 ) ;
#30739 = FACE_OUTER_BOUND ( 'NONE', #26656, .T. ) ;
#30740 = EDGE_LOOP ( 'NONE', ( #3702, #17349 ) ) ;
#30741 = EDGE_CURVE ( 'NONE', #18729, #19586, #17814, .T. ) ;
#30742 =( LENGTH_UNIT ( ) NAMED_UNIT ( * ) SI_UNIT ( .MILLI., .METRE. ) );
#30743 = DIRECTION ( 'NONE',  ( 1.000000000000000000, 0.000000000000000000, 0.000000000000000000 ) ) ;
#30744 = EDGE_CURVE ( 'NONE', #9425, #15109, #22062, .T. ) ;
#30745 = VECTOR ( 'NONE', #36382, 1000.000000000000000 ) ;
#30746 = DIRECTION ( 'NONE',  ( 0.000000000000000000, 0.000000000000000000, 1.000000000000000000 ) ) ;
#30747 = ADVANCED_FACE ( 'NONE', ( #17614 ), #29046, .F. ) ;
#30748 = DIRECTION ( 'NONE',  ( 0.000000000000000000, 0.000000000000000000, -1.000000000000000000 ) ) ;
#30749 = EDGE_CURVE ( 'NONE', #10183, #6568, #32245, .T. ) ;
#30750 = ORIENTED_EDGE ( 'NONE', *, *, #36193, .F. ) ;
#30751 = ORIENTED_EDGE ( 'NONE', *, *, #10829, .T. ) ;
#30752 = CIRCLE ( 'NONE', #14582, 2.000000000000001776 ) ;
#30753 = EDGE_LOOP ( 'NONE', ( #28301, #28060, #2558, #24518 ) ) ;
#30754 = DIRECTION ( 'NONE',  ( 1.000000000000000000, 0.000000000000000000, 0.000000000000000000 ) ) ;
#30755 = AXIS2_PLACEMENT_3D ( 'NONE', #32651, #4351, #9424 ) ;
#30756 = DIRECTION ( 'NONE',  ( 0.000000000000000000, 0.000000000000000000, -1.000000000000000000 ) ) ;
#30757 = DIRECTION ( 'NONE',  ( 1.000000000000000000, 0.000000000000000000, 0.000000000000000000 ) ) ;
#30758 = CYLINDRICAL_SURFACE ( 'NONE', #10928, 2.000000000000001776 ) ;
#30759 = CARTESIAN_POINT ( 'NONE',  ( 4.999999999999999112, -2.119101676855895899, -3.842106124101172249 ) ) ;
#30760 = VERTEX_POINT ( 'NONE', #12920 ) ;
#30761 = AXIS2_PLACEMENT_3D ( 'NONE', #18661, #21470, #26357 ) ;
#30762 = LINE ( 'NONE', #25716, #29603 ) ;
#30763 = PRODUCT_DEFINITION_SHAPE ( 'NONE', 'NONE',  #37127 ) ;
#30764 = CARTESIAN_POINT ( 'NONE',  ( -45.00000337463111322, -77.94228634059960825, -5.000000000000000000 ) ) ;
#30765 = ORIENTED_EDGE ( 'NONE', *, *, #8716, .T. ) ;
#30766 = DIRECTION ( 'NONE',  ( 0.000000000000000000, 0.000000000000000000, -1.000000000000000000 ) ) ;
#30767 = DIRECTION ( 'NONE',  ( 1.000000000000000000, 0.000000000000000000, 0.000000000000000000 ) ) ;
#30768 = EDGE_LOOP ( 'NONE', ( #34132, #19152, #25193, #9538, #15356 ) ) ;
#30769 = CIRCLE ( 'NONE', #6202, 2.000000000000001776 ) ;
#30770 = ORIENTED_EDGE ( 'NONE', *, *, #34907, .F. ) ;
#30771 = DIRECTION ( 'NONE',  ( 0.000000000000000000, 0.000000000000000000, 1.000000000000000000 ) ) ;
#30772 = CARTESIAN_POINT ( 'NONE',  ( -5.211749180171789675, 2.764497899775240519, -4.027903350935047477 ) ) ;
#30773 = FACE_OUTER_BOUND ( 'NONE', #24480, .T. ) ;
#30774 = CARTESIAN_POINT ( 'NONE',  ( -106.6136243914056507, -41.75127244461555875, 32.50000000000000000 ) ) ;
#30775 = EDGE_LOOP ( 'NONE', ( #34592, #16585, #34381, #1964 ) ) ;
#30776 = ORIENTED_EDGE ( 'NONE', *, *, #27061, .T. ) ;
#30777 = LINE ( 'NONE', #13906, #5144 ) ;
#30778 = AXIS2_PLACEMENT_3D ( 'NONE', #29804, #1305, #27364 ) ;
#30779 = ORIENTED_EDGE ( 'NONE', *, *, #26612, .T. ) ;
#30780 = CARTESIAN_POINT ( 'NONE',  ( 0.000000000000000000, 0.000000000000000000, 12.49999999999999822 ) ) ;
#30781 = ORIENTED_EDGE ( 'NONE', *, *, #25324, .F. ) ;
#30782 = ORIENTED_EDGE ( 'NONE', *, *, #493, .F. ) ;
#30783 = CARTESIAN_POINT ( 'NONE',  ( -56.67878100130369035, 27.78182860042797131, 12.49999999999999822 ) ) ;
#30784 = DIRECTION ( 'NONE',  ( 0.000000000000000000, 0.000000000000000000, 1.000000000000000000 ) ) ;
#30785 = ADVANCED_FACE ( 'NONE', ( #27722 ), #27563, .F. ) ;
#30786 = VERTEX_POINT ( 'NONE', #18931 ) ;
#30787 = ORIENTED_EDGE ( 'NONE', *, *, #17122, .T. ) ;
#30788 = DIRECTION ( 'NONE',  ( -0.000000000000000000, 1.000000000000000000, 0.000000000000000000 ) ) ;
#30789 = DIRECTION ( 'NONE',  ( 0.000000000000000000, 0.000000000000000000, -1.000000000000000000 ) ) ;
#30790 = CARTESIAN_POINT ( 'NONE',  ( 0.000000000000000000, 3.050000000000000711, 2.266666666666999674 ) ) ;
#30791 = CARTESIAN_POINT ( 'NONE',  ( -5.244818697407747976, 2.029379090245544415, -4.190884354498993325 ) ) ;
#30792 = ORIENTED_EDGE ( 'NONE', *, *, #8986, .T. ) ;
#30793 = DIRECTION ( 'NONE',  ( 1.000000000000000000, 0.000000000000000000, 0.000000000000000000 ) ) ;
#30794 = FACE_BOUND ( 'NONE', #28837, .T. ) ;
#30795 = DIRECTION ( 'NONE',  ( -1.000000000000000000, 0.000000000000000000, 0.000000000000000000 ) ) ;
#30796 = FACE_OUTER_BOUND ( 'NONE', #23371, .T. ) ;
#30797 = DIRECTION ( 'NONE',  ( 0.000000000000000000, 0.000000000000000000, -1.000000000000000000 ) ) ;
#30798 = CARTESIAN_POINT ( 'NONE',  ( 56.29165124598846859, -32.50000000000006395, 12.49999999999999822 ) ) ;
#30799 = CIRCLE ( 'NONE', #11625, 3.000000000000006217 ) ;
#30800 = CIRCLE ( 'NONE', #12231, 2.000000000000000000 ) ;
#30801 = CARTESIAN_POINT ( 'NONE',  ( 49.99999662536846756, -69.28203230275519786, -9.999999999999998224 ) ) ;
#30802 = DIRECTION ( 'NONE',  ( 0.000000000000000000, 0.000000000000000000, 1.000000000000000000 ) ) ;
#30803 = VERTEX_POINT ( 'NONE', #18578 ) ;
#30804 = CARTESIAN_POINT ( 'NONE',  ( -5.000000000000000888, -1.936377641173862463, -5.802630826755077464 ) ) ;
#30805 = CARTESIAN_POINT ( 'NONE',  ( 47.99999662536846756, 69.28203230275516944, -9.999999999999998224 ) ) ;
#30806 = CYLINDRICAL_SURFACE ( 'NONE', #25921, 2.000000000000001776 ) ;
#30807 = EDGE_CURVE ( 'NONE', #33375, #14832, #4721, .T. ) ;
#30808 = EDGE_CURVE ( 'NONE', #1450, #16018, #2039, .T. ) ;
#30809 = VERTEX_POINT ( 'NONE', #16306 ) ;
#30810 = ORIENTED_EDGE ( 'NONE', *, *, #5884, .F. ) ;
#30811 = ORIENTED_EDGE ( 'NONE', *, *, #21128, .F. ) ;
#30812 = AXIS2_PLACEMENT_3D ( 'NONE', #12093, #23391, #18110 ) ;
#30813 = CARTESIAN_POINT ( 'NONE',  ( -3.000000000000000000, 3.673940397442059868E-16, -6.000000000000001776 ) ) ;
#30814 = DIRECTION ( 'NONE',  ( 0.000000000000000000, 0.000000000000000000, 1.000000000000000000 ) ) ;
#30815 = ORIENTED_EDGE ( 'NONE', *, *, #8202, .F. ) ;
#30816 = VECTOR ( 'NONE', #15576, 1000.000000000000000 ) ;
#30817 = DIRECTION ( 'NONE',  ( -0.000000000000000000, -0.000000000000000000, 1.000000000000000000 ) ) ;
#30818 = EDGE_CURVE ( 'NONE', #23401, #13703, #17295, .T. ) ;
#30819 = DIRECTION ( 'NONE',  ( 0.000000000000000000, 0.000000000000000000, 1.000000000000000000 ) ) ;
#30820 = VERTEX_POINT ( 'NONE', #36008 ) ;
#30821 = CARTESIAN_POINT ( 'NONE',  ( 23.02815535700703364, -104.7522195559561595, 32.49999999999999289 ) ) ;
#30822 = ORIENTED_EDGE ( 'NONE', *, *, #35042, .F. ) ;
#30823 = FACE_OUTER_BOUND ( 'NONE', #17224, .T. ) ;
#30824 = CIRCLE ( 'NONE', #24248, 2.000000000000001776 ) ;
#30825 = CIRCLE ( 'NONE', #14074, 3.000000000000002665 ) ;
#30826 = CARTESIAN_POINT ( 'NONE',  ( -5.000003374631269537, -77.94228634059960825, 17.49999999999999645 ) ) ;
#30827 = DIRECTION ( 'NONE',  ( -1.000000000000000000, 0.000000000000000000, 0.000000000000000000 ) ) ;
#30828 = ADVANCED_FACE ( 'NONE', ( #1867 ), #27167, .F. ) ;
#30829 = VERTEX_POINT ( 'NONE', #7685 ) ;
#30830 = CARTESIAN_POINT ( 'NONE',  ( -98.28784258492883907, 106.7731239591698937, 32.55002500000000509 ) ) ;
#30831 = B_SPLINE_CURVE_WITH_KNOTS ( 'NONE', 3,
 ( #34982, #11913, #29162, #14728, #34808, #9280 ),
 .UNSPECIFIED., .F., .F.,
 ( 4, 2, 4 ),
 ( 0.000000000000000000, 0.0002514304509865748229, 0.0005028609019731496458 ),
 .UNSPECIFIED. ) ;
#30832 = CONTEXT_DEPENDENT_SHAPE_REPRESENTATION ( #6780, #24488 ) ;
#30833 = DIRECTION ( 'NONE',  ( 0.000000000000000000, 0.000000000000000000, 1.000000000000000000 ) ) ;
#30834 = DIRECTION ( 'NONE',  ( 1.000000000000000000, 0.000000000000000000, 0.000000000000000000 ) ) ;
#30835 = CIRCLE ( 'NONE', #2718, 30.00000000000000000 ) ;
#30836 = VERTEX_POINT ( 'NONE', #36373 ) ;
#30837 = DIRECTION ( 'NONE',  ( 1.000000000000000000, 0.000000000000000000, 0.000000000000000000 ) ) ;
#30838 = DIRECTION ( 'NONE',  ( 1.000000000000000000, 0.000000000000000000, 0.000000000000000000 ) ) ;
#30839 = ORIENTED_EDGE ( 'NONE', *, *, #36702, .F. ) ;
#30840 = CARTESIAN_POINT ( 'NONE',  ( 31.46585318596250502, 86.45172111230321832, 12.49999999999999822 ) ) ;
#30841 = CIRCLE ( 'NONE', #15872, 2.000000000000001776 ) ;
#30842 = DIRECTION ( 'NONE',  ( 0.000000000000000000, 0.000000000000000000, 1.000000000000000000 ) ) ;
#30843 = CARTESIAN_POINT ( 'NONE',  ( 5.253368672218635460, -3.033033817057790404, -4.359491423763655504 ) ) ;
#30844 = CARTESIAN_POINT ( 'NONE',  ( 6.249999999999998224, 0.000000000000000000, 3.000000000000000888 ) ) ;
#30845 = PRESENTATION_LAYER_ASSIGNMENT (  '', '', ( #25451 ) ) ;
#30846 = ORIENTED_EDGE ( 'NONE', *, *, #20497, .T. ) ;
#30847 = EDGE_CURVE ( 'NONE', #17078, #37014, #4137, .T. ) ;
#30848 = ORIENTED_EDGE ( 'NONE', *, *, #29228, .T. ) ;
#30849 = FACE_OUTER_BOUND ( 'NONE', #1332, .T. ) ;
#30850 = CIRCLE ( 'NONE', #35660, 2.000000000000001776 ) ;
#30851 = DIRECTION ( 'NONE',  ( 1.000000000000000000, 0.000000000000000000, 0.000000000000000000 ) ) ;
#30852 = CIRCLE ( 'NONE', #18280, 2.000000000000001776 ) ;
#30853 = CIRCLE ( 'NONE', #936, 3.499999999999989342 ) ;
#30854 = CARTESIAN_POINT ( 'NONE',  ( -6.000000000000000000, 149.8799519615616305, 32.55002500000000509 ) ) ;
#30855 = VERTEX_POINT ( 'NONE', #12724 ) ;
#30856 = ORIENTED_EDGE ( 'NONE', *, *, #19242, .T. ) ;
#30857 = PRODUCT_RELATED_PRODUCT_CATEGORY ( 'part', '', ( #8866 ) ) ;
#30858 = DIRECTION ( 'NONE',  ( 0.000000000000000000, 0.000000000000000000, 1.000000000000000000 ) ) ;
#30859 = FACE_OUTER_BOUND ( 'NONE', #34148, .T. ) ;
#30860 = EDGE_CURVE ( 'NONE', #7478, #200, #10481, .T. ) ;
#30861 = DIRECTION ( 'NONE',  ( 1.000000000000000000, 0.000000000000000000, 0.000000000000000000 ) ) ;
#30862 = ORIENTED_EDGE ( 'NONE', *, *, #19213, .F. ) ;
#30863 = ORIENTED_EDGE ( 'NONE', *, *, #30250, .T. ) ;
#30864 = LINE ( 'NONE', #33882, #27265 ) ;
#30865 = EDGE_CURVE ( 'NONE', #27665, #14128, #4696, .T. ) ;
#30866 = CIRCLE ( 'NONE', #36876, 33.00000000000001421 ) ;
#30867 = DIRECTION ( 'NONE',  ( 0.000000000000000000, 0.000000000000000000, 1.000000000000000000 ) ) ;
#30868 = EDGE_LOOP ( 'NONE', ( #12801, #14275 ) ) ;
#30869 = CIRCLE ( 'NONE', #18295, 2.000000000000001776 ) ;
#30870 = CARTESIAN_POINT ( 'NONE',  ( -8.000003374631278419, -69.28203230275519786, 12.50000000000000000 ) ) ;
#30871 = VERTEX_POINT ( 'NONE', #35827 ) ;
#30872 = FACE_BOUND ( 'NONE', #28714, .T. ) ;
#30873 = AXIS2_PLACEMENT_3D ( 'NONE', #322, #4449, #9527 ) ;
#30874 = AXIS2_PLACEMENT_3D ( 'NONE', #388, #26080, #11822 ) ;
#30875 = CIRCLE ( 'NONE', #8721, 2.000000000000001776 ) ;
#30876 = AXIS2_PLACEMENT_3D ( 'NONE', #27869, #16831, #19444 ) ;
#30877 = CARTESIAN_POINT ( 'NONE',  ( -57.00000337463111322, -43.30127018922202353, -9.999999999999998224 ) ) ;
#30878 = CARTESIAN_POINT ( 'NONE',  ( 0.6806757771963801718, 5.380514348701075811, -3.838711833384166550 ) ) ;
#30879 = EDGE_LOOP ( 'NONE', ( #14, #32234 ) ) ;
#30880 = DIRECTION ( 'NONE',  ( -0.4999999999999919509, 0.8660254037844432595, 0.000000000000000000 ) ) ;
#30881 = VECTOR ( 'NONE', #37081, 1000.000000000000000 ) ;
#30882 = FACE_OUTER_BOUND ( 'NONE', #14172, .T. ) ;
#30883 = EDGE_CURVE ( 'NONE', #8438, #23785, #13293, .T. ) ;
#30884 = CYLINDRICAL_SURFACE ( 'NONE', #22156, 2.000000000000001776 ) ;
#30885 = CYLINDRICAL_SURFACE ( 'NONE', #3548, 2.000000000000001776 ) ;
#30886 = VERTEX_POINT ( 'NONE', #21735 ) ;
#30887 = DIRECTION ( 'NONE',  ( -0.000000000000000000, -0.000000000000000000, 1.000000000000000000 ) ) ;
#30888 = LINE ( 'NONE', #19291, #19063 ) ;
#30889 = CARTESIAN_POINT ( 'NONE',  ( -3.346878500200759277, -3.841181488860386573, -5.948595712916170619 ) ) ;
#30890 = CIRCLE ( 'NONE', #8738, 2.000000000000001776 ) ;
#30891 = EDGE_CURVE ( 'NONE', #28371, #30600, #2334, .T. ) ;
#30892 = ORIENTED_EDGE ( 'NONE', *, *, #26308, .T. ) ;
#30893 = ORIENTED_EDGE ( 'NONE', *, *, #26331, .T. ) ;
#30894 = VECTOR ( 'NONE', #15779, 1000.000000000000000 ) ;
#30895 = ADVANCED_FACE ( 'NONE', ( #1689 ), #21371, .F. ) ;
#30896 = CYLINDRICAL_SURFACE ( 'NONE', #9619, 2.000000000000001776 ) ;
#30897 = ORIENTED_EDGE ( 'NONE', *, *, #35013, .T. ) ;
#30898 =( GEOMETRIC_REPRESENTATION_CONTEXT ( 3 ) GLOBAL_UNCERTAINTY_ASSIGNED_CONTEXT ( ( #30178 ) ) GLOBAL_UNIT_ASSIGNED_CONTEXT ( ( #18348, #18153, #3902 ) ) REPRESENTATION_CONTEXT ( 'NONE', 'WORKASPACE' ) );
#30899 = DIRECTION ( 'NONE',  ( 0.000000000000000000, 0.000000000000000000, -1.000000000000000000 ) ) ;
#30900 = DIRECTION ( 'NONE',  ( 1.000000000000000000, 0.000000000000000000, 0.000000000000000000 ) ) ;
#30901 = AXIS2_PLACEMENT_3D ( 'NONE', #33181, #18948, #10498 ) ;
#30902 = VECTOR ( 'NONE', #17568, 1000.000000000000000 ) ;
#30903 = AXIS2_PLACEMENT_3D ( 'NONE', #18478, #36090, #6832 ) ;
#30904 = DIRECTION ( 'NONE',  ( 0.000000000000000000, 0.000000000000000000, -1.000000000000000000 ) ) ;
#30905 = AXIS2_PLACEMENT_3D ( 'NONE', #11942, #29190, #23399 ) ;
#30906 = CARTESIAN_POINT ( 'NONE',  ( -5.253368672218638125, -3.033033817057809500, -4.359491423763659945 ) ) ;
#30907 = CARTESIAN_POINT ( 'NONE',  ( 33.99999999999999289, 103.4105893997321743, -19.99999999999999645 ) ) ;
#30908 = CARTESIAN_POINT ( 'NONE',  ( -93.06171781654443009, -70.18599611865349175, 32.50000000000000000 ) ) ;
#30909 = DIRECTION ( 'NONE',  ( 0.000000000000000000, 0.000000000000000000, 1.000000000000000000 ) ) ;
#30910 = DIRECTION ( 'NONE',  ( 0.000000000000000000, 0.000000000000000000, 1.000000000000000000 ) ) ;
#30911 = ORIENTED_EDGE ( 'NONE', *, *, #21914, .F. ) ;
#30912 = ORIENTED_EDGE ( 'NONE', *, *, #22187, .T. ) ;
#30913 = FACE_OUTER_BOUND ( 'NONE', #20488, .T. ) ;
#30914 = ADVANCED_FACE ( 'NONE', ( #4494 ), #34669, .T. ) ;
#30915 = CARTESIAN_POINT ( 'NONE',  ( 11.99999662536865763, -69.28203230275519786, -5.000000000000000000 ) ) ;
#30916 = CARTESIAN_POINT ( 'NONE',  ( 72.28378166042060116, 61.53067111003190348, -49.22241343995293761 ) ) ;
#30917 = DIRECTION ( 'NONE',  ( 1.000000000000000000, 0.000000000000000000, 0.000000000000000000 ) ) ;
#30918 = ORIENTED_EDGE ( 'NONE', *, *, #17858, .F. ) ;
#30919 = PRODUCT_DEFINITION_CONTEXT ( 'detailed design', #30999, 'design' ) ;
#30920 = AXIS2_PLACEMENT_3D ( 'NONE', #25372, #36804, #11107 ) ;
#30921 = AXIS2_PLACEMENT_3D ( 'NONE', #3921, #7484, #18741 ) ;
#30922 = CARTESIAN_POINT ( 'NONE',  ( 4.999999999999999112, -2.691295138309024892, -1.881393335304215153 ) ) ;
#30923 = VERTEX_POINT ( 'NONE', #30560 ) ;
#30924 = EDGE_LOOP ( 'NONE', ( #11594, #32519 ) ) ;
#30925 = AXIS2_PLACEMENT_3D ( 'NONE', #11551, #13834, #11006 ) ;
#30926 = CARTESIAN_POINT ( 'NONE',  ( 56.99999662536844625, 60.62177826491077326, -9.999999999999998224 ) ) ;
#30927 = ORIENTED_EDGE ( 'NONE', *, *, #19394, .F. ) ;
#30928 = AXIS2_PLACEMENT_3D ( 'NONE', #30482, #35562, #4055 ) ;
#30929 = LINE ( 'NONE', #33588, #14794 ) ;
#30930 = DIRECTION ( 'NONE',  ( -1.000000000000000000, -0.000000000000000000, -0.000000000000000000 ) ) ;
#30931 = VECTOR ( 'NONE', #32181, 1000.000000000000000 ) ;
#30932 = EDGE_CURVE ( 'NONE', #34151, #29420, #28070, .T. ) ;
#30933 = DIRECTION ( 'NONE',  ( 0.000000000000000000, 0.000000000000000000, 1.000000000000000000 ) ) ;
#30934 = VERTEX_POINT ( 'NONE', #26996 ) ;
#30935 = EDGE_CURVE ( 'NONE', #1224, #1952, #41, .T. ) ;
#30936 = ORIENTED_EDGE ( 'NONE', *, *, #28901, .F. ) ;
#30937 = ORIENTED_EDGE ( 'NONE', *, *, #34852, .T. ) ;
#30938 = TOROIDAL_SURFACE ( 'NONE', #18403, 3.250000000000001332, 0.2500000000000000000 ) ;
#30939 = ADVANCED_FACE ( 'NONE', ( #14409 ), #19850, .F. ) ;
#30940 = ORIENTED_EDGE ( 'NONE', *, *, #15517, .F. ) ;
#30941 = ORIENTED_EDGE ( 'NONE', *, *, #5939, .F. ) ;
#30942 = DIRECTION ( 'NONE',  ( 0.000000000000000000, 0.8660254037844379305, -0.5000000000000014433 ) ) ;
#30943 = DIRECTION ( 'NONE',  ( 0.000000000000000000, 0.000000000000000000, 1.000000000000000000 ) ) ;
#30944 = ADVANCED_FACE ( 'NONE', ( #13851 ), #33739, .F. ) ;
#30945 = CARTESIAN_POINT ( 'NONE',  ( 93.60231327712337190, 15.97563234535636134, 12.49999999999999822 ) ) ;
#30946 = CARTESIAN_POINT ( 'NONE',  ( -22.00000337463124112, 69.28203230275516944, -9.999999999999998224 ) ) ;
#30947 = CARTESIAN_POINT ( 'NONE',  ( -47.63139720814380951, 27.50000000000055422, -15.00000000000000000 ) ) ;
#30948 = EDGE_CURVE ( 'NONE', #6252, #530, #22852, .T. ) ;
#30949 = ORIENTED_EDGE ( 'NONE', *, *, #4806, .T. ) ;
#30950 = DIRECTION ( 'NONE',  ( -0.000000000000000000, -0.000000000000000000, 1.000000000000000000 ) ) ;
#30951 = VECTOR ( 'NONE', #12754, 999.9999999999998863 ) ;
#30952 = CARTESIAN_POINT ( 'NONE',  ( -20.00000337463123756, -69.28203230275522628, -9.999999999999998224 ) ) ;
#30953 = AXIS2_PLACEMENT_3D ( 'NONE', #18840, #30256, #3241 ) ;
#30954 = CLOSED_SHELL ( 'NONE', ( #14090, #27677, #18133, #24508, #33502, #4683, #27904, #30030, #17937, #2227, #5506, #28150, #7396, #21571, #20420, #25322, #24249, #3399, #8676, #6891, #36879, #2858, #7871, #20897, #8664, #13961, #3125, #16230, #29311, #34667, #10663, #4237, #27724, #18520, #22167, #24318, #28115, #4370, #36166 ) ) ;
#30955 = CARTESIAN_POINT ( 'NONE',  ( 0.000000000000000000, 0.000000000000000000, -5.974599999999999689 ) ) ;
#30956 = ORIENTED_EDGE ( 'NONE', *, *, #19168, .T. ) ;
#30957 = CARTESIAN_POINT ( 'NONE',  ( 2.999999999999768630, -68.00000000000000000, -49.86348611802629449 ) ) ;
#30958 = CARTESIAN_POINT ( 'NONE',  ( 27.78182860042856461, 56.67878100130339902, 12.49999999999999822 ) ) ;
#30959 = LINE ( 'NONE', #13337, #15355 ) ;
#30960 = EDGE_CURVE ( 'NONE', #1861, #3252, #24472, .T. ) ;
#30961 = PRESENTATION_LAYER_ASSIGNMENT (  '', '', ( #413 ) ) ;
#30962 = VERTEX_POINT ( 'NONE', #5242 ) ;
#30963 = VECTOR ( 'NONE', #15745, 1000.000000000000000 ) ;
#30964 = ADVANCED_FACE ( 'NONE', ( #30721 ), #27914, .F. ) ;
#30965 = ORIENTED_EDGE ( 'NONE', *, *, #2557, .T. ) ;
#30966 = CIRCLE ( 'NONE', #18396, 2.000000000000000000 ) ;
#30967 = CARTESIAN_POINT ( 'NONE',  ( 42.97377950131527058, 96.90768712682506703, 27.49999999999999645 ) ) ;
#30968 = EDGE_CURVE ( 'NONE', #22847, #12612, #33464, .T. ) ;
#30969 = EDGE_CURVE ( 'NONE', #34463, #30062, #2793, .T. ) ;
#30970 = DIRECTION ( 'NONE',  ( 1.000000000000000000, 0.000000000000000000, 0.000000000000000000 ) ) ;
#30971 = CARTESIAN_POINT ( 'NONE',  ( 5.284804376168104056, -3.015249596956828704, -4.366192694417983411 ) ) ;
#30972 = EDGE_CURVE ( 'NONE', #14875, #34980, #27458, .T. ) ;
#30973 = DIRECTION ( 'NONE',  ( 1.000000000000000000, 0.000000000000000000, 0.000000000000000000 ) ) ;
#30974 = VERTEX_POINT ( 'NONE', #22467 ) ;
#30975 = ORIENTED_EDGE ( 'NONE', *, *, #25742, .F. ) ;
#30976 = AXIS2_PLACEMENT_3D ( 'NONE', #29188, #7070, #13243 ) ;
#30977 = VECTOR ( 'NONE', #13314, 1000.000000000000000 ) ;
#30978 = DIRECTION ( 'NONE',  ( 0.000000000000000000, 0.000000000000000000, 1.000000000000000000 ) ) ;
#30979 = ORIENTED_EDGE ( 'NONE', *, *, #22949, .T. ) ;
#30980 = AXIS2_PLACEMENT_3D ( 'NONE', #33457, #16212, #11110 ) ;
#30981 = DIRECTION ( 'NONE',  ( 0.000000000000000000, 0.000000000000000000, -1.000000000000000000 ) ) ;
#30982 = ORIENTED_EDGE ( 'NONE', *, *, #30146, .T. ) ;
#30983 = AXIS2_PLACEMENT_3D ( 'NONE', #29980, #4298, #15729 ) ;
#30984 = CARTESIAN_POINT ( 'NONE',  ( -25.00000337463120914, 77.94228634059957983, 12.50000000000000000 ) ) ;
#30985 = B_SPLINE_CURVE_WITH_KNOTS ( 'NONE', 3,
 ( #21099, #27273, #9494, #24106, #9841, #9674 ),
 .UNSPECIFIED., .F., .F.,
 ( 4, 2, 4 ),
 ( 0.008070708573309213693, 0.009531758523483287518, 0.01099280847365736134 ),
 .UNSPECIFIED. ) ;
#30986 = CARTESIAN_POINT ( 'NONE',  ( -80.00000337463094979, 34.64101615137757051, -9.999999999999998224 ) ) ;
#30987 = DIRECTION ( 'NONE',  ( 0.000000000000000000, 0.000000000000000000, 1.000000000000000000 ) ) ;
#30988 = ORIENTED_EDGE ( 'NONE', *, *, #32082, .F. ) ;
#30989 = EDGE_LOOP ( 'NONE', ( #6048, #15262, #19705 ) ) ;
#30990 = LINE ( 'NONE', #26791, #2358 ) ;
#30991 = LINE ( 'NONE', #33805, #21350 ) ;
#30992 = STYLED_ITEM ( 'NONE', ( #20580 ), #4968 ) ;
#30993 = VECTOR ( 'NONE', #30563, 1000.000000000000000 ) ;
#30994 = CYLINDRICAL_SURFACE ( 'NONE', #3709, 2.000000000000001776 ) ;
#30995 = CARTESIAN_POINT ( 'NONE',  ( 34.99999662536853862, 77.94228634059959404, 12.50000000000000000 ) ) ;
#30996 = CIRCLE ( 'NONE', #8253, 27.00000000000001421 ) ;
#30997 = ORIENTED_EDGE ( 'NONE', *, *, #35127, .F. ) ;
#30998 = DIRECTION ( 'NONE',  ( 1.000000000000000000, 0.000000000000000000, 0.000000000000000000 ) ) ;
#30999 = APPLICATION_CONTEXT ( 'automotive_design' ) ;
#31000 = FACE_BOUND ( 'NONE', #9393, .T. ) ;
#31001 = CARTESIAN_POINT ( 'NONE',  ( -60.00000337463108480, -51.96152422706641971, -5.000000000000000000 ) ) ;
#31002 = CARTESIAN_POINT ( 'NONE',  ( 61.53067111003264955, -72.28378166041994746, 12.49999999999999822 ) ) ;
#31003 = CIRCLE ( 'NONE', #13659, 2.000000000000001776 ) ;
#31004 = CARTESIAN_POINT ( 'NONE',  ( 79.99999662536833966, -3.469446951953614189E-15, -5.000000000000000000 ) ) ;
#31005 = DIRECTION ( 'NONE',  ( 0.000000000000000000, 0.000000000000000000, 1.000000000000000000 ) ) ;
#31006 = DIRECTION ( 'NONE',  ( 0.000000000000000000, 0.000000000000000000, 1.000000000000000000 ) ) ;
#31007 = AXIS2_PLACEMENT_3D ( 'NONE', #15704, #7087, #13258 ) ;
#31008 = CARTESIAN_POINT ( 'NONE',  ( 41.99999662536853151, 69.28203230275518365, 17.49999999999999645 ) ) ;
#31009 = ORIENTED_EDGE ( 'NONE', *, *, #36027, .F. ) ;
#31010 = CIRCLE ( 'NONE', #35819, 2.000000000000001776 ) ;
#31011 = AXIS2_PLACEMENT_3D ( 'NONE', #1338, #21031, #27024 ) ;
#31012 = CARTESIAN_POINT ( 'NONE',  ( 2.778182860042552438, -69.13212189986967360, -4.999999999999997335 ) ) ;
#31013 = FACE_OUTER_BOUND ( 'NONE', #2067, .T. ) ;
#31014 = VECTOR ( 'NONE', #18309, 1000.000000000000000 ) ;
#31015 = ORIENTED_EDGE ( 'NONE', *, *, #12109, .T. ) ;
#31016 = ADVANCED_FACE ( 'NONE', ( #28108 ), #15497, .F. ) ;
#31017 = ORIENTED_EDGE ( 'NONE', *, *, #5133, .F. ) ;
#31018 = ORIENTED_EDGE ( 'NONE', *, *, #10772, .T. ) ;
#31019 = AXIS2_PLACEMENT_3D ( 'NONE', #14118, #28195, #11494 ) ;
#31020 = EDGE_CURVE ( 'NONE', #12923, #14280, #29859, .T. ) ;
#31021 = CARTESIAN_POINT ( 'NONE',  ( -85.00000337463092137, 25.98076211353317433, -9.999999999999998224 ) ) ;
#31022 = DIRECTION ( 'NONE',  ( 0.000000000000000000, 0.000000000000000000, 1.000000000000000000 ) ) ;
#31023 = ORIENTED_EDGE ( 'NONE', *, *, #3957, .F. ) ;
#31024 = AXIS2_PLACEMENT_3D ( 'NONE', #17412, #30910, #31275 ) ;
#31025 = DIRECTION ( 'NONE',  ( 0.000000000000000000, 0.000000000000000000, -1.000000000000000000 ) ) ;
#31026 = ORIENTED_EDGE ( 'NONE', *, *, #6316, .T. ) ;
#31027 = CARTESIAN_POINT ( 'NONE',  ( 19.04456692557281983, -111.2113061358873836, 32.49999999999999289 ) ) ;
#31028 = EDGE_LOOP ( 'NONE', ( #30162, #21502, #35720, #35499 ) ) ;
#31029 = LINE ( 'NONE', #25054, #365 ) ;
#31030 = CIRCLE ( 'NONE', #26853, 2.000000000000001776 ) ;
#31031 = VERTEX_POINT ( 'NONE', #11953 ) ;
#31032 = LINE ( 'NONE', #25056, #31567 ) ;
#31033 = CARTESIAN_POINT ( 'NONE',  ( 59.99999662536843914, -34.64101615137759893, -9.999999999999998224 ) ) ;
#31034 = CIRCLE ( 'NONE', #29225, 2.000000000000000000 ) ;
#31035 = ORIENTED_EDGE ( 'NONE', *, *, #28554, .T. ) ;
#31036 = DIRECTION ( 'NONE',  ( 0.000000000000000000, 0.000000000000000000, 1.000000000000000000 ) ) ;
#31037 = AXIS2_PLACEMENT_3D ( 'NONE', #25877, #174, #23056 ) ;
#31038 = CONTEXT_DEPENDENT_SHAPE_REPRESENTATION ( #18789, #15486 ) ;
#31039 = EDGE_CURVE ( 'NONE', #12699, #23292, #13700, .T. ) ;
#31040 = FACE_OUTER_BOUND ( 'NONE', #2304, .T. ) ;
#31041 = DIRECTION ( 'NONE',  ( -0.000000000000000000, -0.000000000000000000, 1.000000000000000000 ) ) ;
#31042 = VERTEX_POINT ( 'NONE', #26569 ) ;
#31043 = DIRECTION ( 'NONE',  ( 0.5000000000000038858, 0.8660254037844362651, 0.000000000000000000 ) ) ;
#31044 = CARTESIAN_POINT ( 'NONE',  ( -65.00000337463102085, 43.30127018922198801, 12.50000000000000000 ) ) ;
#31045 = ORIENTED_EDGE ( 'NONE', *, *, #21119, .T. ) ;
#31046 = DIRECTION ( 'NONE',  ( -1.156482317317870344E-14, -1.000000000000000000, 0.000000000000000000 ) ) ;
#31047 = DIRECTION ( 'NONE',  ( 0.000000000000000000, 0.000000000000000000, 1.000000000000000000 ) ) ;
#31048 = DIRECTION ( 'NONE',  ( 0.000000000000000000, -0.000000000000000000, -1.000000000000000000 ) ) ;
#31049 = CIRCLE ( 'NONE', #14882, 33.00000000000001421 ) ;
#31050 = PLANE ( 'NONE',  #11670 ) ;
#31051 =( BOUNDED_SURFACE ( )  B_SPLINE_SURFACE ( 3, 2, ( 
 ( #30696, #33710, #36153 ),
 ( #16454, #5211, #22272 ),
 ( #10455, #17348, #3094 ),
 ( #21898, #19455, #24548 ),
 ( #30878, #7461, #33343 ),
 ( #16651, #28583, #35984 ) ),
 .UNSPECIFIED., .F., .F., .F. ) 
 B_SPLINE_SURFACE_WITH_KNOTS ( ( 4, 2, 4 ),
 ( 3, 3 ),
 ( 0.002450104044831664246, 0.005591829551853650000, 0.008733555058875635754 ),
 ( 0.000000000000000000, 1.000000000000000000 ),
 .UNSPECIFIED. ) 
 GEOMETRIC_REPRESENTATION_ITEM ( )  RATIONAL_B_SPLINE_SURFACE ( (
 ( 1.000000000000000000, 0.8047731410850403888, 1.000000000000000000),
 ( 1.000000000000000000, 0.8125552299154461533, 1.000000000000000000),
 ( 1.000000000000000000, 0.8191520442892223919, 1.000000000000000000),
 ( 1.000000000000000000, 0.8191520442887518794, 1.000000000000000000),
 ( 1.000000000000000000, 0.8125552299157995373, 1.000000000000000000),
 ( 1.000000000000000000, 0.8047731410850398337, 1.000000000000000000) ) ) 
 REPRESENTATION_ITEM ( '' )  SURFACE ( )  );
#31052 = EDGE_CURVE ( 'NONE', #16962, #14513, #19100, .T. ) ;
#31053 = CIRCLE ( 'NONE', #2311, 2.000000000000001776 ) ;
#31054 = VERTEX_POINT ( 'NONE', #3330 ) ;
#31055 = ORIENTED_EDGE ( 'NONE', *, *, #1833, .T. ) ;
#31056 = LINE ( 'NONE', #25081, #1013 ) ;
#31057 = CIRCLE ( 'NONE', #7106, 2.000000000000001776 ) ;
#31058 = DIRECTION ( 'NONE',  ( -1.000000000000000000, 0.000000000000000000, 0.000000000000000000 ) ) ;
#31059 = VERTEX_POINT ( 'NONE', #11760 ) ;
#31060 = EDGE_LOOP ( 'NONE', ( #36705, #8393 ) ) ;
#31061 = CIRCLE ( 'NONE', #30447, 65.00000000000000000 ) ;
#31062 = EDGE_CURVE ( 'NONE', #148, #17870, #34056, .T. ) ;
#31063 = CARTESIAN_POINT ( 'NONE',  ( 4.999996625368645198, 77.94228634059957983, -5.000000000000000000 ) ) ;
#31064 = CARTESIAN_POINT ( 'NONE',  ( -62.00000337463104927, 34.64101615137757051, -9.999999999999998224 ) ) ;
#31065 = AXIS2_PLACEMENT_3D ( 'NONE', #37085, #25829, #6121 ) ;
#31066 = DIRECTION ( 'NONE',  ( 1.000000000000000000, 0.000000000000000000, 0.000000000000000000 ) ) ;
#31067 = EDGE_LOOP ( 'NONE', ( #19843, #12866, #19862, #24940 ) ) ;
#31068 = ORIENTED_EDGE ( 'NONE', *, *, #5759, .F. ) ;
#31069 = CYLINDRICAL_SURFACE ( 'NONE', #26090, 2.000000000000001776 ) ;
#31070 = CARTESIAN_POINT ( 'NONE',  ( -17.00000337463125533, -77.94228634059960825, 12.50000000000000000 ) ) ;
#31071 = ORIENTED_EDGE ( 'NONE', *, *, #12409, .T. ) ;
#31072 = AXIS2_PLACEMENT_3D ( 'NONE', #31908, #6075, #34390 ) ;
#31073 = CARTESIAN_POINT ( 'NONE',  ( -8.000003374631249997, -86.60254037844400443, 17.49999999999999645 ) ) ;
#31074 = ORIENTED_EDGE ( 'NONE', *, *, #6827, .F. ) ;
#31075 = DIRECTION ( 'NONE',  ( -1.000000000000000000, 0.000000000000000000, -0.000000000000000000 ) ) ;
#31076 = VECTOR ( 'NONE', #22135, 1000.000000000000000 ) ;
#31077 = AXIS2_PLACEMENT_3D ( 'NONE', #26781, #1097, #12521 ) ;
#31078 = DIRECTION ( 'NONE',  ( 0.000000000000000000, 0.000000000000000000, 1.000000000000000000 ) ) ;
#31079 = EDGE_CURVE ( 'NONE', #8482, #10470, #23281, .T. ) ;
#31080 = EDGE_LOOP ( 'NONE', ( #8003, #33753, #18642, #26685 ) ) ;
#31081 = EDGE_CURVE ( 'NONE', #2089, #4841, #1713, .T. ) ;
#31082 = CARTESIAN_POINT ( 'NONE',  ( -70.80619744049063513, -84.18124734178185520, -26.00000000000000000 ) ) ;
#31083 = CARTESIAN_POINT ( 'NONE',  ( 93.60231327712337190, 15.97563234535636134, -49.86561046011506448 ) ) ;
#31084 = AXIS2_PLACEMENT_3D ( 'NONE', #8761, #22838, #25835 ) ;
#31085 = DIRECTION ( 'NONE',  ( 1.000000000000000000, 0.000000000000000000, 0.000000000000000000 ) ) ;
#31086 = CARTESIAN_POINT ( 'NONE',  ( -75.00000337463097821, 25.98076211353318854, 12.50000000000000000 ) ) ;
#31087 = EDGE_LOOP ( 'NONE', ( #26071, #13333, #9197, #34792, #12462, #5367, #26582, #19509, #18191, #2244, #32954, #33437, #839, #14508, #17843, #13957, #24486, #29164, #9616, #14588, #1784, #32230, #4210, #10291, #21110, #5619, #3, #24152, #12648 ) ) ;
#31088 = CARTESIAN_POINT ( 'NONE',  ( 9.999996625368618552, 69.28203230275516944, 17.49999999999999645 ) ) ;
#31089 = EDGE_CURVE ( 'NONE', #15962, #32853, #321, .T. ) ;
#31090 = AXIS2_PLACEMENT_3D ( 'NONE', #19205, #8320, #19917 ) ;
#31091 = LINE ( 'NONE', #5225, #5248 ) ;
#31092 = CARTESIAN_POINT ( 'NONE',  ( -2.500000000000003997, -4.330127018922192761, -6.000000000000000000 ) ) ;
#31093 = ORIENTED_EDGE ( 'NONE', *, *, #13693, .T. ) ;
#31094 = EDGE_CURVE ( 'NONE', #35130, #5261, #23577, .T. ) ;
#31095 = ORIENTED_EDGE ( 'NONE', *, *, #9858, .T. ) ;
#31096 = AXIS2_PLACEMENT_3D ( 'NONE', #10233, #10045, #21280 ) ;
#31097 = VERTEX_POINT ( 'NONE', #885 ) ;
#31098 = CYLINDRICAL_SURFACE ( 'NONE', #15151, 2.000000000000001776 ) ;
#31099 = LINE ( 'NONE', #16474, #36930 ) ;
#31100 = VECTOR ( 'NONE', #34089, 1000.000000000000000 ) ;
#31101 = CYLINDRICAL_SURFACE ( 'NONE', #9019, 2.000000000000000000 ) ;
#31102 = CIRCLE ( 'NONE', #32928, 2.000000000000001776 ) ;
#31103 = DIRECTION ( 'NONE',  ( 0.000000000000000000, -0.000000000000000000, -1.000000000000000000 ) ) ;
#31104 = EDGE_CURVE ( 'NONE', #33241, #27057, #6815, .T. ) ;
#31105 = AXIS2_PLACEMENT_3D ( 'NONE', #36640, #33819, #34022 ) ;
#31106 = DIRECTION ( 'NONE',  ( -1.000000000000000000, 0.000000000000000000, 0.000000000000000000 ) ) ;
#31107 = CARTESIAN_POINT ( 'NONE',  ( 52.39915983220795681, 35.19434990244919703, 12.49999999999999822 ) ) ;
#31108 = CARTESIAN_POINT ( 'NONE',  ( -85.00000337463092137, 8.660254037844389075, -9.999999999999998224 ) ) ;
#31109 = CARTESIAN_POINT ( 'NONE',  ( 3.000000000000000000, 0.000000000000000000, 0.000000000000000000 ) ) ;
#31110 = ORIENTED_EDGE ( 'NONE', *, *, #26125, .T. ) ;
#31111 = ORIENTED_EDGE ( 'NONE', *, *, #33594, .F. ) ;
#31112 = CARTESIAN_POINT ( 'NONE',  ( -62.00000337463107769, -34.64101615137762025, 12.50000000000000000 ) ) ;
#31113 = AXIS2_PLACEMENT_3D ( 'NONE', #35210, #18116, #9693 ) ;
#31114 = DIRECTION ( 'NONE',  ( -0.5000000000000098810, -0.8660254037844328234, 0.000000000000000000 ) ) ;
#31115 = FACE_OUTER_BOUND ( 'NONE', #15559, .T. ) ;
#31116 = DIRECTION ( 'NONE',  ( -0.000000000000000000, -0.000000000000000000, -1.000000000000000000 ) ) ;
#31117 = VERTEX_POINT ( 'NONE', #23775 ) ;
#31118 = AXIS2_PLACEMENT_3D ( 'NONE', #5577, #17210, #8760 ) ;
#31119 = EDGE_CURVE ( 'NONE', #25823, #22212, #223, .T. ) ;
#31120 = DIRECTION ( 'NONE',  ( 0.000000000000000000, 0.000000000000000000, 1.000000000000000000 ) ) ;
#31121 = EDGE_LOOP ( 'NONE', ( #20251, #19756, #2938, #9659, #11425 ) ) ;
#31122 = ORIENTED_EDGE ( 'NONE', *, *, #23499, .T. ) ;
#31123 = EDGE_CURVE ( 'NONE', #34040, #33, #4421, .T. ) ;
#31124 = DIRECTION ( 'NONE',  ( -0.000000000000000000, -0.000000000000000000, 1.000000000000000000 ) ) ;
#31125 = ORIENTED_EDGE ( 'NONE', *, *, #10394, .T. ) ;
#31126 = VECTOR ( 'NONE', #79, 1000.000000000000000 ) ;
#31127 = DIRECTION ( 'NONE',  ( -0.000000000000000000, -0.000000000000000000, -1.000000000000000000 ) ) ;
#31128 = CARTESIAN_POINT ( 'NONE',  ( -8.000003374631287301, 69.28203230275516944, -9.999999999999998224 ) ) ;
#31129 = AXIS2_PLACEMENT_3D ( 'NONE', #7143, #12363, #23632 ) ;
#31130 = DIRECTION ( 'NONE',  ( -0.000000000000000000, 0.000000000000000000, -1.000000000000000000 ) ) ;
#31131 = CIRCLE ( 'NONE', #8967, 33.00000000000001421 ) ;
#31132 = ORIENTED_EDGE ( 'NONE', *, *, #27726, .F. ) ;
#31133 = VERTEX_POINT ( 'NONE', #8778 ) ;
#31134 = EDGE_CURVE ( 'NONE', #4152, #36749, #1414, .T. ) ;
#31135 = AXIS2_PLACEMENT_3D ( 'NONE', #19335, #30756, #5077 ) ;
#31136 = EDGE_LOOP ( 'NONE', ( #26134, #3264 ) ) ;
#31137 = ORIENTED_EDGE ( 'NONE', *, *, #6821, .T. ) ;
#31138 = EDGE_CURVE ( 'NONE', #7314, #18680, #31925, .T. ) ;
#31139 = EDGE_LOOP ( 'NONE', ( #8472, #4299 ) ) ;
#31140 = DIRECTION ( 'NONE',  ( -1.000000000000000000, 0.000000000000000000, 0.000000000000000000 ) ) ;
#31141 = CIRCLE ( 'NONE', #8977, 45.00000000000000711 ) ;
#31142 = FACE_OUTER_BOUND ( 'NONE', #4791, .T. ) ;
#31143 = VECTOR ( 'NONE', #2170, 1000.000000000000000 ) ;
#31144 = DIRECTION ( 'NONE',  ( 1.000000000000000000, 0.000000000000000000, 0.000000000000000000 ) ) ;
#31145 = DIRECTION ( 'NONE',  ( 1.000000000000000000, 0.000000000000000000, 0.000000000000000000 ) ) ;
#31146 = CARTESIAN_POINT ( 'NONE',  ( 0.000000000000000000, 1.467624384280029615, 2.541999999999997151 ) ) ;
#31147 = VERTEX_POINT ( 'NONE', #6526 ) ;
#31148 = DIRECTION ( 'NONE',  ( 1.000000000000000000, 0.000000000000000000, 0.000000000000000000 ) ) ;
#31149 = LINE ( 'NONE', #5086, #20370 ) ;
#31150 = CARTESIAN_POINT ( 'NONE',  ( 19.99999662536861678, -86.60254037844400443, 17.49999999999999645 ) ) ;
#31151 = VERTEX_POINT ( 'NONE', #31647 ) ;
#31152 = VECTOR ( 'NONE', #20476, 1000.000000000000000 ) ;
#31153 = CARTESIAN_POINT ( 'NONE',  ( 0.000000000000000000, 98.60827697811544112, -19.99999999999999645 ) ) ;
#31154 = DIRECTION ( 'NONE',  ( 0.000000000000000000, 0.000000000000000000, 1.000000000000000000 ) ) ;
#31155 = AXIS2_PLACEMENT_3D ( 'NONE', #30378, #27740, #13488 ) ;
#31156 = VERTEX_POINT ( 'NONE', #20760 ) ;
#31157 = VERTEX_POINT ( 'NONE', #32194 ) ;
#31158 = ADVANCED_FACE ( 'NONE', ( #20561 ), #29389, .T. ) ;
#31159 = FACE_OUTER_BOUND ( 'NONE', #570, .T. ) ;
#31160 = CARTESIAN_POINT ( 'NONE',  ( -6.726859516510129033, 8.238026975208041383E-16, -4.599999999999999645 ) ) ;
#31161 = AXIS2_PLACEMENT_3D ( 'NONE', #5832, #11609, #9370 ) ;
#31162 = CARTESIAN_POINT ( 'NONE',  ( -5.000003374631269537, -77.94228634059960825, -5.000000000000000000 ) ) ;
#31163 = CARTESIAN_POINT ( 'NONE',  ( 89.27079897466126113, -32.49191361593859284, 12.49999999999999822 ) ) ;
#31164 = VERTEX_POINT ( 'NONE', #20959 ) ;
#31165 = ORIENTED_EDGE ( 'NONE', *, *, #4357, .T. ) ;
#31166 = CIRCLE ( 'NONE', #25773, 2.000000000000001776 ) ;
#31167 = ADVANCED_FACE ( 'NONE', ( #5979 ), #36752, .T. ) ;
#31168 = DIRECTION ( 'NONE',  ( -0.000000000000000000, -0.000000000000000000, 1.000000000000000000 ) ) ;
#31169 = VERTEX_POINT ( 'NONE', #525 ) ;
#31170 = EDGE_CURVE ( 'NONE', #21416, #16153, #19994, .T. ) ;
#31171 = EDGE_CURVE ( 'NONE', #36953, #29140, #30769, .T. ) ;
#31172 = DIRECTION ( 'NONE',  ( 0.000000000000000000, 0.000000000000000000, 1.000000000000000000 ) ) ;
#31173 = ORIENTED_EDGE ( 'NONE', *, *, #13306, .T. ) ;
#31174 = ORIENTED_EDGE ( 'NONE', *, *, #18774, .T. ) ;
#31175 = DIRECTION ( 'NONE',  ( 1.000000000000000000, 0.000000000000000000, 0.000000000000000000 ) ) ;
#31176 = CARTESIAN_POINT ( 'NONE',  ( 44.99999662536851019, -60.62177826491080168, -5.000000000000000000 ) ) ;
#31177 = PLANE ( 'NONE',  #37012 ) ;
#31178 = EDGE_LOOP ( 'NONE', ( #27654, #6628, #8538, #19209 ) ) ;
#31179 = EDGE_LOOP ( 'NONE', ( #15675, #20423, #9795, #29558, #19262 ) ) ;
#31180 = CARTESIAN_POINT ( 'NONE',  ( 62.97617850287784336, 4.279621169095339184, 12.49999999999999822 ) ) ;
#31181 = PLANE ( 'NONE',  #17160 ) ;
#31182 = CARTESIAN_POINT ( 'NONE',  ( -69.13212189986965939, -2.778182860042805125, 12.49999999999999645 ) ) ;
#31183 = CARTESIAN_POINT ( 'NONE',  ( -6.284666409917640040E-14, -6.000000000000000000, 32.50000000000000000 ) ) ;
#31184 = ADVANCED_FACE ( 'NONE', ( #27511 ), #12867, .T. ) ;
#31185 = EDGE_LOOP ( 'NONE', ( #19691, #31759, #7816, #15564, #10357 ) ) ;
#31186 = CARTESIAN_POINT ( 'NONE',  ( 62.97617850287784336, 4.279621169095339184, 12.49999999999999822 ) ) ;
#31187 = CIRCLE ( 'NONE', #32384, 2.000000000000001776 ) ;
#31188 = FACE_BOUND ( 'NONE', #3615, .T. ) ;
#31189 = DIRECTION ( 'NONE',  ( 1.000000000000000000, 0.000000000000000000, 0.000000000000000000 ) ) ;
#31190 = DIRECTION ( 'NONE',  ( 0.000000000000000000, 0.000000000000000000, -1.000000000000000000 ) ) ;
#31191 = DIRECTION ( 'NONE',  ( 0.000000000000000000, 0.000000000000000000, -1.000000000000000000 ) ) ;
#31192 = DIRECTION ( 'NONE',  ( 0.000000000000000000, -0.000000000000000000, -1.000000000000000000 ) ) ;
#31193 = CARTESIAN_POINT ( 'NONE',  ( 22.62085438525362591, 105.9441488773368860, 27.49998799999998411 ) ) ;
#31194 = LINE ( 'NONE', #5509, #19364 ) ;
#31195 = ORIENTED_EDGE ( 'NONE', *, *, #2139, .T. ) ;
#31196 = CARTESIAN_POINT ( 'NONE',  ( 46.99999662536849598, -77.94228634059960825, -9.999999999999998224 ) ) ;
#31197 = CARTESIAN_POINT ( 'NONE',  ( -42.97377950131527058, 96.90768712682508124, 18.49999999999999645 ) ) ;
#31198 = CYLINDRICAL_SURFACE ( 'NONE', #35960, 2.000000000000000000 ) ;
#31199 = EDGE_LOOP ( 'NONE', ( #4928, #35785, #11766, #28685 ) ) ;
#31200 = ORIENTED_EDGE ( 'NONE', *, *, #21249, .T. ) ;
#31201 = ADVANCED_FACE ( 'NONE', ( #24325 ), #4273, .T. ) ;
#31202 = ORIENTED_EDGE ( 'NONE', *, *, #19624, .T. ) ;
#31203 = DIRECTION ( 'NONE',  ( 1.000000000000000000, 0.000000000000000000, 0.000000000000000000 ) ) ;
#31204 = FACE_OUTER_BOUND ( 'NONE', #25702, .T. ) ;
#31205 = ADVANCED_FACE ( 'NONE', ( #16088 ), #24526, .F. ) ;
#31206 = ORIENTED_EDGE ( 'NONE', *, *, #34811, .F. ) ;
#31207 = CARTESIAN_POINT ( 'NONE',  ( 62.99999662536839651, -43.30127018922199511, -9.999999999999998224 ) ) ;
#31208 = ORIENTED_EDGE ( 'NONE', *, *, #34596, .F. ) ;
#31209 = CARTESIAN_POINT ( 'NONE',  ( -60.93295298010992411, -19.13981058454771755, 12.49999999999999822 ) ) ;
#31211 = ADVANCED_FACE ( 'NONE', ( #1828 ), #21132, .F. ) ;
#31210 = EDGE_LOOP ( 'NONE', ( #1159, #21640, #22918, #1672 ) ) ;
#31212 = CARTESIAN_POINT ( 'NONE',  ( 54.99999662536844625, 60.62177826491077326, -5.000000000000000000 ) ) ;
#31213 = ORIENTED_EDGE ( 'NONE', *, *, #10802, .F. ) ;
#31214 = CARTESIAN_POINT ( 'NONE',  ( -4.279621169095561228, 62.97617850287782915, 12.49999999999999822 ) ) ;
#31215 = CARTESIAN_POINT ( 'NONE',  ( -78.38502691089041718, -33.46124879229190441, -5.000000000000000000 ) ) ;
#31216 = ORIENTED_EDGE ( 'NONE', *, *, #268, .F. ) ;
#31217 = CARTESIAN_POINT ( 'NONE',  ( -62.00000337463107769, -34.64101615137762025, -9.999999999999998224 ) ) ;
#31218 = ADVANCED_FACE ( 'NONE', ( #29952 ), #35771, .F. ) ;
#31219 = LINE ( 'NONE', #22233, #35664 ) ;
#31220 = EDGE_CURVE ( 'NONE', #1450, #14564, #5028, .T. ) ;
#31221 = DIRECTION ( 'NONE',  ( -1.000000000000000000, 0.000000000000000000, 0.000000000000000000 ) ) ;
#31222 = EDGE_CURVE ( 'NONE', #19410, #10608, #15701, .T. ) ;
#31223 = VERTEX_POINT ( 'NONE', #18703 ) ;
#31224 = CYLINDRICAL_SURFACE ( 'NONE', #18946, 2.000000000000001776 ) ;
#31225 = CARTESIAN_POINT ( 'NONE',  ( 59.99999662536843914, -34.64101615137759893, 12.50000000000000000 ) ) ;
#31226 = EDGE_CURVE ( 'NONE', #36567, #21017, #10990, .T. ) ;
#31227 = ORIENTED_EDGE ( 'NONE', *, *, #28666, .F. ) ;
#31228 = DIRECTION ( 'NONE',  ( 0.000000000000000000, 0.000000000000000000, 1.000000000000000000 ) ) ;
#31229 = CIRCLE ( 'NONE', #25121, 2.000000000000001776 ) ;
#31230 = DIRECTION ( 'NONE',  ( 1.000000000000000000, 0.000000000000000000, 0.000000000000000000 ) ) ;
#31231 = CARTESIAN_POINT ( 'NONE',  ( 59.99999662536842493, 51.96152422706639129, -9.999999999999998224 ) ) ;
#31232 = FACE_OUTER_BOUND ( 'NONE', #1896, .T. ) ;
#31233 = VERTEX_POINT ( 'NONE', #18884 ) ;
#31234 = ORIENTED_EDGE ( 'NONE', *, *, #13683, .T. ) ;
#31235 = CARTESIAN_POINT ( 'NONE',  ( 0.4022569922705656609, -5.541259509125485039, -0.4198507760575983516 ) ) ;
#31236 = LINE ( 'NONE', #5552, #33144 ) ;
#31237 = EDGE_LOOP ( 'NONE', ( #18057, #22428 ) ) ;
#31238 = VERTEX_POINT ( 'NONE', #1637 ) ;
#31239 = DIRECTION ( 'NONE',  ( -0.000000000000000000, -0.000000000000000000, 1.000000000000000000 ) ) ;
#31240 = DIRECTION ( 'NONE',  ( 0.000000000000000000, 0.000000000000000000, -1.000000000000000000 ) ) ;
#31241 = DIRECTION ( 'NONE',  ( 0.000000000000000000, 0.000000000000000000, -1.000000000000000000 ) ) ;
#31242 = EDGE_CURVE ( 'NONE', #36088, #8851, #15791, .T. ) ;
#31243 = ORIENTED_EDGE ( 'NONE', *, *, #35938, .F. ) ;
#31244 = VERTEX_POINT ( 'NONE', #13069 ) ;
#31245 = DIRECTION ( 'NONE',  ( 0.000000000000000000, -0.000000000000000000, -1.000000000000000000 ) ) ;
#31246 = CIRCLE ( 'NONE', #35444, 2.000000000000001776 ) ;
#31247 = DIRECTION ( 'NONE',  ( -1.000000000000000000, 0.000000000000000000, 0.000000000000000000 ) ) ;
#31248 = VERTEX_POINT ( 'NONE', #4085 ) ;
#31249 = DIRECTION ( 'NONE',  ( 1.000000000000000000, 0.000000000000000000, 0.000000000000000000 ) ) ;
#31250 = ORIENTED_EDGE ( 'NONE', *, *, #22119, .F. ) ;
#31251 = FACE_OUTER_BOUND ( 'NONE', #14596, .T. ) ;
#31252 = CARTESIAN_POINT ( 'NONE',  ( 9.999996625368618552, 69.28203230275516944, -5.000000000000000000 ) ) ;
#31253 = ORIENTED_EDGE ( 'NONE', *, *, #21145, .F. ) ;
#31254 = DIRECTION ( 'NONE',  ( 0.000000000000000000, 0.000000000000000000, 1.000000000000000000 ) ) ;
#31255 = DIRECTION ( 'NONE',  ( 0.5000000000000039968, 0.8660254037844363761, 0.000000000000000000 ) ) ;
#31256 = CARTESIAN_POINT ( 'NONE',  ( 66.99999662536839651, -60.62177826491080168, 12.50000000000000000 ) ) ;
#31257 = FACE_OUTER_BOUND ( 'NONE', #4287, .T. ) ;
#31258 = EDGE_CURVE ( 'NONE', #603, #13910, #23573, .T. ) ;
#31259 = EDGE_LOOP ( 'NONE', ( #24079, #8962 ) ) ;
#31260 = DIRECTION ( 'NONE',  ( 0.000000000000000000, 0.000000000000000000, 1.000000000000000000 ) ) ;
#31261 = CARTESIAN_POINT ( 'NONE',  ( -45.00000337463111322, 77.94228634059959404, -5.000000000000000000 ) ) ;
#31262 = CARTESIAN_POINT ( 'NONE',  ( 81.99999662536832545, -17.32050807568879591, 12.50000000000000000 ) ) ;
#31263 = ORIENTED_EDGE ( 'NONE', *, *, #29961, .F. ) ;
#31264 = ORIENTED_EDGE ( 'NONE', *, *, #3313, .F. ) ;
#31265 = AXIS2_PLACEMENT_3D ( 'NONE', #5675, #11846, #22930 ) ;
#31266 = ORIENTED_EDGE ( 'NONE', *, *, #5273, .T. ) ;
#31267 = DIRECTION ( 'NONE',  ( 0.000000000000000000, 0.000000000000000000, -1.000000000000000000 ) ) ;
#31268 = CARTESIAN_POINT ( 'NONE',  ( -83.45172111230354517, 31.46585318596159553, -4.999999999999997335 ) ) ;
#31269 = DIRECTION ( 'NONE',  ( 0.000000000000000000, -0.000000000000000000, -1.000000000000000000 ) ) ;
#31270 = CARTESIAN_POINT ( 'NONE',  ( 32.49191361593954497, 89.27079897466093428, 12.49999999999999822 ) ) ;
#31271 = DIRECTION ( 'NONE',  ( 1.000000000000000000, 0.000000000000000000, 0.000000000000000000 ) ) ;
#31272 = CARTESIAN_POINT ( 'NONE',  ( -107.0107436789505329, -51.13647734612944618, 32.50000000000000711 ) ) ;
#31273 = CARTESIAN_POINT ( 'NONE',  ( 52.39915983220795681, 35.19434990244919703, -4.999999999999997335 ) ) ;
#31274 = EDGE_CURVE ( 'NONE', #3592, #281, #29553, .T. ) ;
#31275 = DIRECTION ( 'NONE',  ( 1.000000000000000000, 0.000000000000000000, 0.000000000000000000 ) ) ;
#31276 = EDGE_CURVE ( 'NONE', #8319, #32142, #2029, .T. ) ;
#31277 = ORIENTED_EDGE ( 'NONE', *, *, #18993, .T. ) ;
#31278 = VERTEX_POINT ( 'NONE', #4645 ) ;
#31279 = CIRCLE ( 'NONE', #1953, 2.000000000000001776 ) ;
#31280 = DIRECTION ( 'NONE',  ( 1.000000000000000000, 0.000000000000000000, 0.000000000000000000 ) ) ;
#31281 = LINE ( 'NONE', #28468, #30745 ) ;
#31282 = CARTESIAN_POINT ( 'NONE',  ( 0.000000000000000000, 89.94802294027097389, 32.49999999999990052 ) ) ;
#31283 = DIRECTION ( 'NONE',  ( 1.000000000000000000, 0.000000000000000000, 0.000000000000000000 ) ) ;
#31284 = ADVANCED_FACE ( 'NONE', ( #33321 ), #7639, .T. ) ;
#31285 = ORIENTED_EDGE ( 'NONE', *, *, #3882, .F. ) ;
#31286 = EDGE_CURVE ( 'NONE', #35776, #10733, #28966, .T. ) ;
#31287 = FACE_BOUND ( 'NONE', #22824, .T. ) ;
#31288 = ORIENTED_EDGE ( 'NONE', *, *, #18119, .T. ) ;
#31289 = CIRCLE ( 'NONE', #12704, 8.500000000000000000 ) ;
#31290 = ORIENTED_EDGE ( 'NONE', *, *, #28320, .F. ) ;
#31291 = AXIS2_PLACEMENT_3D ( 'NONE', #32347, #9831, #6663 ) ;
#31292 = DIRECTION ( 'NONE',  ( 0.000000000000000000, 0.000000000000000000, 1.000000000000000000 ) ) ;
#31293 = EDGE_LOOP ( 'NONE', ( #2778, #6108 ) ) ;
#31294 = SURFACE_STYLE_FILL_AREA ( #5266 ) ;
#31295 = CARTESIAN_POINT ( 'NONE',  ( 7.999996625368625658, 86.60254037844397601, 12.50000000000000000 ) ) ;
#31296 = PRODUCT_DEFINITION_SHAPE ( 'NONE', 'NONE',  #15978 ) ;
#31297 = DIRECTION ( 'NONE',  ( -0.000000000000000000, -0.8660254037844420383, -0.4999999999999941713 ) ) ;
#31298 = LINE ( 'NONE', #2819, #36453 ) ;
#31299 = ADVANCED_FACE ( 'NONE', ( #16634 ), #33693, .T. ) ;
#31300 = ORIENTED_EDGE ( 'NONE', *, *, #2094, .T. ) ;
#31301 = ORIENTED_EDGE ( 'NONE', *, *, #31527, .F. ) ;
#31302 = ORIENTED_EDGE ( 'NONE', *, *, #31123, .F. ) ;
#31303 = EDGE_LOOP ( 'NONE', ( #28970, #30326, #3796, #441, #35431, #22020, #34409, #6236 ) ) ;
#31304 = AXIS2_PLACEMENT_3D ( 'NONE', #35634, #1696, #1492 ) ;
#31305 = ORIENTED_EDGE ( 'NONE', *, *, #19330, .F. ) ;
#31306 = CARTESIAN_POINT ( 'NONE',  ( -59.13646009116099833, 70.47608876694653190, -4.999999999999997335 ) ) ;
#31307 =( NAMED_UNIT ( * ) PLANE_ANGLE_UNIT ( ) SI_UNIT ( $, .RADIAN. ) );
#31308 = CARTESIAN_POINT ( 'NONE',  ( 0.000000000000000000, 89.94802294027097389, -24.99999999999990763 ) ) ;
#31309 = CARTESIAN_POINT ( 'NONE',  ( 0.000000000000000000, 0.000000000000000000, 32.50000000000000000 ) ) ;
#31310 = DIRECTION ( 'NONE',  ( 1.000000000000000000, 0.000000000000000000, 0.000000000000000000 ) ) ;
#31311 = ORIENTED_EDGE ( 'NONE', *, *, #3137, .F. ) ;
#31312 = CARTESIAN_POINT ( 'NONE',  ( 46.00000000000000000, 103.4105893997321743, 27.49999999999999645 ) ) ;
#31313 = CARTESIAN_POINT ( 'NONE',  ( -4.817183509279844955, -3.279805190042336616, -4.266911319714225215 ) ) ;
#31314 = EDGE_CURVE ( 'NONE', #19087, #25741, #18794, .T. ) ;
#31315 = CARTESIAN_POINT ( 'NONE',  ( 83.67878100130371877, -27.78182860042797131, 12.49999999999999822 ) ) ;
#31316 = ORIENTED_EDGE ( 'NONE', *, *, #6873, .F. ) ;
#31317 = DIRECTION ( 'NONE',  ( 1.000000000000000000, 0.000000000000000000, 0.000000000000000000 ) ) ;
#31318 = CARTESIAN_POINT ( 'NONE',  ( -4.242640687119273224, -4.242640687119226151, 27.50000000000000000 ) ) ;
#31319 = ORIENTED_EDGE ( 'NONE', *, *, #3932, .F. ) ;
#31320 = ORIENTED_EDGE ( 'NONE', *, *, #13095, .F. ) ;
#31321 = CARTESIAN_POINT ( 'NONE',  ( -75.00000337463097821, 8.660254037844374864, -9.999999999999998224 ) ) ;
#31322 = CARTESIAN_POINT ( 'NONE',  ( -1.582370436568139027, 4.859920694385941431, -3.719399823475518119 ) ) ;
#31323 = DIRECTION ( 'NONE',  ( 0.000000000000000000, 0.000000000000000000, 1.000000000000000000 ) ) ;
#31324 = DIRECTION ( 'NONE',  ( -1.000000000000000000, 0.000000000000000000, -0.000000000000000000 ) ) ;
#31325 = EDGE_CURVE ( 'NONE', #10522, #29596, #28943, .T. ) ;
#31326 = ORIENTED_EDGE ( 'NONE', *, *, #18981, .F. ) ;
#31327 = EDGE_LOOP ( 'NONE', ( #30705, #10994, #2617, #13557 ) ) ;
#31328 = CIRCLE ( 'NONE', #33125, 2.000000000000001776 ) ;
#31329 = DIRECTION ( 'NONE',  ( 1.000000000000000000, 0.000000000000000000, 0.000000000000000000 ) ) ;
#31330 = CARTESIAN_POINT ( 'NONE',  ( 5.000000000000000888, 0.000000000000000000, -6.000000000000000000 ) ) ;
#31331 = EDGE_CURVE ( 'NONE', #20247, #16338, #7998, .T. ) ;
#31332 = ORIENTED_EDGE ( 'NONE', *, *, #18488, .F. ) ;
#31333 = FACE_BOUND ( 'NONE', #21474, .T. ) ;
#31334 = ORIENTED_EDGE ( 'NONE', *, *, #25903, .F. ) ;
#31335 = EDGE_LOOP ( 'NONE', ( #16337, #1117, #26946 ) ) ;
#31336 = CARTESIAN_POINT ( 'NONE',  ( -60.00000337463107059, -34.64101615137762025, -9.999999999999998224 ) ) ;
#31337 = CARTESIAN_POINT ( 'NONE',  ( -8.000003374631249997, -86.60254037844400443, -9.999999999999998224 ) ) ;
#31338 = AXIS2_PLACEMENT_3D ( 'NONE', #9048, #28362, #8870 ) ;
#31339 = DIRECTION ( 'NONE',  ( 0.000000000000000000, 0.000000000000000000, 1.000000000000000000 ) ) ;
#31340 = EDGE_LOOP ( 'NONE', ( #24197, #30382, #23894, #11167 ) ) ;
#31341 = ORIENTED_EDGE ( 'NONE', *, *, #9131, .F. ) ;
#31342 = PLANE ( 'NONE',  #28092 ) ;
#31343 = LINE ( 'NONE', #20099, #22560 ) ;
#31344 = FACE_OUTER_BOUND ( 'NONE', #2779, .T. ) ;
#31345 = CARTESIAN_POINT ( 'NONE',  ( 2.500000000000008438, 4.330127018922190096, -2.691222917490924395E-15 ) ) ;
#31346 = ADVANCED_FACE ( 'NONE', ( #5556 ), #36521, .F. ) ;
#31347 = ORIENTED_EDGE ( 'NONE', *, *, #3953, .F. ) ;
#31348 = CARTESIAN_POINT ( 'NONE',  ( 59.99999662536845335, 34.64101615137759893, -9.999999999999998224 ) ) ;
#31349 = FACE_BOUND ( 'NONE', #14308, .T. ) ;
#31350 = CARTESIAN_POINT ( 'NONE',  ( 54.99999662536844625, 60.62177826491077326, -9.999999999999998224 ) ) ;
#31351 = CARTESIAN_POINT ( 'NONE',  ( 0.000000000000000000, 0.000000000000000000, -5.000000000000000000 ) ) ;
#31352 = DIRECTION ( 'NONE',  ( -0.4999999999999980016, 0.8660254037844398178, 0.000000000000000000 ) ) ;
#31353 = DIRECTION ( 'NONE',  ( 0.000000000000000000, 0.000000000000000000, -1.000000000000000000 ) ) ;
#31354 = EDGE_CURVE ( 'NONE', #15333, #36697, #12171, .T. ) ;
#31355 = AXIS2_PLACEMENT_3D ( 'NONE', #20221, #14966, #29199 ) ;
#31356 = DIRECTION ( 'NONE',  ( 1.000000000000000000, 0.000000000000000000, 0.000000000000000000 ) ) ;
#31357 = ADVANCED_FACE ( 'NONE', ( #25634 ), #21780, .F. ) ;
#31358 = CARTESIAN_POINT ( 'NONE',  ( -52.00000337463112032, -51.96152422706641971, 12.50000000000000000 ) ) ;
#31359 = EDGE_LOOP ( 'NONE', ( #36822, #17601, #4707, #30193, #28019, #33184 ) ) ;
#31360 = CARTESIAN_POINT ( 'NONE',  ( -75.00000337463100664, -43.30127018922202353, 17.49999999999999645 ) ) ;
#31361 = DIRECTION ( 'NONE',  ( 0.000000000000000000, 0.000000000000000000, -1.000000000000000000 ) ) ;
#31362 = LINE ( 'NONE', #11121, #26971 ) ;
#31363 = CIRCLE ( 'NONE', #10389, 3.000000000000000000 ) ;
#31364 = ORIENTED_EDGE ( 'NONE', *, *, #34520, .F. ) ;
#31365 = ORIENTED_EDGE ( 'NONE', *, *, #3584, .T. ) ;
#31366 = EDGE_LOOP ( 'NONE', ( #33908, #32247 ) ) ;
#31367 = CIRCLE ( 'NONE', #34383, 2.000000000000001776 ) ;
#31368 = CARTESIAN_POINT ( 'NONE',  ( -51.13139720814437084, -27.49999999999955591, -5.000000000000000000 ) ) ;
#31369 = DIRECTION ( 'NONE',  ( 0.000000000000000000, 0.000000000000000000, 1.000000000000000000 ) ) ;
#31370 = CARTESIAN_POINT ( 'NONE',  ( -40.99999999999999289, 103.4105893997321743, 32.50000000000000000 ) ) ;
#31371 = EDGE_LOOP ( 'NONE', ( #33234, #32202 ) ) ;
#31372 = DIRECTION ( 'NONE',  ( 0.000000000000000000, 0.000000000000000000, 1.000000000000000000 ) ) ;
#31373 = EDGE_CURVE ( 'NONE', #22617, #1670, #821, .T. ) ;
#31374 = VERTEX_POINT ( 'NONE', #30680 ) ;
#31375 = DIRECTION ( 'NONE',  ( 0.000000000000000000, 0.000000000000000000, 1.000000000000000000 ) ) ;
#31376 = ORIENTED_EDGE ( 'NONE', *, *, #33121, .T. ) ;
#31377 = DIRECTION ( 'NONE',  ( 1.000000000000000000, 0.000000000000000000, 0.000000000000000000 ) ) ;
#31378 = ORIENTED_EDGE ( 'NONE', *, *, #35594, .F. ) ;
#31379 = EDGE_LOOP ( 'NONE', ( #34033, #1716 ) ) ;
#31380 = AXIS2_PLACEMENT_3D ( 'NONE', #24101, #10901, #27969 ) ;
#31381 = FACE_OUTER_BOUND ( 'NONE', #10745, .T. ) ;
#31382 = CARTESIAN_POINT ( 'NONE',  ( 74.99999662536836809, 8.660254037844394404, -9.999999999999998224 ) ) ;
#31383 = VERTEX_POINT ( 'NONE', #36869 ) ;
#31384 = DIRECTION ( 'NONE',  ( 0.000000000000000000, 0.000000000000000000, 1.000000000000000000 ) ) ;
#31385 = AXIS2_PLACEMENT_3D ( 'NONE', #19697, #16706, #27940 ) ;
#31386 = CARTESIAN_POINT ( 'NONE',  ( -72.00000337463102085, -51.96152422706641971, -5.000000000000000000 ) ) ;
#31387 = DIRECTION ( 'NONE',  ( 0.000000000000000000, 0.000000000000000000, -1.000000000000000000 ) ) ;
#31388 = EDGE_CURVE ( 'NONE', #393, #5725, #34370, .T. ) ;
#31389 = VERTEX_POINT ( 'NONE', #2561 ) ;
#31390 = CIRCLE ( 'NONE', #27809, 2.000000000000001776 ) ;
#31391 = DIRECTION ( 'NONE',  ( -0.000000000000000000, -0.000000000000000000, 1.000000000000000000 ) ) ;
#31392 = CARTESIAN_POINT ( 'NONE',  ( -61.53067111003215217, 72.28378166042038799, 12.49999999999999822 ) ) ;
#31393 = VERTEX_POINT ( 'NONE', #34257 ) ;
#31394 = EDGE_CURVE ( 'NONE', #14998, #11018, #19988, .T. ) ;
#31395 = DIRECTION ( 'NONE',  ( -1.047444401652940795E-14, -1.000000000000000000, 0.000000000000000000 ) ) ;
#31396 = DIRECTION ( 'NONE',  ( -1.000000000000000000, 0.000000000000000000, 0.000000000000000000 ) ) ;
#31397 = LINE ( 'NONE', #23162, #35129 ) ;
#31398 = FACE_OUTER_BOUND ( 'NONE', #13046, .T. ) ;
#31399 = EDGE_CURVE ( 'NONE', #4235, #6394, #18190, .T. ) ;
#31400 = ORIENTED_EDGE ( 'NONE', *, *, #12325, .T. ) ;
#31401 = CIRCLE ( 'NONE', #7542, 95.00000000000001421 ) ;
#31402 = ORIENTED_EDGE ( 'NONE', *, *, #28573, .T. ) ;
#31403 = VECTOR ( 'NONE', #22980, 1000.000000000000000 ) ;
#31404 = EDGE_CURVE ( 'NONE', #35276, #5559, #36325, .T. ) ;
#31405 = DIRECTION ( 'NONE',  ( 0.000000000000000000, 0.000000000000000000, 1.000000000000000000 ) ) ;
#31406 = DIRECTION ( 'NONE',  ( 1.000000000000000000, 0.000000000000000000, 0.000000000000000000 ) ) ;
#31407 = EDGE_CURVE ( 'NONE', #33059, #8160, #5819, .T. ) ;
#31408 = AXIS2_PLACEMENT_3D ( 'NONE', #15015, #6191, #35462 ) ;
#31409 = ORIENTED_EDGE ( 'NONE', *, *, #2564, .T. ) ;
#31410 = ORIENTED_EDGE ( 'NONE', *, *, #17199, .F. ) ;
#31411 = DIRECTION ( 'NONE',  ( 1.000000000000000000, 0.000000000000000000, 0.000000000000000000 ) ) ;
#31412 = DIRECTION ( 'NONE',  ( -1.000000000000000000, 0.000000000000000000, 0.000000000000000000 ) ) ;
#31413 = CARTESIAN_POINT ( 'NONE',  ( -50.00000337463112032, -51.96152422706641971, -9.999999999999998224 ) ) ;
#31414 = EDGE_CURVE ( 'NONE', #34083, #35809, #17017, .T. ) ;
#31415 = CIRCLE ( 'NONE', #16440, 2.000000000000000000 ) ;
#31416 = AXIS2_PLACEMENT_3D ( 'NONE', #14595, #4468, #9545 ) ;
#31418 = EDGE_LOOP ( 'NONE', ( #14786, #9948 ) ) ;
#31417 = EDGE_CURVE ( 'NONE', #13656, #12615, #6841, .T. ) ;
#31419 = VECTOR ( 'NONE', #20927, 1000.000000000000000 ) ;
#31420 = EDGE_CURVE ( 'NONE', #4355, #26422, #22256, .T. ) ;
#31421 = AXIS2_PLACEMENT_3D ( 'NONE', #91, #31041, #5719 ) ;
#31422 = CARTESIAN_POINT ( 'NONE',  ( 59.99999662536842493, 51.96152422706639129, 17.49999999999999645 ) ) ;
#31424 = EDGE_CURVE ( 'NONE', #29605, #6350, #28063, .T. ) ;
#31423 = ORIENTED_EDGE ( 'NONE', *, *, #17345, .T. ) ;
#31425 = EDGE_CURVE ( 'NONE', #29624, #29503, #5640, .T. ) ;
#31426 = DIRECTION ( 'NONE',  ( 0.000000000000000000, 0.000000000000000000, 1.000000000000000000 ) ) ;
#31427 = ORIENTED_EDGE ( 'NONE', *, *, #4989, .F. ) ;
#31428 = FACE_BOUND ( 'NONE', #4009, .T. ) ;
#31429 = CARTESIAN_POINT ( 'NONE',  ( 98.28784258493033121, 106.7731239591685437, 32.55002500000000509 ) ) ;
#31430 = CIRCLE ( 'NONE', #32606, 2.000000000000001776 ) ;
#31431 = CARTESIAN_POINT ( 'NONE',  ( 24.99999662536857059, 77.94228634059957983, 12.50000000000000000 ) ) ;
#31432 = CIRCLE ( 'NONE', #14676, 27.00000000000001421 ) ;
#31433 = ORIENTED_EDGE ( 'NONE', *, *, #30048, .F. ) ;
#31434 = DIRECTION ( 'NONE',  ( 0.000000000000000000, 0.000000000000000000, 1.000000000000000000 ) ) ;
#31435 = AXIS2_PLACEMENT_3D ( 'NONE', #24711, #5398, #13636 ) ;
#31436 = CIRCLE ( 'NONE', #9896, 2.000000000000001776 ) ;
#31437 = DIRECTION ( 'NONE',  ( 1.000000000000000000, 0.000000000000000000, 0.000000000000000000 ) ) ;
#31438 = LINE ( 'NONE', #28981, #7169 ) ;
#31439 = CARTESIAN_POINT ( 'NONE',  ( -30.00000337463118427, 69.28203230275516944, -5.000000000000000000 ) ) ;
#31440 = ORIENTED_EDGE ( 'NONE', *, *, #27656, .T. ) ;
#31441 = DIRECTION ( 'NONE',  ( 0.8660254037844347108, -0.5000000000000067724, 0.000000000000000000 ) ) ;
#31442 = CARTESIAN_POINT ( 'NONE',  ( 81.99999662536833966, -3.469446951953614189E-15, -9.999999999999998224 ) ) ;
#31443 = CARTESIAN_POINT ( 'NONE',  ( -53.00000337463106348, 43.30127018922197379, 17.49999999999999645 ) ) ;
#31444 = VECTOR ( 'NONE', #8759, 1000.000000000000000 ) ;
#31445 = EDGE_LOOP ( 'NONE', ( #27493, #15232, #5517, #33155 ) ) ;
#31446 = EDGE_LOOP ( 'NONE', ( #9384, #20804, #33399, #29439, #31562, #24082 ) ) ;
#31447 = ORIENTED_EDGE ( 'NONE', *, *, #10619, .T. ) ;
#31448 = CARTESIAN_POINT ( 'NONE',  ( 59.99999662536842493, -51.96152422706639840, 17.49999999999999645 ) ) ;
#31449 = CARTESIAN_POINT ( 'NONE',  ( -2.930059260563453005, -4.081832189068429706, -2.862547845245907365E-14 ) ) ;
#31450 = DIRECTION ( 'NONE',  ( 0.000000000000000000, 0.000000000000000000, 1.000000000000000000 ) ) ;
#31451 = DIRECTION ( 'NONE',  ( 0.000000000000000000, 0.000000000000000000, -1.000000000000000000 ) ) ;
#31452 = DIRECTION ( 'NONE',  ( -0.000000000000000000, -0.000000000000000000, -1.000000000000000000 ) ) ;
#31453 = CONICAL_SURFACE ( 'NONE', #34474, 3.000000000000000888, 0.9599310885968804774 ) ;
#31454 = DIRECTION ( 'NONE',  ( 0.000000000000000000, 0.000000000000000000, 1.000000000000000000 ) ) ;
#31455 = AXIS2_PLACEMENT_3D ( 'NONE', #1792, #16232, #35930 ) ;
#31456 = ORIENTED_EDGE ( 'NONE', *, *, #21287, .F. ) ;
#31457 =( GEOMETRIC_REPRESENTATION_CONTEXT ( 3 ) GLOBAL_UNCERTAINTY_ASSIGNED_CONTEXT ( ( #9941 ) ) GLOBAL_UNIT_ASSIGNED_CONTEXT ( ( #37074, #8005, #14183 ) ) REPRESENTATION_CONTEXT ( 'NONE', 'WORKASPACE' ) );
#31458 = ORIENTED_EDGE ( 'NONE', *, *, #20665, .F. ) ;
#31459 = CARTESIAN_POINT ( 'NONE',  ( -149.8799519615616873, -5.999999999998430589, 32.55002500000000509 ) ) ;
#31460 = ADVANCED_FACE ( 'NONE', ( #32152 ), #6287, .F. ) ;
#31461 = DIRECTION ( 'NONE',  ( -0.000000000000000000, -0.000000000000000000, 1.000000000000000000 ) ) ;
#31462 = CYLINDRICAL_SURFACE ( 'NONE', #24504, 1.999999999999998224 ) ;
#31463 = ORIENTED_EDGE ( 'NONE', *, *, #8649, .F. ) ;
#31464 = AXIS2_PLACEMENT_3D ( 'NONE', #16629, #7830, #7994 ) ;
#31465 = FACE_BOUND ( 'NONE', #16980, .T. ) ;
#31466 = EDGE_LOOP ( 'NONE', ( #13522, #36902, #2494, #1489 ) ) ;
#31467 = ORIENTED_EDGE ( 'NONE', *, *, #27781, .F. ) ;
#31468 = LINE ( 'NONE', #544, #24830 ) ;
#31469 = ORIENTED_EDGE ( 'NONE', *, *, #26233, .T. ) ;
#31470 = PRESENTATION_STYLE_ASSIGNMENT (( #17252 ) ) ;
#31471 = DIRECTION ( 'NONE',  ( 0.000000000000000000, 0.000000000000000000, -1.000000000000000000 ) ) ;
#31472 = AXIS2_PLACEMENT_3D ( 'NONE', #31725, #9609, #20850 ) ;
#31473 = DIRECTION ( 'NONE',  ( 0.000000000000000000, 0.000000000000000000, 1.000000000000000000 ) ) ;
#31474 = ORIENTED_EDGE ( 'NONE', *, *, #11427, .F. ) ;
#31475 = AXIS2_PLACEMENT_3D ( 'NONE', #30593, #25518, #31148 ) ;
#31476 = EDGE_LOOP ( 'NONE', ( #30691, #34832, #9069, #1936 ) ) ;
#31477 = VECTOR ( 'NONE', #13065, 1000.000000000000000 ) ;
#31478 = ORIENTED_EDGE ( 'NONE', *, *, #8414, .F. ) ;
#31479 = AXIS2_PLACEMENT_3D ( 'NONE', #18947, #18759, #21582 ) ;
#31480 = ADVANCED_FACE ( 'NONE', ( #31948 ), #843, .F. ) ;
#31481 = AXIS2_PLACEMENT_3D ( 'NONE', #24836, #15833, #29902 ) ;
#31482 = ORIENTED_EDGE ( 'NONE', *, *, #3108, .T. ) ;
#31483 = CIRCLE ( 'NONE', #27324, 2.000000000000001776 ) ;
#31484 = EDGE_LOOP ( 'NONE', ( #9634, #26037 ) ) ;
#31485 = DIRECTION ( 'NONE',  ( 0.000000000000000000, 0.000000000000000000, 1.000000000000000000 ) ) ;
#31486 = CARTESIAN_POINT ( 'NONE',  ( -10.00000337463125000, -86.60254037844400443, 17.49999999999999645 ) ) ;
#31487 = CARTESIAN_POINT ( 'NONE',  ( 0.000000000000000000, 0.000000000000000000, -5.000000000000000000 ) ) ;
#31488 = CARTESIAN_POINT ( 'NONE',  ( 3.000000000000000000, 2.935248768560057453, -3.903127820947815962E-15 ) ) ;
#31489 = DIRECTION ( 'NONE',  ( 0.000000000000000000, 0.000000000000000000, -1.000000000000000000 ) ) ;
#31490 = VERTEX_POINT ( 'NONE', #3494 ) ;
#31491 = DIRECTION ( 'NONE',  ( 0.000000000000000000, 0.000000000000000000, 1.000000000000000000 ) ) ;
#31492 = AXIS2_PLACEMENT_3D ( 'NONE', #8207, #11545, #36534 ) ;
#31493 = LINE ( 'NONE', #14449, #3618 ) ;
#31494 = DIRECTION ( 'NONE',  ( 1.000000000000000000, 0.000000000000000000, 0.000000000000000000 ) ) ;
#31495 = ORIENTED_EDGE ( 'NONE', *, *, #12325, .F. ) ;
#31496 = DIRECTION ( 'NONE',  ( 0.000000000000000000, 0.000000000000000000, 1.000000000000000000 ) ) ;
#31497 = CYLINDRICAL_SURFACE ( 'NONE', #18988, 3.000000000000000888 ) ;
#31498 = ORIENTED_EDGE ( 'NONE', *, *, #16239, .T. ) ;
#31499 = AXIS2_PLACEMENT_3D ( 'NONE', #12800, #27067, #10014 ) ;
#31500 = ORIENTED_EDGE ( 'NONE', *, *, #6232, .T. ) ;
#31501 = DIRECTION ( 'NONE',  ( 1.000000000000000000, 0.000000000000000000, 0.000000000000000000 ) ) ;
#31502 = CIRCLE ( 'NONE', #21316, 2.000000000000001776 ) ;
#31503 = CARTESIAN_POINT ( 'NONE',  ( -80.00000337463096400, -34.64101615137762025, -9.999999999999998224 ) ) ;
#31504 = EDGE_CURVE ( 'NONE', #30372, #14697, #2051, .T. ) ;
#31505 = DIRECTION ( 'NONE',  ( 0.000000000000000000, 0.000000000000000000, -1.000000000000000000 ) ) ;
#31506 = CARTESIAN_POINT ( 'NONE',  ( -65.00000337463104927, -25.98076211353322051, -9.999999999999998224 ) ) ;
#31507 = ORIENTED_EDGE ( 'NONE', *, *, #34334, .F. ) ;
#31508 = EDGE_LOOP ( 'NONE', ( #31546, #25816, #32148, #9780, #33834 ) ) ;
#31509 = VECTOR ( 'NONE', #2143, 1000.000000000000000 ) ;
#31510 = CIRCLE ( 'NONE', #12332, 2.000000000000001776 ) ;
#31511 = AXIS2_PLACEMENT_3D ( 'NONE', #24191, #30006, #27008 ) ;
#31512 = DIRECTION ( 'NONE',  ( 0.000000000000000000, 0.000000000000000000, 1.000000000000000000 ) ) ;
#31514 = AXIS2_PLACEMENT_3D ( 'NONE', #1349, #12967, #15425 ) ;
#31513 = LINE ( 'NONE', #17293, #32667 ) ;
#31515 = CARTESIAN_POINT ( 'NONE',  ( 4.999999999999999112, -2.417244626924488049, -5.688952927922135139 ) ) ;
#31516 = AXIS2_PLACEMENT_3D ( 'NONE', #4988, #10811, #10252 ) ;
#31517 = ORIENTED_EDGE ( 'NONE', *, *, #67, .F. ) ;
#31518 = DIRECTION ( 'NONE',  ( 0.000000000000000000, 0.000000000000000000, 1.000000000000000000 ) ) ;
#31519 = EDGE_LOOP ( 'NONE', ( #4329, #3768, #26911, #1979, #27688 ) ) ;
#31520 = ORIENTED_EDGE ( 'NONE', *, *, #21359, .F. ) ;
#31521 = LINE ( 'NONE', #36297, #21174 ) ;
#31522 = EDGE_CURVE ( 'NONE', #27267, #35279, #28384, .T. ) ;
#31523 = DIRECTION ( 'NONE',  ( 0.000000000000000000, -0.000000000000000000, 1.000000000000000000 ) ) ;
#31524 = ORIENTED_EDGE ( 'NONE', *, *, #18347, .T. ) ;
#31525 = ORIENTED_EDGE ( 'NONE', *, *, #19867, .F. ) ;
#31526 = CYLINDRICAL_SURFACE ( 'NONE', #11179, 1.750000000000015765 ) ;
#31527 = EDGE_CURVE ( 'NONE', #36437, #26422, #8635, .T. ) ;
#31528 = AXIS2_PLACEMENT_3D ( 'NONE', #23299, #20464, #9039 ) ;
#31529 = DIRECTION ( 'NONE',  ( 0.000000000000000000, 0.000000000000000000, -1.000000000000000000 ) ) ;
#31530 = CARTESIAN_POINT ( 'NONE',  ( -15.00000337463125710, -77.94228634059960825, 12.50000000000000000 ) ) ;
#31531 = CIRCLE ( 'NONE', #26141, 2.000000000000001776 ) ;
#31532 = ORIENTED_EDGE ( 'NONE', *, *, #2091, .F. ) ;
#31533 = CARTESIAN_POINT ( 'NONE',  ( 3.000000000000000000, -1.467624384280032501, -2.541999999999998483 ) ) ;
#31534 = FACE_BOUND ( 'NONE', #36233, .T. ) ;
#31535 = EDGE_CURVE ( 'NONE', #3432, #26470, #9236, .T. ) ;
#31536 = FACE_OUTER_BOUND ( 'NONE', #24073, .T. ) ;
#31537 = DIRECTION ( 'NONE',  ( 1.000000000000000000, 0.000000000000000000, 0.000000000000000000 ) ) ;
#31538 = DIRECTION ( 'NONE',  ( -0.000000000000000000, -0.000000000000000000, -1.000000000000000000 ) ) ;
#31539 = AXIS2_PLACEMENT_3D ( 'NONE', #12861, #30673, #19081 ) ;
#31540 = DIRECTION ( 'NONE',  ( 1.000000000000000000, 0.000000000000000000, 0.000000000000000000 ) ) ;
#31541 = CIRCLE ( 'NONE', #15390, 3.499999999999996003 ) ;
#31542 = AXIS2_PLACEMENT_3D ( 'NONE', #36523, #4450, #7837 ) ;
#31543 = DIRECTION ( 'NONE',  ( 0.000000000000000000, 0.000000000000000000, 1.000000000000000000 ) ) ;
#31544 = ADVANCED_FACE ( 'NONE', ( #108 ), #6110, .F. ) ;
#31545 = DIRECTION ( 'NONE',  ( 0.000000000000000000, 0.000000000000000000, 1.000000000000000000 ) ) ;
#31546 = ORIENTED_EDGE ( 'NONE', *, *, #36728, .F. ) ;
#31547 = DIRECTION ( 'NONE',  ( 0.000000000000000000, 0.000000000000000000, 1.000000000000000000 ) ) ;
#31548 = CARTESIAN_POINT ( 'NONE',  ( -4.378301941662551044, 3.528365556573270556, -4.190643565754935906 ) ) ;
#31549 = DIRECTION ( 'NONE',  ( -1.000000000000000000, 0.000000000000000000, 0.000000000000000000 ) ) ;
#31550 = ORIENTED_EDGE ( 'NONE', *, *, #28921, .F. ) ;
#31551 = CIRCLE ( 'NONE', #21368, 2.000000000000000000 ) ;
#31552 = EDGE_LOOP ( 'NONE', ( #13239, #29908 ) ) ;
#31553 = ORIENTED_EDGE ( 'NONE', *, *, #19629, .T. ) ;
#31554 = DIRECTION ( 'NONE',  ( 1.000000000000000000, 0.000000000000000000, 0.000000000000000000 ) ) ;
#31555 = DIRECTION ( 'NONE',  ( 1.000000000000000000, 0.000000000000000000, 0.000000000000000000 ) ) ;
#31556 = CARTESIAN_POINT ( 'NONE',  ( -5.000003374631269537, -77.94228634059960825, -5.000000000000000000 ) ) ;
#31557 = ORIENTED_EDGE ( 'NONE', *, *, #17999, .F. ) ;
#31558 = CIRCLE ( 'NONE', #28568, 2.000000000000001776 ) ;
#31559 = CYLINDRICAL_SURFACE ( 'NONE', #36494, 30.00000000000000000 ) ;
#31560 = EDGE_CURVE ( 'NONE', #22867, #18257, #30831, .T. ) ;
#31561 = AXIS2_PLACEMENT_3D ( 'NONE', #25034, #36466, #36273 ) ;
#31562 = ORIENTED_EDGE ( 'NONE', *, *, #24443, .T. ) ;
#31563 = CARTESIAN_POINT ( 'NONE',  ( 47.63139720814400846, -27.50000000000022737, -15.00000000000000000 ) ) ;
#31564 = EDGE_LOOP ( 'NONE', ( #28983, #30301 ) ) ;
#31565 = DIRECTION ( 'NONE',  ( 0.000000000000000000, 0.000000000000000000, 1.000000000000000000 ) ) ;
#31566 = ORIENTED_EDGE ( 'NONE', *, *, #8787, .F. ) ;
#31567 = VECTOR ( 'NONE', #36490, 1000.000000000000000 ) ;
#31568 = EDGE_LOOP ( 'NONE', ( #1731, #13679 ) ) ;
#31569 = EDGE_CURVE ( 'NONE', #17870, #148, #23014, .T. ) ;
#31570 = AXIS2_PLACEMENT_3D ( 'NONE', #7590, #30267, #13384 ) ;
#31571 = AXIS2_PLACEMENT_3D ( 'NONE', #30435, #1554, #35890 ) ;
#31572 =( NAMED_UNIT ( * ) SI_UNIT ( $, .STERADIAN. ) SOLID_ANGLE_UNIT ( ) );
#31573 = DIRECTION ( 'NONE',  ( -1.000000000000000000, 0.000000000000000000, 0.000000000000000000 ) ) ;
#31574 = EDGE_CURVE ( 'NONE', #36512, #33080, #11017, .T. ) ;
#31575 = LINE ( 'NONE', #36541, #26659 ) ;
#31576 = ORIENTED_EDGE ( 'NONE', *, *, #24885, .F. ) ;
#31577 = DIRECTION ( 'NONE',  ( 1.000000000000000000, 0.000000000000000000, 0.000000000000000000 ) ) ;
#31578 = CIRCLE ( 'NONE', #3436, 2.000000000000000000 ) ;
#31579 = CARTESIAN_POINT ( 'NONE',  ( -70.00000337463102085, -34.64101615137762025, 12.50000000000000000 ) ) ;
#31580 = CYLINDRICAL_SURFACE ( 'NONE', #831, 2.000000000000000000 ) ;
#31581 = EDGE_LOOP ( 'NONE', ( #30572, #11160 ) ) ;
#31582 = DIRECTION ( 'NONE',  ( 0.000000000000000000, 0.000000000000000000, 1.000000000000000000 ) ) ;
#31584 = FACE_OUTER_BOUND ( 'NONE', #8093, .T. ) ;
#31583 = AXIS2_PLACEMENT_3D ( 'NONE', #32869, #7187, #795 ) ;
#31585 = ORIENTED_EDGE ( 'NONE', *, *, #3233, .F. ) ;
#31586 = DIRECTION ( 'NONE',  ( 1.000000000000000000, 0.000000000000000000, 0.000000000000000000 ) ) ;
#31587 = AXIS2_PLACEMENT_3D ( 'NONE', #33694, #36522, #19265 ) ;
#31588 = AXIS2_PLACEMENT_3D ( 'NONE', #16520, #5462, #25168 ) ;
#31589 = CARTESIAN_POINT ( 'NONE',  ( -35.00000337463117717, -77.94228634059963667, -9.999999999999998224 ) ) ;
#31590 = CARTESIAN_POINT ( 'NONE',  ( -5.238704763094644612, -1.015773027556931440, -4.085839086323462155 ) ) ;
#31591 = MANIFOLD_SOLID_BREP ( 'TorqueElement', #30954 ) ;
#31593 = AXIS2_PLACEMENT_3D ( 'NONE', #20101, #31529, #26097 ) ;
#31592 = DIRECTION ( 'NONE',  ( -1.000000000000000000, 0.000000000000000000, 0.000000000000000000 ) ) ;
#31594 = CARTESIAN_POINT ( 'NONE',  ( 66.99999662536841072, -25.98076211353320275, -9.999999999999998224 ) ) ;
#31595 = EDGE_CURVE ( 'NONE', #5465, #5553, #7232, .T. ) ;
#31596 = CIRCLE ( 'NONE', #26840, 2.000000000000001776 ) ;
#31597 = ORIENTED_EDGE ( 'NONE', *, *, #32722, .F. ) ;
#31598 = CARTESIAN_POINT ( 'NONE',  ( -70.80619744049063513, -84.18124734178186941, 32.50000000000000000 ) ) ;
#31599 = CARTESIAN_POINT ( 'NONE',  ( -3.374631327851540519E-06, 86.60254037844397601, 17.49999999999999645 ) ) ;
#31600 = VERTEX_POINT ( 'NONE', #17539 ) ;
#31601 = CIRCLE ( 'NONE', #26822, 2.000000000000000000 ) ;
#31602 = ORIENTED_EDGE ( 'NONE', *, *, #20563, .F. ) ;
#31603 = ORIENTED_EDGE ( 'NONE', *, *, #20884, .F. ) ;
#31604 = CARTESIAN_POINT ( 'NONE',  ( 7.041719095097282852E-16, 78.44802294027068967, -24.99999999999999645 ) ) ;
#31605 = DIRECTION ( 'NONE',  ( -1.000000000000000000, 0.000000000000000000, 0.000000000000000000 ) ) ;
#31606 = CARTESIAN_POINT ( 'NONE',  ( 42.99999662536848888, -77.94228634059960825, 12.50000000000000000 ) ) ;
#31607 = VECTOR ( 'NONE', #22608, 1000.000000000000000 ) ;
#31608 = ADVANCED_FACE ( 'NONE', ( #33612 ), #9669, .F. ) ;
#31609 = VECTOR ( 'NONE', #8657, 1000.000000000000000 ) ;
#31610 = DIRECTION ( 'NONE',  ( -1.000000000000000000, 0.000000000000000000, 0.000000000000000000 ) ) ;
#31611 = ORIENTED_EDGE ( 'NONE', *, *, #21359, .T. ) ;
#31612 = ADVANCED_FACE ( 'NONE', ( #26917 ), #22173, .T. ) ;
#31613 = CYLINDRICAL_SURFACE ( 'NONE', #17936, 2.000000000000000000 ) ;
#31614 = VERTEX_POINT ( 'NONE', #24277 ) ;
#31615 = AXIS2_PLACEMENT_3D ( 'NONE', #13220, #18847, #10784 ) ;
#31616 = AXIS2_PLACEMENT_3D ( 'NONE', #6177, #25514, #36957 ) ;
#31617 = FACE_BOUND ( 'NONE', #1182, .T. ) ;
#31618 = AXIS2_PLACEMENT_3D ( 'NONE', #13058, #21504, #9867 ) ;
#31619 = EDGE_CURVE ( 'NONE', #26391, #13843, #33808, .T. ) ;
#31620 = AXIS2_PLACEMENT_3D ( 'NONE', #14452, #34168, #16898 ) ;
#31621 = DIRECTION ( 'NONE',  ( 1.000000000000000000, 0.000000000000000000, 0.000000000000000000 ) ) ;
#31622 = ADVANCED_FACE ( 'NONE', ( #7914 ), #9837, .F. ) ;
#31623 = CARTESIAN_POINT ( 'NONE',  ( 3.500000000000000888, 55.00000000000000000, -5.000000000000000888 ) ) ;
#31624 = EDGE_CURVE ( 'NONE', #34831, #14526, #251, .T. ) ;
#31625 = EDGE_CURVE ( 'NONE', #20160, #36282, #31951, .T. ) ;
#31626 = DIRECTION ( 'NONE',  ( -0.5000000000000041078, -0.8660254037844364872, 0.000000000000000000 ) ) ;
#31627 = DIRECTION ( 'NONE',  ( 1.000000000000000000, 0.000000000000000000, 0.000000000000000000 ) ) ;
#31628 = AXIS2_PLACEMENT_3D ( 'NONE', #31530, #5870, #23100 ) ;
#31629 = DIRECTION ( 'NONE',  ( 1.000000000000000000, 0.000000000000000000, 0.000000000000000000 ) ) ;
#31630 = CARTESIAN_POINT ( 'NONE',  ( 0.000000000000000000, 0.000000000000000000, -5.000000000000000000 ) ) ;
#31631 = VERTEX_POINT ( 'NONE', #21275 ) ;
#31632 = DIRECTION ( 'NONE',  ( 0.000000000000000000, 0.000000000000000000, 1.000000000000000000 ) ) ;
#31633 = DIRECTION ( 'NONE',  ( -1.000000000000000000, 0.000000000000000000, -0.000000000000000000 ) ) ;
#31634 = VECTOR ( 'NONE', #48, 1000.000000000000000 ) ;
#31635 = CARTESIAN_POINT ( 'NONE',  ( -3.374631334790434423E-06, 69.28203230275516944, -5.000000000000000000 ) ) ;
#31636 = ADVANCED_FACE ( 'NONE', ( #1039 ), #7041, .T. ) ;
#31637 = EDGE_CURVE ( 'NONE', #30617, #18465, #29577, .T. ) ;
#31638 = ORIENTED_EDGE ( 'NONE', *, *, #23180, .T. ) ;
#31639 = ORIENTED_EDGE ( 'NONE', *, *, #16543, .F. ) ;
#31640 = EDGE_CURVE ( 'NONE', #6520, #30108, #5058, .T. ) ;
#31641 = AXIS2_PLACEMENT_3D ( 'NONE', #2621, #30748, #19327 ) ;
#31642 = ORIENTED_EDGE ( 'NONE', *, *, #27254, .T. ) ;
#31643 = CIRCLE ( 'NONE', #16118, 0.2500000000000002220 ) ;
#31644 = AXIS2_PLACEMENT_3D ( 'NONE', #6098, #34794, #17522 ) ;
#31645 = DIRECTION ( 'NONE',  ( 0.000000000000000000, 0.000000000000000000, -1.000000000000000000 ) ) ;
#31646 = AXIS2_PLACEMENT_3D ( 'NONE', #34286, #36912, #31106 ) ;
#31647 = CARTESIAN_POINT ( 'NONE',  ( -67.00000337463106348, -60.62177826491083010, 17.49999999999999645 ) ) ;
#31648 = DIRECTION ( 'NONE',  ( 1.000000000000000000, 0.000000000000000000, 0.000000000000000000 ) ) ;
#31649 = FACE_OUTER_BOUND ( 'NONE', #2810, .T. ) ;
#31650 = DIRECTION ( 'NONE',  ( 1.000000000000000000, 0.000000000000000000, 0.000000000000000000 ) ) ;
#31651 = EDGE_LOOP ( 'NONE', ( #3260, #31093, #10599, #3664, #8923 ) ) ;
#31652 = ORIENTED_EDGE ( 'NONE', *, *, #33725, .F. ) ;
#31653 = DIRECTION ( 'NONE',  ( 1.000000000000000000, 0.000000000000000000, 0.000000000000000000 ) ) ;
#31654 = EDGE_CURVE ( 'NONE', #11580, #3735, #14623, .T. ) ;
#31655 = LINE ( 'NONE', #14586, #19969 ) ;
#31656 = EDGE_CURVE ( 'NONE', #4290, #25888, #1435, .T. ) ;
#31657 = CARTESIAN_POINT ( 'NONE',  ( 83.47442710120355969, -31.09745072740822991, -5.000000000000011546 ) ) ;
#31658 = VERTEX_POINT ( 'NONE', #1401 ) ;
#31659 = FACE_BOUND ( 'NONE', #7229, .T. ) ;
#31660 = CIRCLE ( 'NONE', #2944, 2.000000000000001776 ) ;
#31661 = ORIENTED_EDGE ( 'NONE', *, *, #33769, .T. ) ;
#31662 = VERTEX_POINT ( 'NONE', #35729 ) ;
#31663 = EDGE_CURVE ( 'NONE', #6793, #3051, #29520, .T. ) ;
#31664 = VECTOR ( 'NONE', #4380, 1000.000000000000000 ) ;
#31665 = CYLINDRICAL_SURFACE ( 'NONE', #18858, 2.000000000000001776 ) ;
#31666 = ORIENTED_EDGE ( 'NONE', *, *, #6085, .T. ) ;
#31667 = CARTESIAN_POINT ( 'NONE',  ( -2.000003374631289521, -69.28203230275519786, 17.49999999999999645 ) ) ;
#31668 = DIRECTION ( 'NONE',  ( -0.000000000000000000, -0.000000000000000000, -1.000000000000000000 ) ) ;
#31669 = ORIENTED_EDGE ( 'NONE', *, *, #7511, .F. ) ;
#31670 = VERTEX_POINT ( 'NONE', #18276 ) ;
#31671 = CIRCLE ( 'NONE', #19732, 2.000000000000001776 ) ;
#31672 = EDGE_CURVE ( 'NONE', #28731, #530, #18211, .T. ) ;
#31673 = ORIENTED_EDGE ( 'NONE', *, *, #25711, .T. ) ;
#31674 = EDGE_CURVE ( 'NONE', #22987, #14529, #36776, .T. ) ;
#31675 = ORIENTED_EDGE ( 'NONE', *, *, #32065, .F. ) ;
#31676 = AXIS2_PLACEMENT_3D ( 'NONE', #34094, #13831, #295 ) ;
#31677 = ORIENTED_EDGE ( 'NONE', *, *, #15517, .T. ) ;
#31678 = ADVANCED_FACE ( 'NONE', ( #12823 ), #10038, .F. ) ;
#31679 = DIRECTION ( 'NONE',  ( 0.000000000000000000, 0.000000000000000000, -1.000000000000000000 ) ) ;
#31680 = ADVANCED_FACE ( 'NONE', ( #24989 ), #22342, .F. ) ;
#31681 =( NAMED_UNIT ( * ) SI_UNIT ( $, .STERADIAN. ) SOLID_ANGLE_UNIT ( ) );
#31682 = CYLINDRICAL_SURFACE ( 'NONE', #25062, 5.750000000000005329 ) ;
#31683 = LINE ( 'NONE', #25515, #14519 ) ;
#31684 = CARTESIAN_POINT ( 'NONE',  ( 19.99999662536861678, -86.60254037844400443, -5.000000000000000000 ) ) ;
#31685 = ORIENTED_EDGE ( 'NONE', *, *, #18105, .T. ) ;
#31686 = DIRECTION ( 'NONE',  ( 0.000000000000000000, 0.000000000000000000, 1.000000000000000000 ) ) ;
#31687 = CARTESIAN_POINT ( 'NONE',  ( -0.4317663827706223478, -5.811727376006694534, -4.266919140436448821 ) ) ;
#31688 = CIRCLE ( 'NONE', #11934, 30.00000000000000000 ) ;
#31689 = DIRECTION ( 'NONE',  ( 0.000000000000000000, 0.000000000000000000, 1.000000000000000000 ) ) ;
#31690 = ORIENTED_EDGE ( 'NONE', *, *, #35459, .F. ) ;
#31691 = CARTESIAN_POINT ( 'NONE',  ( -35.00000337463116296, -60.62177826491080168, -9.999999999999998224 ) ) ;
#31692 = CIRCLE ( 'NONE', #14340, 6.000000000000005329 ) ;
#31693 = LINE ( 'NONE', #26065, #28551 ) ;
#31694 = VERTEX_POINT ( 'NONE', #16735 ) ;
#31695 = VERTEX_POINT ( 'NONE', #22526 ) ;
#31696 = CARTESIAN_POINT ( 'NONE',  ( -145.0000000000001137, -5.999999999998481215, 27.50000000000000000 ) ) ;
#31697 = DIRECTION ( 'NONE',  ( -1.000000000000000000, -0.000000000000000000, -0.000000000000000000 ) ) ;
#31698 = DIRECTION ( 'NONE',  ( 0.000000000000000000, 0.000000000000000000, -1.000000000000000000 ) ) ;
#31699 = CARTESIAN_POINT ( 'NONE',  ( -3.374631334790434423E-06, 69.28203230275516944, -9.999999999999998224 ) ) ;
#31700 = ORIENTED_EDGE ( 'NONE', *, *, #17205, .T. ) ;
#31701 = AXIS2_PLACEMENT_3D ( 'NONE', #28622, #33887, #31249 ) ;
#31702 = EDGE_CURVE ( 'NONE', #9342, #16686, #14012, .T. ) ;
#31703 = DIRECTION ( 'NONE',  ( 0.000000000000000000, -1.000000000000000000, 0.000000000000000000 ) ) ;
#31704 = FACE_OUTER_BOUND ( 'NONE', #15206, .T. ) ;
#31705 = CARTESIAN_POINT ( 'NONE',  ( -2.775557561562891351E-14, 19.94802294027085310, -19.99999999999999645 ) ) ;
#31706 = ORIENTED_EDGE ( 'NONE', *, *, #2624, .T. ) ;
#31707 = CARTESIAN_POINT ( 'NONE',  ( -15.00000337463126066, 77.94228634059957983, -5.000000000000000000 ) ) ;
#31708 = AXIS2_PLACEMENT_3D ( 'NONE', #30023, #30197, #1515 ) ;
#31709 = ORIENTED_EDGE ( 'NONE', *, *, #19330, .T. ) ;
#31710 = ORIENTED_EDGE ( 'NONE', *, *, #32082, .T. ) ;
#31711 = CARTESIAN_POINT ( 'NONE',  ( -45.00000337463111322, 77.94228634059959404, 12.50000000000000000 ) ) ;
#31712 = AXIS2_PLACEMENT_3D ( 'NONE', #34059, #5543, #8908 ) ;
#31713 = FACE_OUTER_BOUND ( 'NONE', #518, .T. ) ;
#31714 = EDGE_LOOP ( 'NONE', ( #27438, #21428, #2105, #1846, #22567 ) ) ;
#31715 = ORIENTED_EDGE ( 'NONE', *, *, #3708, .F. ) ;
#31716 = DIRECTION ( 'NONE',  ( -0.8660254037844360431, -0.5000000000000045519, 0.000000000000000000 ) ) ;
#31717 = DIRECTION ( 'NONE',  ( 1.000000000000000000, 0.000000000000000000, 0.000000000000000000 ) ) ;
#31718 = CARTESIAN_POINT ( 'NONE',  ( -62.00000337463104927, 34.64101615137757051, -5.000000000000000000 ) ) ;
#31719 = VERTEX_POINT ( 'NONE', #11080 ) ;
#31720 = CARTESIAN_POINT ( 'NONE',  ( -65.00000337463102085, 43.30127018922198801, -9.999999999999998224 ) ) ;
#31721 = EDGE_CURVE ( 'NONE', #21374, #10270, #18824, .T. ) ;
#31722 = FACE_BOUND ( 'NONE', #37094, .T. ) ;
#31723 = CARTESIAN_POINT ( 'NONE',  ( 16.99999662536859901, 77.94228634059957983, -5.000000000000000000 ) ) ;
#31724 = DIRECTION ( 'NONE',  ( -0.000000000000000000, -0.000000000000000000, 1.000000000000000000 ) ) ;
#31725 = CARTESIAN_POINT ( 'NONE',  ( -106.7731239591695669, -98.28784258492920856, 32.55002500000000509 ) ) ;
#31726 = CIRCLE ( 'NONE', #30545, 2.000000000000001776 ) ;
#31727 = DIRECTION ( 'NONE',  ( 1.000000000000000000, 0.000000000000000000, 0.000000000000000000 ) ) ;
#31728 = DIRECTION ( 'NONE',  ( 1.000000000000000000, 0.000000000000000000, 0.000000000000000000 ) ) ;
#31729 = CIRCLE ( 'NONE', #2401, 2.000000000000000000 ) ;
#31730 = DIRECTION ( 'NONE',  ( 1.000000000000000000, 0.000000000000000000, 0.000000000000000000 ) ) ;
#31731 = VERTEX_POINT ( 'NONE', #33784 ) ;
#31732 = DIRECTION ( 'NONE',  ( 1.000000000000000000, 0.000000000000000000, 0.000000000000000000 ) ) ;
#31733 = CARTESIAN_POINT ( 'NONE',  ( -17.55872235085560007, 89.94802294027088863, 32.49999999999999289 ) ) ;
#31734 = AXIS2_PLACEMENT_3D ( 'NONE', #735, #18366, #15361 ) ;
#31735 = CYLINDRICAL_SURFACE ( 'NONE', #14545, 2.000000000000001776 ) ;
#31736 = EDGE_LOOP ( 'NONE', ( #5006, #22458 ) ) ;
#31737 = EDGE_LOOP ( 'NONE', ( #8122, #20098, #12216, #10913 ) ) ;
#31738 = EDGE_LOOP ( 'NONE', ( #24995, #36582, #26924, #17491 ) ) ;
#31739 = AXIS2_PLACEMENT_3D ( 'NONE', #31989, #14970, #6705 ) ;
#31740 = DIRECTION ( 'NONE',  ( 0.000000000000000000, 0.000000000000000000, -1.000000000000000000 ) ) ;
#31741 = DIRECTION ( 'NONE',  ( -1.000000000000000000, 0.000000000000000000, 0.000000000000000000 ) ) ;
#31742 = CARTESIAN_POINT ( 'NONE',  ( 0.000000000000000000, 101.4480229402710734, 32.49999999999999289 ) ) ;
#31743 = ORIENTED_EDGE ( 'NONE', *, *, #13111, .F. ) ;
#31744 = EDGE_CURVE ( 'NONE', #12615, #17955, #32614, .T. ) ;
#31745 = DIRECTION ( 'NONE',  ( 0.000000000000000000, 0.000000000000000000, 1.000000000000000000 ) ) ;
#31746 = ORIENTED_EDGE ( 'NONE', *, *, #36476, .F. ) ;
#31747 = VECTOR ( 'NONE', #622, 1000.000000000000000 ) ;
#31748 = CARTESIAN_POINT ( 'NONE',  ( -23.02818743869751827, -104.7521194859946263, 32.50000000000001421 ) ) ;
#31749 = EDGE_CURVE ( 'NONE', #2553, #35136, #24847, .T. ) ;
#31750 = VERTEX_POINT ( 'NONE', #375 ) ;
#31751 = DIRECTION ( 'NONE',  ( 0.000000000000000000, 0.000000000000000000, -1.000000000000000000 ) ) ;
#31752 = EDGE_LOOP ( 'NONE', ( #28486, #1131 ) ) ;
#31753 = VERTEX_POINT ( 'NONE', #31696 ) ;
#31754 = EDGE_CURVE ( 'NONE', #24605, #15127, #8086, .T. ) ;
#31755 = CARTESIAN_POINT ( 'NONE',  ( -44.13139720814380951, 27.50000000000055422, -5.000000000000000000 ) ) ;
#31756 = CARTESIAN_POINT ( 'NONE',  ( 2.381231458764692110, -4.398698068175666442, -0.5078976954043025183 ) ) ;
#31758 = VECTOR ( 'NONE', #11072, 1000.000000000000000 ) ;
#31757 = LINE ( 'NONE', #20685, #20073 ) ;
#31759 = ORIENTED_EDGE ( 'NONE', *, *, #22294, .T. ) ;
#31760 = CARTESIAN_POINT ( 'NONE',  ( 1.301042606982605321E-15, 5.773502691896264416, -5.553418012614792509 ) ) ;
#31761 = CYLINDRICAL_SURFACE ( 'NONE', #9310, 33.00000000000001421 ) ;
#31762 = DIRECTION ( 'NONE',  ( 1.000000000000000000, 0.000000000000000000, 0.000000000000000000 ) ) ;
#31763 = ORIENTED_EDGE ( 'NONE', *, *, #36622, .T. ) ;
#31764 = DIRECTION ( 'NONE',  ( 1.000000000000000000, 0.000000000000000000, 0.000000000000000000 ) ) ;
#31765 = CYLINDRICAL_SURFACE ( 'NONE', #12553, 2.500000000000000000 ) ;
#31766 = EDGE_LOOP ( 'NONE', ( #15198, #13193, #7430, #8654, #11550, #26046 ) ) ;
#31767 = EDGE_CURVE ( 'NONE', #13910, #6635, #17649, .T. ) ;
#31768 = CARTESIAN_POINT ( 'NONE',  ( -3.374631303565411855E-06, -86.60254037844400443, -5.000000000000000000 ) ) ;
#31769 = CARTESIAN_POINT ( 'NONE',  ( -82.00000337463096400, -34.64101615137762025, -9.999999999999998224 ) ) ;
#31770 = DIRECTION ( 'NONE',  ( 0.000000000000000000, 0.000000000000000000, 1.000000000000000000 ) ) ;
#31771 = DIRECTION ( 'NONE',  ( -0.000000000000000000, -0.000000000000000000, -1.000000000000000000 ) ) ;
#31772 = DIRECTION ( 'NONE',  ( 0.000000000000000000, 0.000000000000000000, 1.000000000000000000 ) ) ;
#31773 = ORIENTED_EDGE ( 'NONE', *, *, #22406, .T. ) ;
#31774 = CARTESIAN_POINT ( 'NONE',  ( 0.4317663827706206270, 5.811727376006657231, -4.266919140436438163 ) ) ;
#31775 = CARTESIAN_POINT ( 'NONE',  ( -35.19434990244938888, 52.39915983220783602, 12.49999999999999822 ) ) ;
#31777 = ADVANCED_FACE ( 'NONE', ( #13899 ), #33983, .F. ) ;
#31776 = ORIENTED_EDGE ( 'NONE', *, *, #19544, .F. ) ;
#31778 = VERTEX_POINT ( 'NONE', #8296 ) ;
#31779 = ORIENTED_EDGE ( 'NONE', *, *, #36350, .T. ) ;
#31780 = ADVANCED_FACE ( 'NONE', ( #31159 ), #5476, .F. ) ;
#31781 = TOROIDAL_SURFACE ( 'NONE', #29383, 17.55872235085559652, 2.000000000000000000 ) ;
#31782 = FILL_AREA_STYLE ('',( #17374 ) ) ;
#31783 = DIRECTION ( 'NONE',  ( 0.000000000000000000, 0.000000000000000000, 1.000000000000000000 ) ) ;
#31784 = CARTESIAN_POINT ( 'NONE',  ( -5.000000000000000000, -4.846777557549235459E-18, -0.5080592402122449114 ) ) ;
#31785 = CYLINDRICAL_SURFACE ( 'NONE', #24875, 2.000000000000000000 ) ;
#31786 = EDGE_LOOP ( 'NONE', ( #9940, #22171 ) ) ;
#31787 = DIRECTION ( 'NONE',  ( 1.000000000000000000, 0.000000000000000000, 0.000000000000000000 ) ) ;
#31788 = ADVANCED_FACE ( 'NONE', ( #28325 ), #2646, .F. ) ;
#31789 = ORIENTED_EDGE ( 'NONE', *, *, #13699, .F. ) ;
#31790 = FACE_BOUND ( 'NONE', #28148, .T. ) ;
#31791 = EDGE_CURVE ( 'NONE', #35055, #22308, #2079, .T. ) ;
#31792 = DIRECTION ( 'NONE',  ( 1.000000000000000000, 0.000000000000000000, 0.000000000000000000 ) ) ;
#31793 = CARTESIAN_POINT ( 'NONE',  ( 79.99999662536833966, 34.64101615137759183, -9.999999999999998224 ) ) ;
#31794 = CARTESIAN_POINT ( 'NONE',  ( 79.99999662536833966, -3.469446951953614189E-15, -5.000000000000000000 ) ) ;
#31795 = APPLICATION_PROTOCOL_DEFINITION ( 'draft international standard', 'automotive_design', 1998, #18530 ) ;
#31796 = DIRECTION ( 'NONE',  ( 1.000000000000000000, 0.000000000000000000, 0.000000000000000000 ) ) ;
#31797 = PLANE ( 'NONE',  #20972 ) ;
#31798 = CARTESIAN_POINT ( 'NONE',  ( 22.99999662536857059, 77.94228634059957983, -5.000000000000000000 ) ) ;
#31799 = ORIENTED_EDGE ( 'NONE', *, *, #25511, .T. ) ;
#31800 = FACE_OUTER_BOUND ( 'NONE', #31818, .T. ) ;
#31801 = CARTESIAN_POINT ( 'NONE',  ( 3.000000000000000000, -1.467624384280032501, -2.541999999999998483 ) ) ;
#31802 = CARTESIAN_POINT ( 'NONE',  ( -47.00000337463111322, 77.94228634059959404, -9.999999999999998224 ) ) ;
#31803 = ORIENTED_EDGE ( 'NONE', *, *, #5333, .F. ) ;
#31804 = EDGE_CURVE ( 'NONE', #4245, #12365, #22728, .T. ) ;
#31805 = ORIENTED_EDGE ( 'NONE', *, *, #18337, .F. ) ;
#31806 = VERTEX_POINT ( 'NONE', #19896 ) ;
#31807 = CARTESIAN_POINT ( 'NONE',  ( 6.999996625368645198, 77.94228634059957983, 17.49999999999999645 ) ) ;
#31808 = EDGE_CURVE ( 'NONE', #1539, #21899, #12857, .T. ) ;
#31809 = DIRECTION ( 'NONE',  ( 0.000000000000000000, 0.000000000000000000, 1.000000000000000000 ) ) ;
#31810 = CIRCLE ( 'NONE', #20449, 2.000000000000000000 ) ;
#31811 = EDGE_CURVE ( 'NONE', #25464, #20246, #1488, .T. ) ;
#31812 = DIRECTION ( 'NONE',  ( 0.000000000000000000, 0.000000000000000000, 1.000000000000000000 ) ) ;
#31813 = CARTESIAN_POINT ( 'NONE',  ( 0.000000000000000000, 0.000000000000000000, -5.000000000000000000 ) ) ;
#31814 = CIRCLE ( 'NONE', #30635, 2.000000000000000000 ) ;
#31815 = DIRECTION ( 'NONE',  ( 1.000000000000000000, 0.000000000000000000, 0.000000000000000000 ) ) ;
#31816 = FACE_OUTER_BOUND ( 'NONE', #10880, .T. ) ;
#31817 = VERTEX_POINT ( 'NONE', #14626 ) ;
#31818 = EDGE_LOOP ( 'NONE', ( #11634, #23514, #10891, #32249, #5329 ) ) ;
#31819 = LINE ( 'NONE', #32203, #896 ) ;
#31820 = CARTESIAN_POINT ( 'NONE',  ( 74.99999662536836809, 43.30127018922198801, -9.999999999999998224 ) ) ;
#31821 = CARTESIAN_POINT ( 'NONE',  ( 47.99999662536846756, 69.28203230275516944, 17.49999999999999645 ) ) ;
#31822 = VERTEX_POINT ( 'NONE', #11618 ) ;
#31823 = ADVANCED_FACE ( 'NONE', ( #23072 ), #34521, .F. ) ;
#31824 = FACE_BOUND ( 'NONE', #13776, .T. ) ;
#31825 = ORIENTED_EDGE ( 'NONE', *, *, #7937, .T. ) ;
#31826 = ORIENTED_EDGE ( 'NONE', *, *, #12058, .T. ) ;
#31827 = DIRECTION ( 'NONE',  ( 0.4999999999999919509, -0.8660254037844433705, 0.000000000000000000 ) ) ;
#31828 = VERTEX_POINT ( 'NONE', #21007 ) ;
#31829 = DIRECTION ( 'NONE',  ( 0.000000000000000000, 0.000000000000000000, -1.000000000000000000 ) ) ;
#31830 = AXIS2_PLACEMENT_3D ( 'NONE', #30627, #4944, #5131 ) ;
#31831 = CYLINDRICAL_SURFACE ( 'NONE', #4144, 2.000000000000001776 ) ;
#31832 = ORIENTED_EDGE ( 'NONE', *, *, #35981, .F. ) ;
#31833 = ORIENTED_EDGE ( 'NONE', *, *, #31560, .F. ) ;
#31834 = ORIENTED_EDGE ( 'NONE', *, *, #2395, .F. ) ;
#31835 = ORIENTED_EDGE ( 'NONE', *, *, #4941, .F. ) ;
#31836 = EDGE_CURVE ( 'NONE', #23515, #19493, #22421, .T. ) ;
#31837 = ORIENTED_EDGE ( 'NONE', *, *, #28005, .F. ) ;
#31838 = DIRECTION ( 'NONE',  ( 1.000000000000000000, 0.000000000000000000, 0.000000000000000000 ) ) ;
#31839 = CARTESIAN_POINT ( 'NONE',  ( 19.53925848833874213, 89.94802294027088863, 30.77834620192012594 ) ) ;
#31840 = EDGE_CURVE ( 'NONE', #20325, #33375, #12220, .T. ) ;
#31841 = DIRECTION ( 'NONE',  ( 0.000000000000000000, 0.000000000000000000, 1.000000000000000000 ) ) ;
#31842 = CARTESIAN_POINT ( 'NONE',  ( 106.9296898191251159, 51.67694400691266310, 32.49999999999999289 ) ) ;
#31843 = DIRECTION ( 'NONE',  ( 1.000000000000000000, 0.000000000000000000, 0.000000000000000000 ) ) ;
#31844 = ORIENTED_EDGE ( 'NONE', *, *, #19076, .F. ) ;
#31845 = DIRECTION ( 'NONE',  ( 1.000000000000000000, 0.000000000000000000, 0.000000000000000000 ) ) ;
#31846 = EDGE_CURVE ( 'NONE', #5584, #11561, #14652, .T. ) ;
#31847 = CIRCLE ( 'NONE', #15714, 2.000000000000001776 ) ;
#31848 = VECTOR ( 'NONE', #2852, 1000.000000000000000 ) ;
#31849 = DIRECTION ( 'NONE',  ( 1.000000000000000000, 0.000000000000000000, 0.000000000000000000 ) ) ;
#31850 = CARTESIAN_POINT ( 'NONE',  ( 23.49154088336464241, -103.5526315789473699, 27.50000000000000000 ) ) ;
#31851 = ORIENTED_EDGE ( 'NONE', *, *, #27069, .T. ) ;
#31852 = CARTESIAN_POINT ( 'NONE',  ( 0.000000000000000000, 0.000000000000000000, 12.49999999999999822 ) ) ;
#31853 = ADVANCED_FACE ( 'NONE', ( #11813 ), #32040, .F. ) ;
#31854 = FACE_OUTER_BOUND ( 'NONE', #9832, .T. ) ;
#31855 = EDGE_CURVE ( 'NONE', #33050, #20027, #14826, .T. ) ;
#31856 = ORIENTED_EDGE ( 'NONE', *, *, #29821, .F. ) ;
#31857 = ORIENTED_EDGE ( 'NONE', *, *, #30075, .T. ) ;
#31858 = PLANE ( 'NONE',  #35011 ) ;
#31859 = CIRCLE ( 'NONE', #26501, 2.000000000000001776 ) ;
#31860 = DIRECTION ( 'NONE',  ( 0.000000000000000000, 0.000000000000000000, 1.000000000000000000 ) ) ;
#31861 = DIRECTION ( 'NONE',  ( -1.000000000000000000, 0.000000000000000000, 0.000000000000000000 ) ) ;
#31862 = CYLINDRICAL_SURFACE ( 'NONE', #26253, 2.000000000000000000 ) ;
#31863 = EDGE_LOOP ( 'NONE', ( #6564, #23670 ) ) ;
#31864 = EDGE_CURVE ( 'NONE', #31828, #36323, #33207, .T. ) ;
#31865 = CYLINDRICAL_SURFACE ( 'NONE', #13515, 2.000000000000001776 ) ;
#31866 = CARTESIAN_POINT ( 'NONE',  ( -5.000000000000000888, 2.886751345948107783, -0.5999999999999836575 ) ) ;
#31867 = ADVANCED_FACE ( 'NONE', ( #34720 ), #31858, .F. ) ;
#31868 = CARTESIAN_POINT ( 'NONE',  ( -89.42901512340354486, 31.83425564451495404, -4.999999999999997335 ) ) ;
#31869 = EDGE_CURVE ( 'NONE', #28166, #25343, #18384, .T. ) ;
#31870 = ORIENTED_EDGE ( 'NONE', *, *, #21967, .F. ) ;
#31871 = EDGE_CURVE ( 'NONE', #19642, #7368, #26823, .T. ) ;
#31872 = DIRECTION ( 'NONE',  ( 1.000000000000000000, 0.000000000000000000, 0.000000000000000000 ) ) ;
#31873 = ORIENTED_EDGE ( 'NONE', *, *, #26474, .F. ) ;
#31874 = DIRECTION ( 'NONE',  ( 0.000000000000000000, 0.000000000000000000, -1.000000000000000000 ) ) ;
#31875 = CIRCLE ( 'NONE', #23529, 2.000000000000001776 ) ;
#31876 = DIRECTION ( 'NONE',  ( 0.000000000000000000, 0.000000000000000000, 1.000000000000000000 ) ) ;
#31877 = CARTESIAN_POINT ( 'NONE',  ( -3.750000000000001776, 4.592425496802576930E-16, 2.266666666666999674 ) ) ;
#31878 = ORIENTED_EDGE ( 'NONE', *, *, #22485, .T. ) ;
#31879 = ORIENTED_EDGE ( 'NONE', *, *, #20519, .F. ) ;
#31880 = DIRECTION ( 'NONE',  ( -1.000000000000000000, 0.000000000000000000, 0.000000000000000000 ) ) ;
#31881 = CARTESIAN_POINT ( 'NONE',  ( 29.97040607558719572, -71.28181339061548272, -5.000000000000000000 ) ) ;
#31882 = CARTESIAN_POINT ( 'NONE',  ( 54.99999662536844625, 43.30127018922198801, -9.999999999999998224 ) ) ;
#31883 = ORIENTED_EDGE ( 'NONE', *, *, #30481, .F. ) ;
#31884 = LINE ( 'NONE', #15038, #4002 ) ;
#31885 = AXIS2_PLACEMENT_3D ( 'NONE', #28272, #30714, #5034 ) ;
#31886 = FACE_BOUND ( 'NONE', #10013, .T. ) ;
#31887 = AXIS2_PLACEMENT_3D ( 'NONE', #27814, #16034, #21653 ) ;
#31888 = DIRECTION ( 'NONE',  ( -0.5000000000000051070, 0.000000000000000000, 0.8660254037844355990 ) ) ;
#31889 = DIRECTION ( 'NONE',  ( -1.000000000000000000, 0.000000000000000000, 0.000000000000000000 ) ) ;
#31890 = DIRECTION ( 'NONE',  ( 0.000000000000000000, 0.000000000000000000, -1.000000000000000000 ) ) ;
#31891 = FACE_OUTER_BOUND ( 'NONE', #13866, .T. ) ;
#31892 = DIRECTION ( 'NONE',  ( 1.000000000000000000, 0.000000000000000000, 0.000000000000000000 ) ) ;
#31893 = CARTESIAN_POINT ( 'NONE',  ( 5.999999999999998224, 0.000000000000000000, 5.000000000000000000 ) ) ;
#31894 = EDGE_LOOP ( 'NONE', ( #19707, #28892 ) ) ;
#31895 = CARTESIAN_POINT ( 'NONE',  ( -37.50000000000000000, 103.4105893997321886, -19.99999999999999645 ) ) ;
#31896 = CARTESIAN_POINT ( 'NONE',  ( -4.817220356105919699, 3.279784343982782957, -4.266919140436429281 ) ) ;
#31897 = CIRCLE ( 'NONE', #6783, 1.999999999999998224 ) ;
#31898 = CARTESIAN_POINT ( 'NONE',  ( 5.000000000000000000, 30.00000000000000355, 15.00000000000000000 ) ) ;
#31899 = ORIENTED_EDGE ( 'NONE', *, *, #19030, .T. ) ;
#31900 = CIRCLE ( 'NONE', #15766, 2.000000000000001776 ) ;
#31901 = ORIENTED_EDGE ( 'NONE', *, *, #22864, .F. ) ;
#31902 = ORIENTED_EDGE ( 'NONE', *, *, #4650, .T. ) ;
#31903 = CARTESIAN_POINT ( 'NONE',  ( 59.99999662536845335, 34.64101615137759893, 17.49999999999999645 ) ) ;
#31904 = CARTESIAN_POINT ( 'NONE',  ( 67.99999662536836809, -51.96152422706639840, -5.000000000000000000 ) ) ;
#31905 = CARTESIAN_POINT ( 'NONE',  ( -28.00000337463119493, -69.28203230275522628, 12.50000000000000000 ) ) ;
#31906 = EDGE_LOOP ( 'NONE', ( #17868, #20309, #9922, #35893 ) ) ;
#31907 = VERTEX_POINT ( 'NONE', #29255 ) ;
#31908 = CARTESIAN_POINT ( 'NONE',  ( -82.27241335952211898, -47.49999999999924682, 27.50000000000000000 ) ) ;
#31909 = AXIS2_PLACEMENT_3D ( 'NONE', #36087, #18838, #27459 ) ;
#31910 = VERTEX_POINT ( 'NONE', #3937 ) ;
#31911 = EDGE_CURVE ( 'NONE', #11174, #33080, #9184, .T. ) ;
#31912 = CARTESIAN_POINT ( 'NONE',  ( 89.67878100130370456, -27.78182860042797131, 12.49999999999999822 ) ) ;
#31913 = ORIENTED_EDGE ( 'NONE', *, *, #21980, .T. ) ;
#31914 = DIRECTION ( 'NONE',  ( 1.000000000000000000, 0.000000000000000000, 0.000000000000000000 ) ) ;
#31915 = EDGE_LOOP ( 'NONE', ( #22770, #5657 ) ) ;
#31916 = ORIENTED_EDGE ( 'NONE', *, *, #20003, .F. ) ;
#31917 = DIRECTION ( 'NONE',  ( 1.000000000000000000, 0.000000000000000000, 0.000000000000000000 ) ) ;
#31918 = FACE_BOUND ( 'NONE', #8377, .T. ) ;
#31919 = CYLINDRICAL_SURFACE ( 'NONE', #9284, 3.000000000000002665 ) ;
#31920 = ORIENTED_EDGE ( 'NONE', *, *, #6602, .F. ) ;
#31921 = CARTESIAN_POINT ( 'NONE',  ( 86.99999662536831124, -25.98076211353319565, 12.50000000000000000 ) ) ;
#31922 = AXIS2_PLACEMENT_3D ( 'NONE', #4749, #12975, #15991 ) ;
#31923 = CARTESIAN_POINT ( 'NONE',  ( 60.93295298011005201, 19.13981058454729123, 12.49999999999999822 ) ) ;
#31924 = DIRECTION ( 'NONE',  ( -0.000000000000000000, 0.000000000000000000, -1.000000000000000000 ) ) ;
#31925 = CIRCLE ( 'NONE', #16409, 2.000000000000001776 ) ;
#31926 = VERTEX_POINT ( 'NONE', #1136 ) ;
#31927 = CYLINDRICAL_SURFACE ( 'NONE', #27896, 2.000000000000001776 ) ;
#31928 = CYLINDRICAL_SURFACE ( 'NONE', #18576, 2.000000000000001776 ) ;
#31929 = ORIENTED_EDGE ( 'NONE', *, *, #35404, .T. ) ;
#31930 = LINE ( 'NONE', #12064, #8863 ) ;
#31931 = CYLINDRICAL_SURFACE ( 'NONE', #5918, 2.000000000000001776 ) ;
#31932 = DIRECTION ( 'NONE',  ( -1.000000000000000000, 0.000000000000000000, 0.000000000000000000 ) ) ;
#31933 = EDGE_CURVE ( 'NONE', #9156, #4556, #10687, .T. ) ;
#31934 = EDGE_CURVE ( 'NONE', #14326, #10243, #35282, .T. ) ;
#31935 = CYLINDRICAL_SURFACE ( 'NONE', #8104, 3.500000000000000888 ) ;
#31936 = AXIS2_PLACEMENT_3D ( 'NONE', #35398, #9505, #12481 ) ;
#31937 = DIRECTION ( 'NONE',  ( 0.000000000000000000, 0.000000000000000000, 1.000000000000000000 ) ) ;
#31938 = CIRCLE ( 'NONE', #23584, 2.000000000000001776 ) ;
#31939 = CARTESIAN_POINT ( 'NONE',  ( 52.99999662536844625, -60.62177826491080168, -9.999999999999998224 ) ) ;
#31940 = ORIENTED_EDGE ( 'NONE', *, *, #27768, .F. ) ;
#31941 = DIRECTION ( 'NONE',  ( 1.000000000000000000, 0.000000000000000000, 0.000000000000000000 ) ) ;
#31942 = CARTESIAN_POINT ( 'NONE',  ( -15.00000337463126066, 77.94228634059957983, 12.50000000000000000 ) ) ;
#31943 = DIRECTION ( 'NONE',  ( 0.000000000000000000, 0.000000000000000000, 1.000000000000000000 ) ) ;
#31944 = VERTEX_POINT ( 'NONE', #23629 ) ;
#31946 = ORIENTED_EDGE ( 'NONE', *, *, #29334, .T. ) ;
#31945 = EDGE_CURVE ( 'NONE', #21999, #33006, #27822, .T. ) ;
#31947 = ORIENTED_EDGE ( 'NONE', *, *, #36128, .T. ) ;
#31948 = FACE_OUTER_BOUND ( 'NONE', #30403, .T. ) ;
#31949 = DIRECTION ( 'NONE',  ( -0.000000000000000000, -0.000000000000000000, 1.000000000000000000 ) ) ;
#31950 = DIRECTION ( 'NONE',  ( 0.000000000000000000, 0.000000000000000000, -1.000000000000000000 ) ) ;
#31951 = CIRCLE ( 'NONE', #21212, 2.000000000000001776 ) ;
#31952 = CARTESIAN_POINT ( 'NONE',  ( -61.06482292022059966, 72.77422209630346117, 12.49999999999999822 ) ) ;
#31953 = EDGE_LOOP ( 'NONE', ( #35509, #11878 ) ) ;
#31954 = EDGE_CURVE ( 'NONE', #35050, #19348, #18012, .T. ) ;
#31955 = CARTESIAN_POINT ( 'NONE',  ( -22.00000337463124112, -86.60254037844400443, -5.000000000000000000 ) ) ;
#31956 = ORIENTED_EDGE ( 'NONE', *, *, #6005, .F. ) ;
#31957 = FACE_BOUND ( 'NONE', #18817, .T. ) ;
#31958 = VECTOR ( 'NONE', #31297, 1000.000000000000114 ) ;
#31959 = LINE ( 'NONE', #35940, #556 ) ;
#31960 = CIRCLE ( 'NONE', #21224, 2.000000000000001776 ) ;
#31961 = CARTESIAN_POINT ( 'NONE',  ( 0.000000000000000000, 0.000000000000000000, 13.31572692736085095 ) ) ;
#31962 = ORIENTED_EDGE ( 'NONE', *, *, #681, .T. ) ;
#31963 = DIRECTION ( 'NONE',  ( -1.000000000000000000, 0.000000000000000000, 0.000000000000000000 ) ) ;
#31964 = DIRECTION ( 'NONE',  ( -0.7813797561979431983, 0.6240558281147950970, 0.000000000000000000 ) ) ;
#31965 = DIRECTION ( 'NONE',  ( 1.000000000000000000, 0.000000000000000000, 0.000000000000000000 ) ) ;
#31966 = DIRECTION ( 'NONE',  ( 1.000000000000000000, 0.000000000000000000, 0.000000000000000000 ) ) ;
#31967 = DIRECTION ( 'NONE',  ( 1.000000000000000000, -1.047444401652940007E-14, 0.000000000000000000 ) ) ;
#31968 = ADVANCED_FACE ( 'NONE', ( #29434 ), #3753, .F. ) ;
#31969 = EDGE_LOOP ( 'NONE', ( #1365, #29739 ) ) ;
#31970 = CARTESIAN_POINT ( 'NONE',  ( 44.99999662536851019, 77.94228634059959404, -9.999999999999998224 ) ) ;
#31971 = AXIS2_PLACEMENT_3D ( 'NONE', #12712, #21360, #27356 ) ;
#31972 = CARTESIAN_POINT ( 'NONE',  ( 36.99999662536855283, 60.62177826491078747, -9.999999999999998224 ) ) ;
#31973 = CARTESIAN_POINT ( 'NONE',  ( 54.99999662536846046, -43.30127018922200222, -9.999999999999998224 ) ) ;
#31974 = EDGE_CURVE ( 'NONE', #35726, #36154, #938, .T. ) ;
#31975 = ORIENTED_EDGE ( 'NONE', *, *, #18408, .F. ) ;
#31976 = AXIS2_PLACEMENT_3D ( 'NONE', #15189, #24015, #26622 ) ;
#31977 = ORIENTED_EDGE ( 'NONE', *, *, #14238, .F. ) ;
#31978 = ORIENTED_EDGE ( 'NONE', *, *, #11486, .T. ) ;
#31979 = EDGE_CURVE ( 'NONE', #10472, #17978, #11042, .T. ) ;
#31980 = DIRECTION ( 'NONE',  ( 1.000000000000000000, 0.000000000000000000, 0.000000000000000000 ) ) ;
#31981 = CIRCLE ( 'NONE', #15255, 3.500000000000003109 ) ;
#31982 = AXIS2_PLACEMENT_3D ( 'NONE', #12890, #21709, #2208 ) ;
#31983 = CARTESIAN_POINT ( 'NONE',  ( 71.99999662536838230, -51.96152422706639840, -5.000000000000000000 ) ) ;
#31984 = EDGE_CURVE ( 'NONE', #7436, #7675, #7464, .T. ) ;
#31985 = AXIS2_PLACEMENT_3D ( 'NONE', #10416, #30492, #4817 ) ;
#31986 = CARTESIAN_POINT ( 'NONE',  ( -10.00000337463128730, 69.28203230275516944, 12.50000000000000000 ) ) ;
#31987 = CARTESIAN_POINT ( 'NONE',  ( -107.2742747693529566, -47.50000423952285900, 32.50001250000000397 ) ) ;
#31988 = CARTESIAN_POINT ( 'NONE',  ( -72.00000337463100664, -2.404119930384582903E-14, -5.000000000000000000 ) ) ;
#31989 = CARTESIAN_POINT ( 'NONE',  ( -37.50000000000000000, -103.4105893997321743, 27.50000000000000000 ) ) ;
#31990 = ORIENTED_EDGE ( 'NONE', *, *, #19162, .T. ) ;
#31991 = ORIENTED_EDGE ( 'NONE', *, *, #2709, .T. ) ;
#31992 = DIRECTION ( 'NONE',  ( 0.000000000000000000, 0.000000000000000000, 1.000000000000000000 ) ) ;
#31993 = AXIS2_PLACEMENT_3D ( 'NONE', #23259, #11987, #9009 ) ;
#31994 = CARTESIAN_POINT ( 'NONE',  ( -2.448772250512182280E-15, 99.94802294027086020, 27.49999999999999645 ) ) ;
#31995 = VECTOR ( 'NONE', #1943, 1000.000000000000000 ) ;
#31996 = CARTESIAN_POINT ( 'NONE',  ( 62.97617850287784336, 4.279621169095339184, -49.86561046011506448 ) ) ;
#31997 = EDGE_LOOP ( 'NONE', ( #4922, #25463, #13491, #25862 ) ) ;
#31998 = VECTOR ( 'NONE', #17238, 1000.000000000000000 ) ;
#31999 = EDGE_CURVE ( 'NONE', #14157, #27148, #33001, .T. ) ;
#32000 = FACE_BOUND ( 'NONE', #19996, .T. ) ;
#32001 = ORIENTED_EDGE ( 'NONE', *, *, #7736, .F. ) ;
#32002 = ORIENTED_EDGE ( 'NONE', *, *, #27653, .T. ) ;
#32003 = FACE_OUTER_BOUND ( 'NONE', #3269, .T. ) ;
#32004 = EDGE_LOOP ( 'NONE', ( #19183, #12433, #13787, #16723 ) ) ;
#32005 =( NAMED_UNIT ( * ) PLANE_ANGLE_UNIT ( ) SI_UNIT ( $, .RADIAN. ) );
#32006 = AXIS2_PLACEMENT_3D ( 'NONE', #30103, #1808, #4429 ) ;
#32007 = EDGE_CURVE ( 'NONE', #9234, #30623, #16314, .T. ) ;
#32008 = CIRCLE ( 'NONE', #15881, 27.00000000000001421 ) ;
#32009 = CARTESIAN_POINT ( 'NONE',  ( 64.99999662536839651, -43.30127018922199511, -5.000000000000000000 ) ) ;
#32010 = DIRECTION ( 'NONE',  ( 1.000000000000000000, 0.000000000000000000, 0.000000000000000000 ) ) ;
#32011 = DIRECTION ( 'NONE',  ( 1.000000000000000000, 0.000000000000000000, 0.000000000000000000 ) ) ;
#32012 = EDGE_CURVE ( 'NONE', #21341, #29683, #17040, .T. ) ;
#32013 = ORIENTED_EDGE ( 'NONE', *, *, #22, .T. ) ;
#32014 = ORIENTED_EDGE ( 'NONE', *, *, #14301, .T. ) ;
#32015 = EDGE_LOOP ( 'NONE', ( #23844, #9355 ) ) ;
#32016 = ORIENTED_EDGE ( 'NONE', *, *, #35454, .F. ) ;
#32017 = VERTEX_POINT ( 'NONE', #15750 ) ;
#32019 = DIRECTION ( 'NONE',  ( 1.000000000000000000, 0.000000000000000000, 0.000000000000000000 ) ) ;
#32018 = AXIS2_PLACEMENT_3D ( 'NONE', #13369, #12806, #16382 ) ;
#32020 = CARTESIAN_POINT ( 'NONE',  ( 51.99999662536847467, 69.28203230275516944, -9.999999999999998224 ) ) ;
#32021 = ORIENTED_EDGE ( 'NONE', *, *, #7849, .T. ) ;
#32022 = CIRCLE ( 'NONE', #12881, 95.00000000000000000 ) ;
#32023 = DIRECTION ( 'NONE',  ( 1.000000000000000000, 0.000000000000000000, 0.000000000000000000 ) ) ;
#32024 = CARTESIAN_POINT ( 'NONE',  ( 107.1113515669819236, 50.40365827702301260, 32.50000000000000711 ) ) ;
#32025 = LINE ( 'NONE', #20431, #23143 ) ;
#32026 = AXIS2_PLACEMENT_3D ( 'NONE', #11629, #31168, #5853 ) ;
#32027 = ORIENTED_EDGE ( 'NONE', *, *, #34134, .F. ) ;
#32028 = AXIS2_PLACEMENT_3D ( 'NONE', #17542, #19995, #5749 ) ;
#32029 = CYLINDRICAL_SURFACE ( 'NONE', #24233, 1.999999999999998224 ) ;
#32030 = CARTESIAN_POINT ( 'NONE',  ( 71.99999662536841072, 51.96152422706640550, 17.49999999999999645 ) ) ;
#32031 = ADVANCED_FACE ( 'NONE', ( #4502 ), #15940, .F. ) ;
#32032 = CARTESIAN_POINT ( 'NONE',  ( -70.80619744049063513, -84.18124734178186941, 27.50000000000000000 ) ) ;
#32033 = ORIENTED_EDGE ( 'NONE', *, *, #18304, .T. ) ;
#32034 = DIRECTION ( 'NONE',  ( 0.000000000000000000, 0.000000000000000000, 1.000000000000000000 ) ) ;
#32035 = FACE_OUTER_BOUND ( 'NONE', #3812, .T. ) ;
#32036 = AXIS2_PLACEMENT_3D ( 'NONE', #20942, #24122, #6687 ) ;
#32037 = ORIENTED_EDGE ( 'NONE', *, *, #24793, .T. ) ;
#32038 = CIRCLE ( 'NONE', #9904, 2.000000000000001776 ) ;
#32039 = ORIENTED_EDGE ( 'NONE', *, *, #18401, .F. ) ;
#32040 = CYLINDRICAL_SURFACE ( 'NONE', #29610, 3.000000000000000000 ) ;
#32041 = DIRECTION ( 'NONE',  ( 1.000000000000000000, 0.000000000000000000, 0.000000000000000000 ) ) ;
#32042 = CARTESIAN_POINT ( 'NONE',  ( -52.39915983220772233, -35.19434990244957362, 12.49999999999999822 ) ) ;
#32043 = DIRECTION ( 'NONE',  ( 1.000000000000000000, 0.000000000000000000, 0.000000000000000000 ) ) ;
#32044 = VERTEX_POINT ( 'NONE', #24186 ) ;
#32045 = CARTESIAN_POINT ( 'NONE',  ( 67.99999662536838230, -3.224517592124143893E-15, 17.49999999999999645 ) ) ;
#32046 = DIRECTION ( 'NONE',  ( 1.000000000000000000, 0.000000000000000000, -0.000000000000000000 ) ) ;
#32047 = CARTESIAN_POINT ( 'NONE',  ( 4.182066831946704255, -3.358985280702828646, -5.826062401966622950 ) ) ;
#32048 = EDGE_CURVE ( 'NONE', #23693, #32859, #15245, .T. ) ;
#32049 = AXIS2_PLACEMENT_3D ( 'NONE', #36638, #5504, #8499 ) ;
#32050 = ORIENTED_EDGE ( 'NONE', *, *, #2954, .T. ) ;
#32051 = EDGE_CURVE ( 'NONE', #12512, #31658, #282, .T. ) ;
#32052 = AXIS2_PLACEMENT_3D ( 'NONE', #13514, #33775, #33602 ) ;
#32053 = CARTESIAN_POINT ( 'NONE',  ( 5.236872748402764621, 8.442024233997350580E-14, -4.057689166958447835 ) ) ;
#32054 = ORIENTED_EDGE ( 'NONE', *, *, #33699, .F. ) ;
#32055 = CIRCLE ( 'NONE', #11122, 6.000000000000005329 ) ;
#32056 = CIRCLE ( 'NONE', #33295, 2.000000000000001776 ) ;
#32057 = AXIS2_PLACEMENT_3D ( 'NONE', #27650, #10235, #21662 ) ;
#32058 = LINE ( 'NONE', #21196, #1333 ) ;
#32059 = EDGE_CURVE ( 'NONE', #20361, #9651, #26031, .T. ) ;
#32060 = VECTOR ( 'NONE', #7779, 1000.000000000000000 ) ;
#32061 = DIRECTION ( 'NONE',  ( 0.000000000000000000, 0.000000000000000000, 1.000000000000000000 ) ) ;
#32062 = FACE_OUTER_BOUND ( 'NONE', #8251, .T. ) ;
#32063 = EDGE_LOOP ( 'NONE', ( #134, #23475 ) ) ;
#32064 = ORIENTED_EDGE ( 'NONE', *, *, #10096, .T. ) ;
#32065 = EDGE_CURVE ( 'NONE', #34930, #9326, #12925, .T. ) ;
#32066 = AXIS2_PLACEMENT_3D ( 'NONE', #24879, #33870, #36319 ) ;
#32067 = DIRECTION ( 'NONE',  ( -0.5000000000000045519, 0.8660254037844360431, 0.000000000000000000 ) ) ;
#32068 = EDGE_CURVE ( 'NONE', #4038, #5699, #36015, .T. ) ;
#32069 = CARTESIAN_POINT ( 'NONE',  ( -103.1837242358309510, 33.77655254667255491, 32.50000000000000000 ) ) ;
#32070 = VECTOR ( 'NONE', #31512, 1000.000000000000000 ) ;
#32071 = CARTESIAN_POINT ( 'NONE',  ( 111.8061974404897825, -19.22934205795014151, 32.50000000000000000 ) ) ;
#32072 = ORIENTED_EDGE ( 'NONE', *, *, #25934, .F. ) ;
#32073 = DIRECTION ( 'NONE',  ( -1.000000000000000000, -0.000000000000000000, -0.000000000000000000 ) ) ;
#32074 = FACE_BOUND ( 'NONE', #20384, .T. ) ;
#32075 = DIRECTION ( 'NONE',  ( 1.000000000000000000, 0.000000000000000000, 0.000000000000000000 ) ) ;
#32076 = CARTESIAN_POINT ( 'NONE',  ( -6.069707180676227632E-15, 5.773502691896268857, -3.984345921091771547 ) ) ;
#32077 = DIRECTION ( 'NONE',  ( 1.000000000000000000, 0.000000000000000000, 0.000000000000000000 ) ) ;
#32078 = EDGE_CURVE ( 'NONE', #18782, #32494, #25426, .T. ) ;
#32079 = ORIENTED_EDGE ( 'NONE', *, *, #23414, .T. ) ;
#32080 = CARTESIAN_POINT ( 'NONE',  ( -98.28784258493107018, -106.7731239591678616, 27.50000000000000000 ) ) ;
#32081 = CIRCLE ( 'NONE', #36293, 2.000000000000000000 ) ;
#32082 = EDGE_CURVE ( 'NONE', #17074, #6836, #6306, .T. ) ;
#32083 = EDGE_CURVE ( 'NONE', #30600, #1512, #11676, .T. ) ;
#32084 = AXIS2_PLACEMENT_3D ( 'NONE', #5287, #31489, #36960 ) ;
#32085 = SURFACE_STYLE_FILL_AREA ( #20653 ) ;
#32086 = ORIENTED_EDGE ( 'NONE', *, *, #15598, .F. ) ;
#32087 = EDGE_CURVE ( 'NONE', #16622, #26755, #6283, .T. ) ;
#32088 = DIRECTION ( 'NONE',  ( -1.000000000000000000, 0.000000000000000000, 0.000000000000000000 ) ) ;
#32089 = COLOUR_RGB ( '', 0.09019608, 0.27058824, 0.51372549) ;
#32090 = FACE_BOUND ( 'NONE', #2010, .T. ) ;
#32091 = LINE ( 'NONE', #29297, #10203 ) ;
#32092 = CIRCLE ( 'NONE', #3982, 2.000000000000001776 ) ;
#32093 = VECTOR ( 'NONE', #1760, 1000.000000000000000 ) ;
#32094 = EDGE_LOOP ( 'NONE', ( #27931, #37104 ) ) ;
#32095 = AXIS2_PLACEMENT_3D ( 'NONE', #24093, #35539, #33265 ) ;
#32096 = ORIENTED_EDGE ( 'NONE', *, *, #33790, .F. ) ;
#32097 = AXIS2_PLACEMENT_3D ( 'NONE', #28267, #33723, #18915 ) ;
#32098 = ORIENTED_EDGE ( 'NONE', *, *, #23714, .T. ) ;
#32099 = DIRECTION ( 'NONE',  ( 1.000000000000000000, 0.000000000000000000, 0.000000000000000000 ) ) ;
#32100 = CYLINDRICAL_SURFACE ( 'NONE', #13987, 2.000000000000001776 ) ;
#32101 = DIRECTION ( 'NONE',  ( 0.000000000000000000, 0.000000000000000000, -1.000000000000000000 ) ) ;
#32102 = VERTEX_POINT ( 'NONE', #1491 ) ;
#32103 = ORIENTED_EDGE ( 'NONE', *, *, #22851, .T. ) ;
#32104 = ORIENTED_EDGE ( 'NONE', *, *, #6917, .T. ) ;
#32105 = CYLINDRICAL_SURFACE ( 'NONE', #35293, 2.000000000000001776 ) ;
#32106 = ORIENTED_EDGE ( 'NONE', *, *, #30860, .T. ) ;
#32107 = CYLINDRICAL_SURFACE ( 'NONE', #4214, 150.0000000000000284 ) ;
#32108 = ORIENTED_EDGE ( 'NONE', *, *, #30212, .T. ) ;
#32109 = DIRECTION ( 'NONE',  ( -0.5000000000000101030, -0.8660254037844329345, 0.000000000000000000 ) ) ;
#32110 = ORIENTED_EDGE ( 'NONE', *, *, #19516, .F. ) ;
#32111 = AXIS2_PLACEMENT_3D ( 'NONE', #6218, #29282, #17478 ) ;
#32112 = VERTEX_POINT ( 'NONE', #21933 ) ;
#32113 = DIRECTION ( 'NONE',  ( -0.000000000000000000, -1.000000000000000000, -0.000000000000000000 ) ) ;
#32114 = CARTESIAN_POINT ( 'NONE',  ( 1.552113441248130554, -4.877389578778822177, -0.7348938709837993244 ) ) ;
#32115 = AXIS2_PLACEMENT_3D ( 'NONE', #9565, #20258, #29038 ) ;
#32116 = CYLINDRICAL_SURFACE ( 'NONE', #33844, 3.499999999999989342 ) ;
#32117 = ORIENTED_EDGE ( 'NONE', *, *, #30332, .T. ) ;
#32118 = VERTEX_POINT ( 'NONE', #35833 ) ;
#32119 = AXIS2_PLACEMENT_3D ( 'NONE', #37088, #34271, #19457 ) ;
#32120 = DIRECTION ( 'NONE',  ( 1.000000000000000000, 0.000000000000000000, 0.000000000000000000 ) ) ;
#32121 = CIRCLE ( 'NONE', #33945, 2.000000000000000000 ) ;
#32122 = VECTOR ( 'NONE', #25424, 1000.000000000000000 ) ;
#32123 = VECTOR ( 'NONE', #18985, 1000.000000000000000 ) ;
#32124 = CARTESIAN_POINT ( 'NONE',  ( 82.99999662536832545, 8.660254037844394404, -9.999999999999998224 ) ) ;
#32125 = CARTESIAN_POINT ( 'NONE',  ( -5.000000000000000888, 1.087997039530374854, -3.720971761088881280 ) ) ;
#32126 = AXIS2_PLACEMENT_3D ( 'NONE', #26752, #15874, #20951 ) ;
#32127 = EDGE_LOOP ( 'NONE', ( #12337, #3382, #22321, #18593 ) ) ;
#32128 = CYLINDRICAL_SURFACE ( 'NONE', #22524, 2.000000000000001776 ) ;
#32129 = DIRECTION ( 'NONE',  ( -0.000000000000000000, -0.000000000000000000, -1.000000000000000000 ) ) ;
#32130 = ORIENTED_EDGE ( 'NONE', *, *, #31855, .T. ) ;
#32131 = CARTESIAN_POINT ( 'NONE',  ( 3.000000000000000000, -1.467624384280027172, 2.542000000000001592 ) ) ;
#32132 = DIRECTION ( 'NONE',  ( 1.000000000000000000, 0.000000000000000000, 0.000000000000000000 ) ) ;
#32133 = DIRECTION ( 'NONE',  ( 0.000000000000000000, 0.000000000000000000, 1.000000000000000000 ) ) ;
#32134 = MANIFOLD_SOLID_BREP ( 'CirPattern3', #11775 ) ;
#32135 = FACE_OUTER_BOUND ( 'NONE', #14804, .T. ) ;
#32136 = AXIS2_PLACEMENT_3D ( 'NONE', #20089, #9028, #31872 ) ;
#32137 = EDGE_CURVE ( 'NONE', #6269, #30055, #23062, .T. ) ;
#32138 = DIRECTION ( 'NONE',  ( -0.000000000000000000, -0.000000000000000000, 1.000000000000000000 ) ) ;
#32139 = ADVANCED_FACE ( 'NONE', ( #36921, #2437, #22680 ), #20230, .F. ) ;
#32140 = ADVANCED_FACE ( 'NONE', ( #30913 ), #19857, .F. ) ;
#32141 = FACE_OUTER_BOUND ( 'NONE', #31303, .T. ) ;
#32142 = VERTEX_POINT ( 'NONE', #5988 ) ;
#32143 = CARTESIAN_POINT ( 'NONE',  ( 42.99999662536850309, -60.62177826491080168, -9.999999999999998224 ) ) ;
#32144 = CARTESIAN_POINT ( 'NONE',  ( -19.31922176934808633, 76.99660315353983719, 27.49999999999999645 ) ) ;
#32145 = FACE_OUTER_BOUND ( 'NONE', #15963, .T. ) ;
#32146 = CIRCLE ( 'NONE', #11196, 17.55872235085559652 ) ;
#32147 = VECTOR ( 'NONE', #36955, 1000.000000000000000 ) ;
#32148 = ORIENTED_EDGE ( 'NONE', *, *, #17644, .T. ) ;
#32149 = ORIENTED_EDGE ( 'NONE', *, *, #19898, .F. ) ;
#32150 = ORIENTED_EDGE ( 'NONE', *, *, #22464, .F. ) ;
#32151 = AXIS2_PLACEMENT_3D ( 'NONE', #6660, #26908, #29153 ) ;
#32152 = FACE_OUTER_BOUND ( 'NONE', #4818, .T. ) ;
#32153 = DIRECTION ( 'NONE',  ( 0.000000000000000000, 0.000000000000000000, 1.000000000000000000 ) ) ;
#32154 = DIRECTION ( 'NONE',  ( 0.000000000000000000, 0.000000000000000000, 1.000000000000000000 ) ) ;
#32155 = CIRCLE ( 'NONE', #12998, 2.000000000000001776 ) ;
#32156 = CIRCLE ( 'NONE', #14792, 2.541999999999999815 ) ;
#32157 = DIRECTION ( 'NONE',  ( 1.000000000000000000, 0.000000000000000000, 0.000000000000000000 ) ) ;
#32158 = CYLINDRICAL_SURFACE ( 'NONE', #27880, 8.500000000000003553 ) ;
#32159 = VERTEX_POINT ( 'NONE', #28466 ) ;
#32160 = CARTESIAN_POINT ( 'NONE',  ( -63.00000337463104927, -25.98076211353322051, -9.999999999999998224 ) ) ;
#32161 = ORIENTED_EDGE ( 'NONE', *, *, #18319, .F. ) ;
#32162 = FACE_BOUND ( 'NONE', #7144, .T. ) ;
#32163 = CIRCLE ( 'NONE', #20214, 3.000000000000000888 ) ;
#32164 = EDGE_CURVE ( 'NONE', #36526, #859, #34127, .T. ) ;
#32165 = AXIS2_PLACEMENT_3D ( 'NONE', #29829, #4154, #24595 ) ;
#32166 = LINE ( 'NONE', #6297, #5372 ) ;
#32167 = AXIS2_PLACEMENT_3D ( 'NONE', #3446, #28924, #14677 ) ;
#32168 = CYLINDRICAL_SURFACE ( 'NONE', #31065, 2.000000000000001776 ) ;
#32169 = ORIENTED_EDGE ( 'NONE', *, *, #16466, .F. ) ;
#32170 = DIRECTION ( 'NONE',  ( 1.000000000000000000, 0.000000000000000000, 0.000000000000000000 ) ) ;
#32171 = AXIS2_PLACEMENT_3D ( 'NONE', #10571, #14109, #22011 ) ;
#32172 = DIRECTION ( 'NONE',  ( 0.7813797561979389794, -0.6240558281148007591, 0.000000000000000000 ) ) ;
#32173 = CIRCLE ( 'NONE', #30983, 2.000000000000001776 ) ;
#32174 = DIRECTION ( 'NONE',  ( 0.000000000000000000, 0.000000000000000000, 1.000000000000000000 ) ) ;
#32175 = CIRCLE ( 'NONE', #32811, 8.500000000000007105 ) ;
#32176 = CARTESIAN_POINT ( 'NONE',  ( 65.00000000000000000, 0.000000000000000000, 12.49999999999999822 ) ) ;
#32177 = DIRECTION ( 'NONE',  ( 0.000000000000000000, 0.000000000000000000, -1.000000000000000000 ) ) ;
#32178 = ORIENTED_EDGE ( 'NONE', *, *, #3221, .T. ) ;
#32179 = CARTESIAN_POINT ( 'NONE',  ( -88.00000337463090716, -1.040834085586084257E-14, 17.49999999999999645 ) ) ;
#32180 = DIRECTION ( 'NONE',  ( -1.000000000000000000, 0.000000000000000000, 0.000000000000000000 ) ) ;
#32181 = DIRECTION ( 'NONE',  ( 0.000000000000000000, 0.000000000000000000, 1.000000000000000000 ) ) ;
#32182 = AXIS2_PLACEMENT_3D ( 'NONE', #19229, #1400, #30641 ) ;
#32183 = VERTEX_POINT ( 'NONE', #2246 ) ;
#32184 = AXIS2_PLACEMENT_3D ( 'NONE', #31033, #5713, #25235 ) ;
#32185 = EDGE_LOOP ( 'NONE', ( #29254, #2184 ) ) ;
#32186 = EDGE_CURVE ( 'NONE', #23515, #19701, #27378, .T. ) ;
#32187 = EDGE_LOOP ( 'NONE', ( #14724, #7336, #33048, #26029, #14084, #2308, #18918, #1291, #3546, #19275 ) ) ;
#32188 = DIRECTION ( 'NONE',  ( 0.000000000000000000, 0.000000000000000000, 1.000000000000000000 ) ) ;
#32189 = CIRCLE ( 'NONE', #30413, 2.000000000000001776 ) ;
#32190 = FACE_OUTER_BOUND ( 'NONE', #19942, .T. ) ;
#32191 = DIRECTION ( 'NONE',  ( 1.000000000000000000, 0.000000000000000000, 0.000000000000000000 ) ) ;
#32192 = ORIENTED_EDGE ( 'NONE', *, *, #36022, .F. ) ;
#32193 = AXIS2_PLACEMENT_3D ( 'NONE', #26642, #20632, #18026 ) ;
#32194 = CARTESIAN_POINT ( 'NONE',  ( 16.99999662536859901, 77.94228634059957983, -9.999999999999998224 ) ) ;
#32195 = DIRECTION ( 'NONE',  ( 0.000000000000000000, 0.000000000000000000, 1.000000000000000000 ) ) ;
#32196 = CIRCLE ( 'NONE', #33400, 3.499999999999991562 ) ;
#32197 = AXIS2_PLACEMENT_3D ( 'NONE', #32641, #6966, #18417 ) ;
#32198 = B_SPLINE_CURVE_WITH_KNOTS ( 'NONE', 3,
 ( #10825, #30681, #7999, #16635, #10637, #27864, #2562, #36136, #11177, #36690, #7640, #19438, #21876, #1997, #25430, #5001, #22257, #24703, #22081, #16089 ),
 .UNSPECIFIED., .F., .F.,
 ( 4, 2, 2, 2, 2, 2, 2, 2, 2, 4 ),
 ( 2.781148944365360171E-07, 0.0008372784139787578517, 0.001674278713063079033, 0.002511279012147400649, 0.003348279311231721830, 0.003766779460773882204, 0.004185279610316042578, 0.005022279909400362459, 0.005859280208484684074, 0.006696280507569004822 ),
 .UNSPECIFIED. ) ;
#32199 = DIRECTION ( 'NONE',  ( 0.000000000000000000, 0.000000000000000000, 1.000000000000000000 ) ) ;
#32200 = ORIENTED_EDGE ( 'NONE', *, *, #35718, .F. ) ;
#32201 = CIRCLE ( 'NONE', #7064, 1.999999999999998224 ) ;
#32202 = ORIENTED_EDGE ( 'NONE', *, *, #17646, .F. ) ;
#32203 = CARTESIAN_POINT ( 'NONE',  ( -68.00000337463102085, -34.64101615137762025, -9.999999999999998224 ) ) ;
#32204 = AXIS2_PLACEMENT_3D ( 'NONE', #34514, #33779, #8090 ) ;
#32205 = EDGE_CURVE ( 'NONE', #29268, #33506, #10487, .T. ) ;
#32206 = DIRECTION ( 'NONE',  ( 0.000000000000000000, 0.000000000000000000, 1.000000000000000000 ) ) ;
#32207 = ORIENTED_EDGE ( 'NONE', *, *, #29228, .F. ) ;
#32208 = DIRECTION ( 'NONE',  ( -1.000000000000000000, 1.490577208987477824E-14, 0.000000000000000000 ) ) ;
#32209 = ORIENTED_EDGE ( 'NONE', *, *, #26741, .F. ) ;
#32210 = EDGE_CURVE ( 'NONE', #19159, #26265, #36569, .T. ) ;
#32211 = CIRCLE ( 'NONE', #20235, 2.541999999999999815 ) ;
#32212 = FACE_BOUND ( 'NONE', #34961, .T. ) ;
#32213 = VERTEX_POINT ( 'NONE', #31112 ) ;
#32214 = EDGE_LOOP ( 'NONE', ( #15500, #37087, #9746, #7320 ) ) ;
#32215 = ADVANCED_FACE ( 'NONE', ( #25483 ), #5799, .F. ) ;
#32216 = DIRECTION ( 'NONE',  ( 0.000000000000000000, 0.000000000000000000, 1.000000000000000000 ) ) ;
#32217 = EDGE_LOOP ( 'NONE', ( #36643, #21440 ) ) ;
#32218 = VECTOR ( 'NONE', #11397, 1000.000000000000000 ) ;
#32219 = DIRECTION ( 'NONE',  ( 0.000000000000000000, 0.000000000000000000, -1.000000000000000000 ) ) ;
#32220 = EDGE_CURVE ( 'NONE', #31117, #27431, #14065, .T. ) ;
#32221 = AXIS2_PLACEMENT_3D ( 'NONE', #16880, #2062, #25156 ) ;
#32222 = DIRECTION ( 'NONE',  ( 0.000000000000000000, 0.000000000000000000, -1.000000000000000000 ) ) ;
#32223 = CARTESIAN_POINT ( 'NONE',  ( 16.99999662536859901, 77.94228634059957983, 17.49999999999999645 ) ) ;
#32224 = ORIENTED_EDGE ( 'NONE', *, *, #26233, .F. ) ;
#32225 = ORIENTED_EDGE ( 'NONE', *, *, #17911, .F. ) ;
#32226 = CIRCLE ( 'NONE', #30450, 2.000000000000001776 ) ;
#32227 = ORIENTED_EDGE ( 'NONE', *, *, #28204, .T. ) ;
#32228 = CIRCLE ( 'NONE', #26242, 2.000000000000001776 ) ;
#32229 = EDGE_LOOP ( 'NONE', ( #12788, #13725 ) ) ;
#32230 = ORIENTED_EDGE ( 'NONE', *, *, #12830, .T. ) ;
#32231 = CARTESIAN_POINT ( 'NONE',  ( -72.00000337463102085, -51.96152422706641971, 17.49999999999999645 ) ) ;
#32232 = EDGE_CURVE ( 'NONE', #36602, #29314, #8785, .T. ) ;
#32233 = CYLINDRICAL_SURFACE ( 'NONE', #10215, 2.000000000000001776 ) ;
#32234 = ORIENTED_EDGE ( 'NONE', *, *, #34671, .F. ) ;
#32235 = DIRECTION ( 'NONE',  ( 1.000000000000000000, 0.000000000000000000, 0.000000000000000000 ) ) ;
#32236 = CARTESIAN_POINT ( 'NONE',  ( 0.000000000000000000, 0.000000000000000000, 27.50000000000000000 ) ) ;
#32237 = DIRECTION ( 'NONE',  ( 0.000000000000000000, 0.000000000000000000, 1.000000000000000000 ) ) ;
#32238 = ORIENTED_EDGE ( 'NONE', *, *, #36236, .F. ) ;
#32239 = DIRECTION ( 'NONE',  ( 1.000000000000000000, 0.000000000000000000, 0.000000000000000000 ) ) ;
#32240 =( BOUNDED_SURFACE ( )  B_SPLINE_SURFACE ( 3, 2, ( 
 ( #8468, #19537, #30772 ),
 ( #10903, #11453, #2479 ),
 ( #25345, #36610, #33984 ),
 ( #36779, #19184, #31322 ),
 ( #17082, #22900, #5301 ),
 ( #14077, #22343, #16737 ) ),
 .UNSPECIFIED., .F., .F., .F. ) 
 B_SPLINE_SURFACE_WITH_KNOTS ( ( 4, 2, 4 ),
 ( 3, 3 ),
 ( 0.002450104044831661210, 0.005591829551853644796, 0.008733555058875628815 ),
 ( 0.000000000000000000, 1.000000000000000000 ),
 .UNSPECIFIED. ) 
 GEOMETRIC_REPRESENTATION_ITEM ( )  RATIONAL_B_SPLINE_SURFACE ( (
 ( 1.000000000000000000, 0.8047731410850402778, 1.000000000000000000),
 ( 1.000000000000000000, 0.8125552299159768399, 1.000000000000000000),
 ( 1.000000000000000000, 0.8191520442885167341, 1.000000000000000000),
 ( 1.000000000000000000, 0.8191520442894577592, 1.000000000000000000),
 ( 1.000000000000000000, 0.8125552299152696278, 1.000000000000000000),
 ( 1.000000000000000000, 0.8047731410850398337, 1.000000000000000000) ) ) 
 REPRESENTATION_ITEM ( '' )  SURFACE ( )  );
#32241 = AXIS2_PLACEMENT_3D ( 'NONE', #5669, #28541, #214 ) ;
#32242 = CARTESIAN_POINT ( 'NONE',  ( 32.99999662536855283, -60.62177826491080168, 12.50000000000000000 ) ) ;
#32243 = CARTESIAN_POINT ( 'NONE',  ( -37.00000337463116296, 60.62177826491077326, 17.49999999999999645 ) ) ;
#32244 = VERTEX_POINT ( 'NONE', #22304 ) ;
#32245 = LINE ( 'NONE', #9572, #501 ) ;
#32246 = CARTESIAN_POINT ( 'NONE',  ( -56.13646009116099123, 70.47608876694653190, 12.49999999999999822 ) ) ;
#32247 = ORIENTED_EDGE ( 'NONE', *, *, #31039, .T. ) ;
#32248 = ADVANCED_FACE ( 'NONE', ( #8046 ), #14231, .F. ) ;
#32249 = ORIENTED_EDGE ( 'NONE', *, *, #12582, .T. ) ;
#32250 = CARTESIAN_POINT ( 'NONE',  ( -63.00000337463104927, -25.98076211353322051, -9.999999999999998224 ) ) ;
#32251 = CIRCLE ( 'NONE', #12500, 3.000000000000001332 ) ;
#32252 = EDGE_CURVE ( 'NONE', #17975, #25264, #11036, .T. ) ;
#32253 = DIRECTION ( 'NONE',  ( 1.000000000000000000, 0.000000000000000000, 0.000000000000000000 ) ) ;
#32254 = DIRECTION ( 'NONE',  ( 1.000000000000000000, 0.000000000000000000, 0.000000000000000000 ) ) ;
#32255 = CARTESIAN_POINT ( 'NONE',  ( 42.99999662536848888, 60.62177826491077326, -9.999999999999998224 ) ) ;
#32256 = ORIENTED_EDGE ( 'NONE', *, *, #11737, .F. ) ;
#32257 = CIRCLE ( 'NONE', #32861, 1.999999999999998224 ) ;
#32258 = EDGE_CURVE ( 'NONE', #14036, #5415, #7492, .T. ) ;
#32259 = DIRECTION ( 'NONE',  ( -1.000000000000000000, 0.000000000000000000, 0.000000000000000000 ) ) ;
#32260 = DIRECTION ( 'NONE',  ( 0.000000000000000000, 0.000000000000000000, 1.000000000000000000 ) ) ;
#32261 = VERTEX_POINT ( 'NONE', #28285 ) ;
#32262 = CIRCLE ( 'NONE', #20904, 2.000000000000001776 ) ;
#32263 = EDGE_CURVE ( 'NONE', #36034, #35959, #25855, .T. ) ;
#32264 = CARTESIAN_POINT ( 'NONE',  ( 74.99999662536836809, 43.30127018922198801, -5.000000000000000000 ) ) ;
#32265 = ORIENTED_EDGE ( 'NONE', *, *, #18601, .T. ) ;
#32266 = CIRCLE ( 'NONE', #18508, 2.000000000000001776 ) ;
#32267 = CYLINDRICAL_SURFACE ( 'NONE', #18715, 2.000000000000001776 ) ;
#32268 = LINE ( 'NONE', #20835, #30188 ) ;
#32269 = AXIS2_PLACEMENT_3D ( 'NONE', #19831, #20192, #5406 ) ;
#32270 = ADVANCED_FACE ( 'NONE', ( #145 ), #20029, .F. ) ;
#32271 = DIRECTION ( 'NONE',  ( 1.000000000000000000, 0.000000000000000000, 0.000000000000000000 ) ) ;
#32272 = EDGE_LOOP ( 'NONE', ( #19533, #22066, #3769, #36506 ) ) ;
#32273 = VECTOR ( 'NONE', #658, 1000.000000000000000 ) ;
#32274 = EDGE_LOOP ( 'NONE', ( #3589, #32933, #12663, #30409 ) ) ;
#32275 = CARTESIAN_POINT ( 'NONE',  ( -83.47442710120355969, 31.09745072740822991, 12.49999999999999645 ) ) ;
#32276 = DIRECTION ( 'NONE',  ( 1.000000000000000000, 0.000000000000000000, 0.000000000000000000 ) ) ;
#32277 = ORIENTED_EDGE ( 'NONE', *, *, #14919, .F. ) ;
#32278 = CYLINDRICAL_SURFACE ( 'NONE', #9968, 2.000000000000000000 ) ;
#32279 = AXIS2_PLACEMENT_3D ( 'NONE', #25243, #16811, #36671 ) ;
#32280 = FACE_BOUND ( 'NONE', #3801, .T. ) ;
#32281 = CIRCLE ( 'NONE', #16147, 2.000000000000001776 ) ;
#32282 = CYLINDRICAL_SURFACE ( 'NONE', #8842, 3.000000000000005773 ) ;
#32283 = CARTESIAN_POINT ( 'NONE',  ( 3.000000000000000000, -1.467624384280027172, 2.542000000000001592 ) ) ;
#32284 = DIRECTION ( 'NONE',  ( 0.000000000000000000, 0.000000000000000000, -1.000000000000000000 ) ) ;
#32285 = ORIENTED_EDGE ( 'NONE', *, *, #5405, .T. ) ;
#32286 = DIRECTION ( 'NONE',  ( 0.000000000000000000, 0.000000000000000000, 1.000000000000000000 ) ) ;
#32287 = EDGE_CURVE ( 'NONE', #30934, #19087, #26773, .T. ) ;
#32288 = CARTESIAN_POINT ( 'NONE',  ( 6.249999999999998224, 0.000000000000000000, 0.000000000000000000 ) ) ;
#32289 = VECTOR ( 'NONE', #30274, 1000.000000000000000 ) ;
#32290 = CYLINDRICAL_SURFACE ( 'NONE', #22982, 2.000000000000001776 ) ;
#32291 = EDGE_LOOP ( 'NONE', ( #21040, #36195, #6505 ) ) ;
#32292 = DIRECTION ( 'NONE',  ( 0.000000000000000000, 0.000000000000000000, -1.000000000000000000 ) ) ;
#32293 = DIRECTION ( 'NONE',  ( -0.000000000000000000, -0.000000000000000000, -1.000000000000000000 ) ) ;
#32294 = CARTESIAN_POINT ( 'NONE',  ( -27.78182860042817026, -56.67878100130359087, -4.999999999999997335 ) ) ;
#32295 = CIRCLE ( 'NONE', #16742, 2.000000000000000000 ) ;
#32296 = ORIENTED_EDGE ( 'NONE', *, *, #31424, .F. ) ;
#32297 = EDGE_CURVE ( 'NONE', #19079, #7505, #32636, .T. ) ;
#32298 = VERTEX_POINT ( 'NONE', #20403 ) ;
#32299 = VECTOR ( 'NONE', #14743, 1000.000000000000000 ) ;
#32300 = VERTEX_POINT ( 'NONE', #12119 ) ;
#32301 = EDGE_CURVE ( 'NONE', #14961, #13777, #36827, .T. ) ;
#32302 = DIRECTION ( 'NONE',  ( 0.000000000000000000, 0.000000000000000000, 1.000000000000000000 ) ) ;
#32303 = CYLINDRICAL_SURFACE ( 'NONE', #7417, 2.000000000000000000 ) ;
#32304 = EDGE_CURVE ( 'NONE', #24335, #3324, #4500, .T. ) ;
#32305 = DIRECTION ( 'NONE',  ( 0.000000000000000000, 0.000000000000000000, 1.000000000000000000 ) ) ;
#32306 = ORIENTED_EDGE ( 'NONE', *, *, #15587, .F. ) ;
#32307 = VERTEX_POINT ( 'NONE', #6333 ) ;
#32308 = CIRCLE ( 'NONE', #16161, 1.999999999999998224 ) ;
#32309 = ORIENTED_EDGE ( 'NONE', *, *, #19084, .T. ) ;
#32310 = DIRECTION ( 'NONE',  ( -1.000000000000000000, 0.000000000000000000, 0.000000000000000000 ) ) ;
#32311 = VERTEX_POINT ( 'NONE', #23227 ) ;
#32312 = CARTESIAN_POINT ( 'NONE',  ( -104.8061974404900241, -19.22934205794863516, 32.50000000000000000 ) ) ;
#32313 = VERTEX_POINT ( 'NONE', #29210 ) ;
#32314 = CIRCLE ( 'NONE', #15572, 2.000000000000001776 ) ;
#32315 = LINE ( 'NONE', #9243, #6961 ) ;
#32316 = ORIENTED_EDGE ( 'NONE', *, *, #4360, .F. ) ;
#32317 = EDGE_LOOP ( 'NONE', ( #32322, #6540 ) ) ;
#32318 = CARTESIAN_POINT ( 'NONE',  ( 64.99999662536839651, 60.62177826491078747, -9.999999999999998224 ) ) ;
#32319 = DIRECTION ( 'NONE',  ( 0.000000000000000000, 0.000000000000000000, -1.000000000000000000 ) ) ;
#32320 = EDGE_CURVE ( 'NONE', #11272, #7613, #3311, .T. ) ;
#32321 = DIRECTION ( 'NONE',  ( 1.000000000000000000, 0.000000000000000000, 0.000000000000000000 ) ) ;
#32322 = ORIENTED_EDGE ( 'NONE', *, *, #35551, .F. ) ;
#32323 = VERTEX_POINT ( 'NONE', #26577 ) ;
#32324 = CARTESIAN_POINT ( 'NONE',  ( 61.99999662536842493, -51.96152422706639840, -9.999999999999998224 ) ) ;
#32325 = FACE_OUTER_BOUND ( 'NONE', #30768, .T. ) ;
#32326 = DIRECTION ( 'NONE',  ( 1.000000000000000000, 0.000000000000000000, 0.000000000000000000 ) ) ;
#32327 = CARTESIAN_POINT ( 'NONE',  ( -5.244935714621999701, 2.071324742674405694, -4.180276246144004837 ) ) ;
#32328 = ORIENTED_EDGE ( 'NONE', *, *, #36892, .T. ) ;
#32329 = DIRECTION ( 'NONE',  ( 0.000000000000000000, 0.000000000000000000, 1.000000000000000000 ) ) ;
#32330 = CARTESIAN_POINT ( 'NONE',  ( 72.99999662536835388, -25.98076211353319565, 12.50000000000000000 ) ) ;
#32331 = ORIENTED_EDGE ( 'NONE', *, *, #3146, .F. ) ;
#32332 = AXIS2_PLACEMENT_3D ( 'NONE', #23867, #32464, #7348 ) ;
#32333 = CARTESIAN_POINT ( 'NONE',  ( -63.00000337463102085, 60.62177826491077326, -9.999999999999998224 ) ) ;
#32334 = DIRECTION ( 'NONE',  ( 1.000000000000000000, 0.000000000000000000, 0.000000000000000000 ) ) ;
#32335 = CIRCLE ( 'NONE', #11355, 2.000000000000001776 ) ;
#32336 = DIRECTION ( 'NONE',  ( 0.000000000000000000, 0.000000000000000000, 1.000000000000000000 ) ) ;
#32337 = DIRECTION ( 'NONE',  ( 0.000000000000000000, 0.000000000000000000, -1.000000000000000000 ) ) ;
#32338 = ADVANCED_FACE ( 'NONE', ( #6709 ), #26407, .T. ) ;
#32339 = CARTESIAN_POINT ( 'NONE',  ( 5.750000000000000000, 89.94802294027094547, -24.99999999999999645 ) ) ;
#32340 = CIRCLE ( 'NONE', #31739, 3.499999999999996003 ) ;
#32341 = CARTESIAN_POINT ( 'NONE',  ( 9.999996625368655856, -86.60254037844400443, -9.999999999999998224 ) ) ;
#32342 = ORIENTED_EDGE ( 'NONE', *, *, #13926, .T. ) ;
#32343 = ADVANCED_FACE ( 'NONE', ( #15330 ), #9329, .F. ) ;
#32344 = DIRECTION ( 'NONE',  ( 0.4999999999999919509, -0.8660254037844432595, 0.000000000000000000 ) ) ;
#32345 = CIRCLE ( 'NONE', #32943, 2.000000000000001776 ) ;
#32346 = DIRECTION ( 'NONE',  ( 0.000000000000000000, 0.000000000000000000, -1.000000000000000000 ) ) ;
#32347 = CARTESIAN_POINT ( 'NONE',  ( -25.00000337463120914, 77.94228634059957983, 12.50000000000000000 ) ) ;
#32348 = ORIENTED_EDGE ( 'NONE', *, *, #31625, .T. ) ;
#32349 = ADVANCED_FACE ( 'NONE', ( #12513 ), #35026, .F. ) ;
#32350 = EDGE_LOOP ( 'NONE', ( #5111, #31779 ) ) ;
#32351 = ORIENTED_EDGE ( 'NONE', *, *, #21361, .T. ) ;
#32352 = CARTESIAN_POINT ( 'NONE',  ( 24.99999662536857059, 77.94228634059957983, 12.50000000000000000 ) ) ;
#32353 = DIRECTION ( 'NONE',  ( 0.000000000000000000, 0.000000000000000000, 1.000000000000000000 ) ) ;
#32354 = AXIS2_PLACEMENT_3D ( 'NONE', #2431, #4880, #33569 ) ;
#32355 = EDGE_CURVE ( 'NONE', #16050, #32632, #31819, .T. ) ;
#32356 = DIRECTION ( 'NONE',  ( 1.000000000000000000, 0.000000000000000000, 0.000000000000000000 ) ) ;
#32357 = ADVANCED_FACE ( 'NONE', ( #6534 ), #17970, .F. ) ;
#32358 = LINE ( 'NONE', #30090, #11918 ) ;
#32359 = DIRECTION ( 'NONE',  ( 1.000000000000000000, 0.000000000000000000, 0.000000000000000000 ) ) ;
#32360 = ORIENTED_EDGE ( 'NONE', *, *, #1476, .F. ) ;
#32361 = AXIS2_PLACEMENT_3D ( 'NONE', #1728, #4350, #24616 ) ;
#32362 = CARTESIAN_POINT ( 'NONE',  ( 6.999996625368645198, 77.94228634059957983, -9.999999999999998224 ) ) ;
#32363 = ORIENTED_EDGE ( 'NONE', *, *, #1109, .F. ) ;
#32365 = AXIS2_PLACEMENT_3D ( 'NONE', #6016, #20428, #23253 ) ;
#32364 = FACE_BOUND ( 'NONE', #36103, .T. ) ;
#32366 = EDGE_CURVE ( 'NONE', #5185, #7360, #2106, .T. ) ;
#32367 = EDGE_CURVE ( 'NONE', #5101, #23102, #11767, .T. ) ;
#32368 = CARTESIAN_POINT ( 'NONE',  ( -68.00000337463099243, 17.32050807568877460, -9.999999999999998224 ) ) ;
#32369 = EDGE_CURVE ( 'NONE', #21899, #1539, #31436, .T. ) ;
#32370 = EDGE_CURVE ( 'NONE', #7742, #28884, #15279, .T. ) ;
#32371 = DIRECTION ( 'NONE',  ( -0.000000000000000000, 0.000000000000000000, -1.000000000000000000 ) ) ;
#32372 = ORIENTED_EDGE ( 'NONE', *, *, #2904, .F. ) ;
#32373 = DIRECTION ( 'NONE',  ( 0.000000000000000000, 0.000000000000000000, 1.000000000000000000 ) ) ;
#32374 = DIRECTION ( 'NONE',  ( -0.1497583224281852643, -0.9887226329277061243, 0.000000000000000000 ) ) ;
#32375 = FACE_OUTER_BOUND ( 'NONE', #26385, .T. ) ;
#32376 = FACE_OUTER_BOUND ( 'NONE', #4542, .T. ) ;
#32377 = DIRECTION ( 'NONE',  ( 0.000000000000000000, 0.000000000000000000, 1.000000000000000000 ) ) ;
#32378 = VERTEX_POINT ( 'NONE', #28831 ) ;
#32379 = DIRECTION ( 'NONE',  ( -0.000000000000000000, -0.000000000000000000, 1.000000000000000000 ) ) ;
#32380 = DIRECTION ( 'NONE',  ( 1.000000000000000000, 0.000000000000000000, 0.000000000000000000 ) ) ;
#32381 = CARTESIAN_POINT ( 'NONE',  ( 14.80603122773118230, -87.83969979969864994, -49.86561046011506448 ) ) ;
#32382 = ORIENTED_EDGE ( 'NONE', *, *, #16330, .T. ) ;
#32383 = ORIENTED_EDGE ( 'NONE', *, *, #18194, .T. ) ;
#32384 = AXIS2_PLACEMENT_3D ( 'NONE', #31448, #2981, #23406 ) ;
#32385 = VERTEX_POINT ( 'NONE', #3156 ) ;
#32386 = LINE ( 'NONE', #23571, #14152 ) ;
#32387 = DIRECTION ( 'NONE',  ( 1.000000000000000000, 0.000000000000000000, 0.000000000000000000 ) ) ;
#32388 = EDGE_CURVE ( 'NONE', #13513, #19051, #533, .T. ) ;
#32389 = CARTESIAN_POINT ( 'NONE',  ( 43.00330684490809574, 60.50675687296563865, -5.000000000000000000 ) ) ;
#32390 = DIRECTION ( 'NONE',  ( 1.000000000000000000, 0.000000000000000000, 0.000000000000000000 ) ) ;
#32391 = DIRECTION ( 'NONE',  ( 1.000000000000000000, 0.000000000000000000, 0.000000000000000000 ) ) ;
#32392 = CARTESIAN_POINT ( 'NONE',  ( -12.00000337463128908, 69.28203230275516944, 12.50000000000000000 ) ) ;
#32393 = ORIENTED_EDGE ( 'NONE', *, *, #4384, .F. ) ;
#32394 = ORIENTED_EDGE ( 'NONE', *, *, #36146, .F. ) ;
#32395 = CARTESIAN_POINT ( 'NONE',  ( 81.99999662536833966, 34.64101615137759183, -9.999999999999998224 ) ) ;
#32396 = CARTESIAN_POINT ( 'NONE',  ( 81.99999662536833966, 17.32050807568879236, 12.50000000000000000 ) ) ;
#32397 = VERTEX_POINT ( 'NONE', #9141 ) ;
#32398 = CARTESIAN_POINT ( 'NONE',  ( -4.400655246573610846, -3.515428273945304216, -4.176900509772398351 ) ) ;
#32399 = ORIENTED_EDGE ( 'NONE', *, *, #15234, .T. ) ;
#32400 = VECTOR ( 'NONE', #31461, 1000.000000000000000 ) ;
#32401 = FACE_BOUND ( 'NONE', #31564, .T. ) ;
#32402 = ORIENTED_EDGE ( 'NONE', *, *, #15142, .F. ) ;
#32403 = VERTEX_POINT ( 'NONE', #22087 ) ;
#32404 = EDGE_CURVE ( 'NONE', #30579, #8438, #24272, .T. ) ;
#32405 = DIRECTION ( 'NONE',  ( 0.000000000000000000, 0.000000000000000000, -1.000000000000000000 ) ) ;
#32406 = EDGE_LOOP ( 'NONE', ( #18364, #28673 ) ) ;
#32407 = FILL_AREA_STYLE ('',( #29407 ) ) ;
#32408 = DIRECTION ( 'NONE',  ( 1.000000000000000000, 0.000000000000000000, 0.000000000000000000 ) ) ;
#32409 = DIRECTION ( 'NONE',  ( 0.000000000000000000, 0.000000000000000000, 1.000000000000000000 ) ) ;
#32410 = CARTESIAN_POINT ( 'NONE',  ( 56.99999662536844625, -60.62177826491080168, -9.999999999999998224 ) ) ;
#32411 = VERTEX_POINT ( 'NONE', #15890 ) ;
#32412 = EDGE_LOOP ( 'NONE', ( #18061, #28968, #22040, #779, #24028, #15995, #16237, #27027, #26512, #30422 ) ) ;
#32413 = ORIENTED_EDGE ( 'NONE', *, *, #16234, .T. ) ;
#32414 = EDGE_LOOP ( 'NONE', ( #16484, #22140, #30389, #20392 ) ) ;
#32415 = ORIENTED_EDGE ( 'NONE', *, *, #8744, .F. ) ;
#32416 = CARTESIAN_POINT ( 'NONE',  ( -7.000003374631269537, -77.94228634059960825, 17.49999999999999645 ) ) ;
#32417 = CIRCLE ( 'NONE', #19873, 2.000000000000001776 ) ;
#32418 = CARTESIAN_POINT ( 'NONE',  ( 0.000000000000000000, 0.000000000000000000, 32.50000000000000000 ) ) ;
#32419 = ORIENTED_EDGE ( 'NONE', *, *, #17345, .F. ) ;
#32420 = CIRCLE ( 'NONE', #25830, 2.000000000000001776 ) ;
#32421 = DIRECTION ( 'NONE',  ( 0.000000000000000000, 0.000000000000000000, -1.000000000000000000 ) ) ;
#32422 = CARTESIAN_POINT ( 'NONE',  ( 78.56331849833966885, 72.23155790780543839, 32.50000000000000000 ) ) ;
#32423 = CARTESIAN_POINT ( 'NONE',  ( -51.68138994340220904, 113.8157894736842053, 32.50000000000000000 ) ) ;
#32424 = ADVANCED_FACE ( 'NONE', ( #4279 ), #18891, .F. ) ;
#32425 = VERTEX_POINT ( 'NONE', #21525 ) ;
#32426 = CARTESIAN_POINT ( 'NONE',  ( -65.00000337463104927, -43.30127018922202353, -9.999999999999998224 ) ) ;
#32427 = EDGE_CURVE ( 'NONE', #32859, #23693, #18302, .T. ) ;
#32428 = CYLINDRICAL_SURFACE ( 'NONE', #4266, 3.000000000000000888 ) ;
#32429 = DIRECTION ( 'NONE',  ( -1.000000000000000000, 0.000000000000000000, -0.000000000000000000 ) ) ;
#32430 = ORIENTED_EDGE ( 'NONE', *, *, #36470, .F. ) ;
#32431 = CARTESIAN_POINT ( 'NONE',  ( -35.19434990244938888, 52.39915983220783602, -49.22241343995295892 ) ) ;
#32432 = ADVANCED_FACE ( 'NONE', ( #9889 ), #18536, .F. ) ;
#32433 = CARTESIAN_POINT ( 'NONE',  ( 28.99999999999999289, 103.4105893997321743, -19.99999999999999645 ) ) ;
#32434 = ORIENTED_EDGE ( 'NONE', *, *, #34446, .F. ) ;
#32435 = EDGE_LOOP ( 'NONE', ( #33127, #4306, #23939, #21896, #13823 ) ) ;
#32436 = EDGE_CURVE ( 'NONE', #8160, #27610, #6198, .T. ) ;
#32437 = DIRECTION ( 'NONE',  ( 0.000000000000000000, 0.000000000000000000, 1.000000000000000000 ) ) ;
#32438 = DIRECTION ( 'NONE',  ( 0.000000000000000000, 0.000000000000000000, 1.000000000000000000 ) ) ;
#32439 = LINE ( 'NONE', #26826, #1298 ) ;
#32440 = LINE ( 'NONE', #26445, #26341 ) ;
#32441 = ORIENTED_EDGE ( 'NONE', *, *, #20004, .T. ) ;
#32442 = DIRECTION ( 'NONE',  ( 0.000000000000000000, 0.000000000000000000, 1.000000000000000000 ) ) ;
#32443 = CYLINDRICAL_SURFACE ( 'NONE', #1542, 1.999999999999998224 ) ;
#32444 = EDGE_LOOP ( 'NONE', ( #35335, #31857, #27121, #30334 ) ) ;
#32445 = CIRCLE ( 'NONE', #31830, 2.000000000000001776 ) ;
#32446 = ADVANCED_FACE ( 'NONE', ( #21325 ), #24143, .T. ) ;
#32447 = DIRECTION ( 'NONE',  ( -1.000000000000000000, 0.000000000000000000, -0.000000000000000000 ) ) ;
#32448 = ORIENTED_EDGE ( 'NONE', *, *, #14901, .F. ) ;
#32449 = DIRECTION ( 'NONE',  ( 0.000000000000000000, 0.000000000000000000, 1.000000000000000000 ) ) ;
#32450 = CARTESIAN_POINT ( 'NONE',  ( 1.999996625368696490, -86.60254037844400443, -5.000000000000000000 ) ) ;
#32451 = CARTESIAN_POINT ( 'NONE',  ( -55.00000337463107059, 43.30127018922197379, -5.000000000000000000 ) ) ;
#32452 = VERTEX_POINT ( 'NONE', #24709 ) ;
#32453 = EDGE_LOOP ( 'NONE', ( #27133, #9709, #19353, #27578, #8060 ) ) ;
#32454 = DIRECTION ( 'NONE',  ( 0.000000000000000000, 0.000000000000000000, 1.000000000000000000 ) ) ;
#32455 = ORIENTED_EDGE ( 'NONE', *, *, #25254, .T. ) ;
#32456 = DIRECTION ( 'NONE',  ( 0.000000000000000000, 0.000000000000000000, 1.000000000000000000 ) ) ;
#32457 = EDGE_CURVE ( 'NONE', #30617, #182, #24892, .T. ) ;
#32458 = FACE_BOUND ( 'NONE', #1427, .T. ) ;
#32459 = DIRECTION ( 'NONE',  ( 0.000000000000000000, 0.000000000000000000, -1.000000000000000000 ) ) ;
#32460 = CARTESIAN_POINT ( 'NONE',  ( 0.000000000000000000, 5.773502691896262640, 0.000000000000000000 ) ) ;
#32461 = DIRECTION ( 'NONE',  ( -1.000000000000000000, 0.000000000000000000, 0.000000000000000000 ) ) ;
#32462 = VERTEX_POINT ( 'NONE', #16273 ) ;
#32463 = CYLINDRICAL_SURFACE ( 'NONE', #13500, 3.000000000000002665 ) ;
#32464 = DIRECTION ( 'NONE',  ( 0.000000000000000000, 0.000000000000000000, -1.000000000000000000 ) ) ;
#32465 = PRODUCT_RELATED_PRODUCT_CATEGORY ( 'part', '', ( #10399 ) ) ;
#32466 = CIRCLE ( 'NONE', #28874, 2.000000000000001776 ) ;
#32467 = FACE_OUTER_BOUND ( 'NONE', #18849, .T. ) ;
#32468 = ORIENTED_EDGE ( 'NONE', *, *, #7577, .T. ) ;
#32469 = CARTESIAN_POINT ( 'NONE',  ( 58.48108235278871803, 36.97203788308965500, 12.49999999999999645 ) ) ;
#32470 = EDGE_CURVE ( 'NONE', #15896, #31042, #2138, .T. ) ;
#32471 = CARTESIAN_POINT ( 'NONE',  ( 0.000000000000000000, 0.000000000000000000, 12.49999999999999822 ) ) ;
#32472 = CARTESIAN_POINT ( 'NONE',  ( -42.00000337463114164, 69.28203230275516944, -9.999999999999998224 ) ) ;
#32473 = ORIENTED_EDGE ( 'NONE', *, *, #5157, .T. ) ;
#32474 = ORIENTED_EDGE ( 'NONE', *, *, #22141, .F. ) ;
#32475 = EDGE_CURVE ( 'NONE', #33006, #21999, #10514, .T. ) ;
#32476 = DIRECTION ( 'NONE',  ( -1.000000000000000000, -0.000000000000000000, -0.000000000000000000 ) ) ;
#32477 = DIRECTION ( 'NONE',  ( 0.000000000000000000, 0.000000000000000000, 1.000000000000000000 ) ) ;
#32478 = CARTESIAN_POINT ( 'NONE',  ( -58.00000337463104216, 51.96152422706639129, -9.999999999999998224 ) ) ;
#32479 = EDGE_LOOP ( 'NONE', ( #35990, #25422, #25789, #31213, #2814, #26043, #18560, #24069 ) ) ;
#32480 = EDGE_LOOP ( 'NONE', ( #38, #27835 ) ) ;
#32481 = ORIENTED_EDGE ( 'NONE', *, *, #16249, .F. ) ;
#32482 = FACE_OUTER_BOUND ( 'NONE', #4773, .T. ) ;
#32483 = CIRCLE ( 'NONE', #17500, 25.00000000000000000 ) ;
#32484 = ORIENTED_EDGE ( 'NONE', *, *, #15291, .T. ) ;
#32485 = ORIENTED_EDGE ( 'NONE', *, *, #7960, .F. ) ;
#32486 = CARTESIAN_POINT ( 'NONE',  ( 0.000000000000000000, 1.467624384280024730, -2.542000000000001592 ) ) ;
#32487 = ORIENTED_EDGE ( 'NONE', *, *, #7511, .T. ) ;
#32488 = ORIENTED_EDGE ( 'NONE', *, *, #25134, .F. ) ;
#32489 = EDGE_CURVE ( 'NONE', #21698, #35086, #29958, .T. ) ;
#32490 = FACE_OUTER_BOUND ( 'NONE', #1993, .T. ) ;
#32491 = AXIS2_PLACEMENT_3D ( 'NONE', #12069, #31267, #19846 ) ;
#32492 = DIRECTION ( 'NONE',  ( 1.000000000000000000, 0.000000000000000000, 0.000000000000000000 ) ) ;
#32493 = VERTEX_POINT ( 'NONE', #6886 ) ;
#32494 = VERTEX_POINT ( 'NONE', #1445 ) ;
#32495 = FACE_OUTER_BOUND ( 'NONE', #3054, .T. ) ;
#32496 = CARTESIAN_POINT ( 'NONE',  ( -108.3061974404896262, 19.22934205795090534, 32.50000000000000000 ) ) ;
#32497 = EDGE_CURVE ( 'NONE', #20832, #16892, #21699, .T. ) ;
#32498 = CARTESIAN_POINT ( 'NONE',  ( 0.000000000000000000, 0.000000000000000000, 17.49999999999999645 ) ) ;
#32499 = CARTESIAN_POINT ( 'NONE',  ( 26.99999662536856704, 77.94228634059957983, -9.999999999999998224 ) ) ;
#32500 = ORIENTED_EDGE ( 'NONE', *, *, #31836, .F. ) ;
#32501 = CARTESIAN_POINT ( 'NONE',  ( 54.99999662536844625, -60.62177826491080168, -9.999999999999998224 ) ) ;
#32502 = DIRECTION ( 'NONE',  ( 0.000000000000000000, 0.000000000000000000, 1.000000000000000000 ) ) ;
#32504 = VERTEX_POINT ( 'NONE', #16097 ) ;
#32503 = ADVANCED_FACE ( 'NONE', ( #18332 ), #29759, .F. ) ;
#32505 = CARTESIAN_POINT ( 'NONE',  ( 29.99999662536856349, 69.28203230275518365, -9.999999999999998224 ) ) ;
#32506 = DIRECTION ( 'NONE',  ( -1.000000000000000000, 0.000000000000000000, 0.000000000000000000 ) ) ;
#32507 = CARTESIAN_POINT ( 'NONE',  ( 35.99999999999999289, 0.000000000000000000, 0.000000000000000000 ) ) ;
#32508 = MANIFOLD_SOLID_BREP ( 'Fillet1', #34554 ) ;
#32509 = CARTESIAN_POINT ( 'NONE',  ( 56.52018970185258695, -35.83991598322081273, 12.49999999999999822 ) ) ;
#32510 = CIRCLE ( 'NONE', #4367, 2.000000000000001776 ) ;
#32511 = CARTESIAN_POINT ( 'NONE',  ( 64.99999662536842493, 43.30127018922200222, -9.999999999999998224 ) ) ;
#32512 = CARTESIAN_POINT ( 'NONE',  ( 4.999999999999999112, 0.2838785441256751474, -0.5080592402122395823 ) ) ;
#32513 = ORIENTED_EDGE ( 'NONE', *, *, #28434, .F. ) ;
#32514 = CARTESIAN_POINT ( 'NONE',  ( 56.67878100130369035, -27.78182860042797131, 12.49999999999999822 ) ) ;
#32515 = CARTESIAN_POINT ( 'NONE',  ( 79.99999662536833966, 34.64101615137759183, -5.000000000000000000 ) ) ;
#32516 = DIRECTION ( 'NONE',  ( 1.000000000000000000, 0.000000000000000000, 0.000000000000000000 ) ) ;
#32517 = ORIENTED_EDGE ( 'NONE', *, *, #29399, .T. ) ;
#32518 = ORIENTED_EDGE ( 'NONE', *, *, #18585, .T. ) ;
#32519 = ORIENTED_EDGE ( 'NONE', *, *, #3628, .T. ) ;
#32520 = EDGE_CURVE ( 'NONE', #21264, #23931, #22506, .T. ) ;
#32521 = AXIS2_PLACEMENT_3D ( 'NONE', #16386, #13574, #36463 ) ;
#32522 = DIRECTION ( 'NONE',  ( 1.000000000000000000, 0.000000000000000000, 0.000000000000000000 ) ) ;
#32523 = CARTESIAN_POINT ( 'NONE',  ( 49.99999662536846756, -69.28203230275519786, -9.999999999999998224 ) ) ;
#32524 = DIRECTION ( 'NONE',  ( -1.000000000000000000, 0.000000000000000000, 0.000000000000000000 ) ) ;
#32525 = PRODUCT_DEFINITION_SHAPE ( 'NONE', 'NONE',  #37125 ) ;
#32526 = DIRECTION ( 'NONE',  ( 0.000000000000000000, 0.000000000000000000, 1.000000000000000000 ) ) ;
#32527 = DIRECTION ( 'NONE',  ( 0.000000000000000000, 0.000000000000000000, 1.000000000000000000 ) ) ;
#32528 = ORIENTED_EDGE ( 'NONE', *, *, #3052, .F. ) ;
#32529 = FACE_OUTER_BOUND ( 'NONE', #12590, .T. ) ;
#32530 = ORIENTED_EDGE ( 'NONE', *, *, #9971, .F. ) ;
#32531 = FACE_BOUND ( 'NONE', #13719, .T. ) ;
#32532 = CIRCLE ( 'NONE', #27743, 17.55872235085560007 ) ;
#32533 = CIRCLE ( 'NONE', #18162, 3.750000000000001776 ) ;
#32534 = EDGE_CURVE ( 'NONE', #27413, #5488, #5147, .T. ) ;
#32535 = DIRECTION ( 'NONE',  ( 0.000000000000000000, 0.000000000000000000, 1.000000000000000000 ) ) ;
#32536 = FACE_OUTER_BOUND ( 'NONE', #13458, .T. ) ;
#32537 = DIRECTION ( 'NONE',  ( -0.000000000000000000, -0.000000000000000000, 1.000000000000000000 ) ) ;
#32538 = EDGE_CURVE ( 'NONE', #34151, #27516, #20094, .T. ) ;
#32539 = ORIENTED_EDGE ( 'NONE', *, *, #7466, .T. ) ;
#32540 = DIRECTION ( 'NONE',  ( 1.000000000000000000, 0.000000000000000000, 0.000000000000000000 ) ) ;
#32541 = AXIS2_PLACEMENT_3D ( 'NONE', #8846, #5863, #20095 ) ;
#32542 = ADVANCED_FACE ( 'NONE', ( #8561 ), #31069, .F. ) ;
#32543 = CARTESIAN_POINT ( 'NONE',  ( 26.99999662536859546, -77.94228634059960825, -5.000000000000000000 ) ) ;
#32544 = AXIS2_PLACEMENT_3D ( 'NONE', #30955, #21609, #13518 ) ;
#32545 = DIRECTION ( 'NONE',  ( -1.000000000000000000, 0.000000000000000000, 0.000000000000000000 ) ) ;
#32546 = DIRECTION ( 'NONE',  ( -1.000000000000000000, 0.000000000000000000, 0.000000000000000000 ) ) ;
#32547 = ORIENTED_EDGE ( 'NONE', *, *, #1790, .T. ) ;
#32548 = CARTESIAN_POINT ( 'NONE',  ( -10.00000337463128730, 69.28203230275516944, 17.49999999999999645 ) ) ;
#32549 = EDGE_CURVE ( 'NONE', #68, #13800, #11126, .T. ) ;
#32550 = CARTESIAN_POINT ( 'NONE',  ( -10.00000337463128197, 86.60254037844397601, 17.49999999999999645 ) ) ;
#32551 = DIRECTION ( 'NONE',  ( 1.000000000000000000, 0.000000000000000000, 0.000000000000000000 ) ) ;
#32552 = ADVANCED_FACE ( 'NONE', ( #7841 ), #22825, .F. ) ;
#32553 = CIRCLE ( 'NONE', #2611, 1.999999999999998224 ) ;
#32554 = ORIENTED_EDGE ( 'NONE', *, *, #34300, .T. ) ;
#32555 = ORIENTED_EDGE ( 'NONE', *, *, #19835, .F. ) ;
#32556 = EDGE_LOOP ( 'NONE', ( #7018, #31482 ) ) ;
#32557 = CARTESIAN_POINT ( 'NONE',  ( -55.27226924886182502, -77.26562141134519379, 27.50000000000000000 ) ) ;
#32558 = CARTESIAN_POINT ( 'NONE',  ( 14.99999662536863632, -77.94228634059960825, -5.000000000000000000 ) ) ;
#32559 = ADVANCED_FACE ( 'NONE', ( #2198 ), #34084, .F. ) ;
#32560 = EDGE_CURVE ( 'NONE', #11572, #27066, #24902, .T. ) ;
#32561 = AXIS2_PLACEMENT_3D ( 'NONE', #28824, #23217, #34673 ) ;
#32562 = CARTESIAN_POINT ( 'NONE',  ( -27.78182860042817026, -56.67878100130359087, 12.49999999999999822 ) ) ;
#32563 = EDGE_CURVE ( 'NONE', #36578, #20452, #6931, .T. ) ;
#32564 = EDGE_CURVE ( 'NONE', #31600, #13165, #2746, .T. ) ;
#32565 = CARTESIAN_POINT ( 'NONE',  ( -27.78182860042817026, -56.67878100130359087, -4.999999999999997335 ) ) ;
#32566 = DIRECTION ( 'NONE',  ( 1.000000000000000000, 0.000000000000000000, 0.000000000000000000 ) ) ;
#32567 = EDGE_CURVE ( 'NONE', #20619, #33480, #30864, .T. ) ;
#32568 = DIRECTION ( 'NONE',  ( 0.000000000000000000, 0.000000000000000000, 1.000000000000000000 ) ) ;
#32569 = ORIENTED_EDGE ( 'NONE', *, *, #6671, .T. ) ;
#32570 = AXIS2_PLACEMENT_3D ( 'NONE', #27187, #4898, #4335 ) ;
#32571 = ORIENTED_EDGE ( 'NONE', *, *, #70, .T. ) ;
#32572 = CARTESIAN_POINT ( 'NONE',  ( -45.00000337463112743, -60.62177826491080168, -9.999999999999998224 ) ) ;
#32573 = AXIS2_PLACEMENT_3D ( 'NONE', #28702, #31689, #22891 ) ;
#32574 = DIRECTION ( 'NONE',  ( -0.000000000000000000, 0.000000000000000000, -1.000000000000000000 ) ) ;
#32575 = ORIENTED_EDGE ( 'NONE', *, *, #25976, .T. ) ;
#32576 = CARTESIAN_POINT ( 'NONE',  ( -65.00000000000000000, 0.000000000000000000, 17.49999999999999645 ) ) ;
#32577 = ORIENTED_EDGE ( 'NONE', *, *, #24579, .T. ) ;
#32578 = FACE_BOUND ( 'NONE', #10815, .T. ) ;
#32579 = ORIENTED_EDGE ( 'NONE', *, *, #16133, .T. ) ;
#32580 = EDGE_LOOP ( 'NONE', ( #20097, #17056, #28850, #16850 ) ) ;
#32581 = DIRECTION ( 'NONE',  ( 1.000000000000000000, 0.000000000000000000, 0.000000000000000000 ) ) ;
#32582 = ORIENTED_EDGE ( 'NONE', *, *, #22761, .F. ) ;
#32583 = SURFACE_STYLE_FILL_AREA ( #32407 ) ;
#32584 = STYLED_ITEM ( 'NONE', ( #3672 ), #31591 ) ;
#32585 = DIRECTION ( 'NONE',  ( 0.000000000000000000, 0.000000000000000000, 1.000000000000000000 ) ) ;
#32586 = CARTESIAN_POINT ( 'NONE',  ( 49.99999662536846756, -69.28203230275519786, -5.000000000000000000 ) ) ;
#32587 = CARTESIAN_POINT ( 'NONE',  ( 11.99999662536865763, -86.60254037844400443, -5.000000000000000000 ) ) ;
#32588 = ORIENTED_EDGE ( 'NONE', *, *, #29534, .F. ) ;
#32589 = ORIENTED_EDGE ( 'NONE', *, *, #25638, .F. ) ;
#32590 = VERTEX_POINT ( 'NONE', #5201 ) ;
#32591 = VECTOR ( 'NONE', #36944, 1000.000000000000000 ) ;
#32592 = AXIS2_PLACEMENT_3D ( 'NONE', #12701, #29405, #9900 ) ;
#32593 = EDGE_LOOP ( 'NONE', ( #35428, #20900, #32382, #15644 ) ) ;
#32594 = ORIENTED_EDGE ( 'NONE', *, *, #14972, .F. ) ;
#32595 = FACE_OUTER_BOUND ( 'NONE', #7991, .T. ) ;
#32596 = CIRCLE ( 'NONE', #8650, 2.000000000000001776 ) ;
#32597 = CARTESIAN_POINT ( 'NONE',  ( 76.99999662536835388, -43.30127018922199511, -5.000000000000000000 ) ) ;
#32598 = ORIENTED_EDGE ( 'NONE', *, *, #34868, .F. ) ;
#32599 = CARTESIAN_POINT ( 'NONE',  ( -58.00000337463104216, 51.96152422706639129, 17.49999999999999645 ) ) ;
#32600 = CARTESIAN_POINT ( 'NONE',  ( 107.2802272138360422, 45.32406911912114822, 32.50000000000000000 ) ) ;
#32601 = CARTESIAN_POINT ( 'NONE',  ( 69.99999662536838230, -51.96152422706639840, -5.000000000000000000 ) ) ;
#32602 = ORIENTED_EDGE ( 'NONE', *, *, #16318, .F. ) ;
#32603 = LINE ( 'NONE', #18574, #11637 ) ;
#32604 = EDGE_CURVE ( 'NONE', #34166, #28642, #29074, .T. ) ;
#32605 = DIRECTION ( 'NONE',  ( 0.000000000000000000, 0.000000000000000000, 1.000000000000000000 ) ) ;
#32606 = AXIS2_PLACEMENT_3D ( 'NONE', #12349, #31686, #29426 ) ;
#32607 = EDGE_CURVE ( 'NONE', #8583, #911, #8724, .T. ) ;
#32608 = LINE ( 'NONE', #26258, #265 ) ;
#32609 = ORIENTED_EDGE ( 'NONE', *, *, #35042, .T. ) ;
#32610 = DIRECTION ( 'NONE',  ( 0.000000000000000000, 0.000000000000000000, 1.000000000000000000 ) ) ;
#32611 = CIRCLE ( 'NONE', #8049, 20.00000000000001066 ) ;
#32612 = LINE ( 'NONE', #18580, #7013 ) ;
#32613 = ORIENTED_EDGE ( 'NONE', *, *, #6212, .T. ) ;
#32614 = CIRCLE ( 'NONE', #30204, 8.500000000000007105 ) ;
#32615 = ORIENTED_EDGE ( 'NONE', *, *, #28542, .F. ) ;
#32616 = DIRECTION ( 'NONE',  ( 1.000000000000000000, 0.000000000000000000, 0.000000000000000000 ) ) ;
#32617 = DIRECTION ( 'NONE',  ( -1.000000000000000000, 0.000000000000000000, 0.000000000000000000 ) ) ;
#32618 = DIRECTION ( 'NONE',  ( 0.8660254037844337116, -0.5000000000000084377, 0.000000000000000000 ) ) ;
#32619 = CARTESIAN_POINT ( 'NONE',  ( 59.99999662536845335, 34.64101615137759893, -9.999999999999998224 ) ) ;
#32620 = VERTEX_POINT ( 'NONE', #11906 ) ;
#32621 = CARTESIAN_POINT ( 'NONE',  ( -67.00000337463102085, 25.98076211353317433, 12.50000000000000000 ) ) ;
#32622 = CIRCLE ( 'NONE', #24251, 45.00000000000000000 ) ;
#32623 = DIRECTION ( 'NONE',  ( 1.000000000000000000, 0.000000000000000000, 0.000000000000000000 ) ) ;
#32624 = VERTEX_POINT ( 'NONE', #18089 ) ;
#32625 = LINE ( 'NONE', #12937, #11217 ) ;
#32626 = ORIENTED_EDGE ( 'NONE', *, *, #21291, .T. ) ;
#32627 = EDGE_CURVE ( 'NONE', #12872, #14823, #7519, .T. ) ;
#32628 = CARTESIAN_POINT ( 'NONE',  ( 52.99999662536844625, -60.62177826491080168, -5.000000000000000000 ) ) ;
#32629 = LINE ( 'NONE', #18770, #14605 ) ;
#32630 = CIRCLE ( 'NONE', #21262, 3.500000000000003109 ) ;
#32631 = CARTESIAN_POINT ( 'NONE',  ( -60.00000337463107059, -34.64101615137762025, -5.000000000000000000 ) ) ;
#32632 = VERTEX_POINT ( 'NONE', #837 ) ;
#32633 = CIRCLE ( 'NONE', #11065, 3.499999999999996003 ) ;
#32634 = ORIENTED_EDGE ( 'NONE', *, *, #30685, .T. ) ;
#32635 = CIRCLE ( 'NONE', #6305, 27.00000000000001776 ) ;
#32636 = CIRCLE ( 'NONE', #22477, 2.000000000000001776 ) ;
#32637 = EDGE_CURVE ( 'NONE', #16950, #9855, #5734, .T. ) ;
#32638 = VERTEX_POINT ( 'NONE', #17918 ) ;
#32639 = CARTESIAN_POINT ( 'NONE',  ( 89.27079897466127534, -32.49191361593859995, -4.999999999999997335 ) ) ;
#32640 = FACE_BOUND ( 'NONE', #6457, .T. ) ;
#32641 = CARTESIAN_POINT ( 'NONE',  ( 9.999996625368655856, -69.28203230275519786, -9.999999999999998224 ) ) ;
#32642 = LINE ( 'NONE', #34920, #12083 ) ;
#32643 = VECTOR ( 'NONE', #18097, 1000.000000000000000 ) ;
#32644 = CYLINDRICAL_SURFACE ( 'NONE', #17728, 2.000000000000000000 ) ;
#32645 = ORIENTED_EDGE ( 'NONE', *, *, #14236, .F. ) ;
#32646 = CARTESIAN_POINT ( 'NONE',  ( -25.00000337463120914, 77.94228634059957983, -9.999999999999998224 ) ) ;
#32647 = CIRCLE ( 'NONE', #33871, 27.00000000000001421 ) ;
#32648 = CIRCLE ( 'NONE', #10524, 2.000000000000001776 ) ;
#32649 = CARTESIAN_POINT ( 'NONE',  ( -73.00000337463097821, -8.660254037844422825, -9.999999999999998224 ) ) ;
#32650 = EDGE_CURVE ( 'NONE', #20452, #32323, #35685, .T. ) ;
#32651 = CARTESIAN_POINT ( 'NONE',  ( -27.78182860042817026, -56.67878100130359087, -4.999999999999997335 ) ) ;
#32652 = ORIENTED_EDGE ( 'NONE', *, *, #697, .T. ) ;
#32653 = DIRECTION ( 'NONE',  ( 0.000000000000000000, 0.000000000000000000, 1.000000000000000000 ) ) ;
#32654 = DIRECTION ( 'NONE',  ( 1.000000000000000000, 0.000000000000000000, 0.000000000000000000 ) ) ;
#32655 = DIRECTION ( 'NONE',  ( 0.000000000000000000, 0.000000000000000000, 1.000000000000000000 ) ) ;
#32656 = ORIENTED_EDGE ( 'NONE', *, *, #32297, .T. ) ;
#32657 = ORIENTED_EDGE ( 'NONE', *, *, #17177, .T. ) ;
#32658 = LINE ( 'NONE', #21424, #4954 ) ;
#32659 = DIRECTION ( 'NONE',  ( 1.000000000000000000, 0.000000000000000000, 0.000000000000000000 ) ) ;
#32660 = AXIS2_PLACEMENT_3D ( 'NONE', #6611, #6224, #17657 ) ;
#32661 = CARTESIAN_POINT ( 'NONE',  ( -10.00000337463128730, 69.28203230275516944, 17.49999999999999645 ) ) ;
#32662 = ORIENTED_EDGE ( 'NONE', *, *, #11289, .T. ) ;
#32663 = VERTEX_POINT ( 'NONE', #663 ) ;
#32664 = CIRCLE ( 'NONE', #34472, 2.000000000000001776 ) ;
#32665 = ORIENTED_EDGE ( 'NONE', *, *, #20296, .T. ) ;
#32666 = CIRCLE ( 'NONE', #32026, 19.53925848833874213 ) ;
#32667 = VECTOR ( 'NONE', #10789, 1000.000000000000000 ) ;
#32668 = AXIS2_PLACEMENT_3D ( 'NONE', #25978, #35379, #34621 ) ;
#32669 = CYLINDRICAL_SURFACE ( 'NONE', #6927, 2.000000000000001776 ) ;
#32670 = ORIENTED_EDGE ( 'NONE', *, *, #22710, .T. ) ;
#32671 = EDGE_CURVE ( 'NONE', #35959, #32911, #28464, .T. ) ;
#32672 = EDGE_LOOP ( 'NONE', ( #28061, #22439 ) ) ;
#32673 = CARTESIAN_POINT ( 'NONE',  ( 46.99999662536851019, -60.62177826491080168, -5.000000000000000000 ) ) ;
#32674 = ORIENTED_EDGE ( 'NONE', *, *, #25444, .F. ) ;
#32675 = EDGE_CURVE ( 'NONE', #33391, #6042, #30264, .T. ) ;
#32676 = VERTEX_POINT ( 'NONE', #9093 ) ;
#32677 = AXIS2_PLACEMENT_3D ( 'NONE', #33135, #13267, #17197 ) ;
#32678 = CARTESIAN_POINT ( 'NONE',  ( -7.041719095097282852E-16, 78.44802294027068967, 32.49999999999999289 ) ) ;
#32679 = CARTESIAN_POINT ( 'NONE',  ( -55.00000337463110611, -43.30127018922202353, -9.999999999999998224 ) ) ;
#32680 = VERTEX_POINT ( 'NONE', #23726 ) ;
#32681 = ADVANCED_FACE ( 'NONE', ( #23368 ), #14920, .F. ) ;
#32682 = ORIENTED_EDGE ( 'NONE', *, *, #3278, .T. ) ;
#32683 = CARTESIAN_POINT ( 'NONE',  ( 71.99999662536838230, -51.96152422706639840, -9.999999999999998224 ) ) ;
#32684 = DIRECTION ( 'NONE',  ( 1.000000000000000000, 0.000000000000000000, 0.000000000000000000 ) ) ;
#32685 = CIRCLE ( 'NONE', #20140, 3.499999999999989342 ) ;
#32686 = DIRECTION ( 'NONE',  ( -0.000000000000000000, -0.000000000000000000, -1.000000000000000000 ) ) ;
#32687 = CARTESIAN_POINT ( 'NONE',  ( 32.99999662536855283, -77.94228634059960825, -9.999999999999998224 ) ) ;
#32688 = EDGE_CURVE ( 'NONE', #17855, #35211, #280, .T. ) ;
#32689 = CIRCLE ( 'NONE', #33289, 2.000000000000000000 ) ;
#32690 = ORIENTED_EDGE ( 'NONE', *, *, #27321, .F. ) ;
#32691 = CYLINDRICAL_SURFACE ( 'NONE', #14757, 2.000000000000001776 ) ;
#32692 = ORIENTED_EDGE ( 'NONE', *, *, #26626, .F. ) ;
#32693 = DIRECTION ( 'NONE',  ( 0.000000000000000000, 0.000000000000000000, 1.000000000000000000 ) ) ;
#32694 = LINE ( 'NONE', #18651, #17805 ) ;
#32695 = CARTESIAN_POINT ( 'NONE',  ( 5.999999999999985789, 149.8799519615616305, 32.50000000000000000 ) ) ;
#32696 = AXIS2_PLACEMENT_3D ( 'NONE', #30007, #15584, #32623 ) ;
#32697 = AXIS2_PLACEMENT_3D ( 'NONE', #12568, #12737, #24023 ) ;
#32698 = CARTESIAN_POINT ( 'NONE',  ( 74.99999662536836809, 8.660254037844394404, -9.999999999999998224 ) ) ;
#32699 = AXIS2_PLACEMENT_3D ( 'NONE', #12250, #23534, #6662 ) ;
#32700 = AXIS2_PLACEMENT_3D ( 'NONE', #22454, #33905, #3524 ) ;
#32701 = CARTESIAN_POINT ( 'NONE',  ( -33.00000337463116296, 77.94228634059957983, 17.49999999999999645 ) ) ;
#32702 = DIRECTION ( 'NONE',  ( 1.000000000000000000, 0.000000000000000000, 0.000000000000000000 ) ) ;
#32703 = EDGE_LOOP ( 'NONE', ( #14138, #13177 ) ) ;
#32704 = DIRECTION ( 'NONE',  ( 0.000000000000000000, 0.000000000000000000, -1.000000000000000000 ) ) ;
#32705 = CARTESIAN_POINT ( 'NONE',  ( -47.04203867989546950, 43.19957991610416315, 12.49999999999999822 ) ) ;
#32706 = DIRECTION ( 'NONE',  ( 1.000000000000000000, 0.000000000000000000, 0.000000000000000000 ) ) ;
#32707 = ORIENTED_EDGE ( 'NONE', *, *, #22376, .F. ) ;
#32708 = AXIS2_PLACEMENT_3D ( 'NONE', #31212, #16957, #16408 ) ;
#32709 = EDGE_CURVE ( 'NONE', #27114, #21666, #24302, .T. ) ;
#32710 = ORIENTED_EDGE ( 'NONE', *, *, #3345, .T. ) ;
#32711 = VERTEX_POINT ( 'NONE', #9274 ) ;
#32712 = CARTESIAN_POINT ( 'NONE',  ( 0.000000000000000000, 0.000000000000000000, 12.49999999999999822 ) ) ;
#32713 = DIRECTION ( 'NONE',  ( 0.000000000000000000, 0.000000000000000000, 1.000000000000000000 ) ) ;
#32714 = CARTESIAN_POINT ( 'NONE',  ( 6.000000000000000000, 0.000000000000000000, 0.000000000000000000 ) ) ;
#32715 = EDGE_LOOP ( 'NONE', ( #31302, #5274 ) ) ;
#32716 = AXIS2_PLACEMENT_3D ( 'NONE', #24254, #21639, #21453 ) ;
#32717 = EDGE_CURVE ( 'NONE', #31926, #19348, #20709, .T. ) ;
#32718 = LINE ( 'NONE', #21483, #5366 ) ;
#32719 = VECTOR ( 'NONE', #33408, 1000.000000000000000 ) ;
#32720 = CARTESIAN_POINT ( 'NONE',  ( -58.00000337463107059, -34.64101615137762025, -5.000000000000000000 ) ) ;
#32721 = ORIENTED_EDGE ( 'NONE', *, *, #16427, .T. ) ;
#32722 = EDGE_CURVE ( 'NONE', #2002, #14001, #8142, .T. ) ;
#32723 = FACE_BOUND ( 'NONE', #2692, .T. ) ;
#32724 = B_SPLINE_CURVE_WITH_KNOTS ( 'NONE', 3,
 ( #13794, #25234, #24857, #7799, #16798, #37039, #36294, #10605 ),
 .UNSPECIFIED., .F., .F.,
 ( 4, 2, 2, 4 ),
 ( 0.002921158011986710323, 0.003648658599403066614, 0.004376159186819422904, 0.005831160361652134617 ),
 .UNSPECIFIED. ) ;
#32725 = VERTEX_POINT ( 'NONE', #29154 ) ;
#32726 = AXIS2_PLACEMENT_3D ( 'NONE', #36543, #22274, #8403 ) ;
#32727 = FACE_BOUND ( 'NONE', #6376, .T. ) ;
#32728 = CIRCLE ( 'NONE', #30928, 2.000000000000001776 ) ;
#32729 = AXIS2_PLACEMENT_3D ( 'NONE', #9783, #7534, #4544 ) ;
#32730 = AXIS2_PLACEMENT_3D ( 'NONE', #22069, #33510, #7821 ) ;
#32731 = CYLINDRICAL_SURFACE ( 'NONE', #23772, 2.000000000000001776 ) ;
#32732 = LINE ( 'NONE', #23946, #29301 ) ;
#32733 = CARTESIAN_POINT ( 'NONE',  ( 1.999996625368696490, -86.60254037844400443, -9.999999999999998224 ) ) ;
#32734 = ORIENTED_EDGE ( 'NONE', *, *, #20793, .T. ) ;
#32735 = DIRECTION ( 'NONE',  ( -0.000000000000000000, -0.000000000000000000, 1.000000000000000000 ) ) ;
#32736 = ITEM_DEFINED_TRANSFORMATION ( 'NONE', 'NONE', #3394,  #21385 ) ;
#32737 = AXIS2_PLACEMENT_3D ( 'NONE', #11632, #23284, #17467 ) ;
#32738 = DIRECTION ( 'NONE',  ( 0.5000000000000045519, -0.8660254037844360431, 0.000000000000000000 ) ) ;
#32739 = EDGE_CURVE ( 'NONE', #29078, #30836, #26165, .T. ) ;
#32740 = DIRECTION ( 'NONE',  ( 0.000000000000000000, 0.000000000000000000, 1.000000000000000000 ) ) ;
#32741 = CYLINDRICAL_SURFACE ( 'NONE', #19745, 2.000000000000001776 ) ;
#32742 = ORIENTED_EDGE ( 'NONE', *, *, #15375, .F. ) ;
#32743 = CARTESIAN_POINT ( 'NONE',  ( 3.500000000000000888, -55.00000000000000000, 5.000000000000000888 ) ) ;
#32744 = LINE ( 'NONE', #7625, #17261 ) ;
#32745 = DIRECTION ( 'NONE',  ( 0.000000000000000000, 0.000000000000000000, -1.000000000000000000 ) ) ;
#32746 = AXIS2_PLACEMENT_3D ( 'NONE', #21960, #28306, #2069 ) ;
#32747 = ORIENTED_EDGE ( 'NONE', *, *, #19293, .F. ) ;
#32748 = ORIENTED_EDGE ( 'NONE', *, *, #6789, .T. ) ;
#32749 = AXIS2_PLACEMENT_3D ( 'NONE', #36369, #2233, #26164 ) ;
#32750 = CLOSED_SHELL ( 'NONE', ( #31016, #5762, #22049, #27000, #20895, #32338, #22819, #31612, #21081, #29204, #11563, #187, #9885, #11460, #13218, #10162, #13832, #10254, #11546, #26463, #11023, #3370, #201, #32215, #20119, #18352, #26261 ) ) ;
#32751 = ORIENTED_EDGE ( 'NONE', *, *, #20100, .F. ) ;
#32752 = VECTOR ( 'NONE', #33405, 1000.000000000000000 ) ;
#32753 = DIRECTION ( 'NONE',  ( -1.047444401652940007E-14, -1.000000000000000000, 0.000000000000000000 ) ) ;
#32754 = LINE ( 'NONE', #15879, #14739 ) ;
#32755 = AXIS2_PLACEMENT_3D ( 'NONE', #28934, #9455, #20886 ) ;
#32756 = AXIS2_PLACEMENT_3D ( 'NONE', #28706, #2845, #34332 ) ;
#32757 = CYLINDRICAL_SURFACE ( 'NONE', #18640, 2.000000000000001776 ) ;
#32758 = AXIS2_PLACEMENT_3D ( 'NONE', #27685, #33695, #13072 ) ;
#32759 = AXIS2_PLACEMENT_3D ( 'NONE', #31231, #34416, #2933 ) ;
#32760 = EDGE_CURVE ( 'NONE', #8805, #14671, #35716, .T. ) ;
#32761 = ORIENTED_EDGE ( 'NONE', *, *, #31171, .F. ) ;
#32762 = DIRECTION ( 'NONE',  ( 0.000000000000000000, 0.000000000000000000, 1.000000000000000000 ) ) ;
#32763 = DIRECTION ( 'NONE',  ( 1.000000000000000000, 0.000000000000000000, 0.000000000000000000 ) ) ;
#32764 = ADVANCED_FACE ( 'NONE', ( #15275 ), #14537, .F. ) ;
#32765 = CARTESIAN_POINT ( 'NONE',  ( -93.06207005441154934, 70.18581618242465936, 32.50000000000000000 ) ) ;
#32766 = ORIENTED_EDGE ( 'NONE', *, *, #9771, .F. ) ;
#32767 = VECTOR ( 'NONE', #33186, 1000.000000000000000 ) ;
#32768 = EDGE_CURVE ( 'NONE', #10304, #24584, #14125, .T. ) ;
#32769 = ORIENTED_EDGE ( 'NONE', *, *, #10234, .F. ) ;
#32770 = CARTESIAN_POINT ( 'NONE',  ( -50.00000337463109190, 51.96152422706637708, -5.000000000000000000 ) ) ;
#32771 = DIRECTION ( 'NONE',  ( -1.000000000000000000, 0.000000000000000000, 0.000000000000000000 ) ) ;
#32772 = ORIENTED_EDGE ( 'NONE', *, *, #22923, .F. ) ;
#32773 = EDGE_CURVE ( 'NONE', #5559, #19449, #22536, .T. ) ;
#32774 = CYLINDRICAL_SURFACE ( 'NONE', #7773, 3.500000000000003109 ) ;
#32775 = ADVANCED_FACE ( 'NONE', ( #10223 ), #15661, .F. ) ;
#32776 = ORIENTED_EDGE ( 'NONE', *, *, #28798, .T. ) ;
#32777 = CARTESIAN_POINT ( 'NONE',  ( -78.00000337463094979, -2.428612866367529932E-14, 12.50000000000000000 ) ) ;
#32778 = CIRCLE ( 'NONE', #20228, 27.00000000000001776 ) ;
#32779 = AXIS2_PLACEMENT_3D ( 'NONE', #15832, #13576, #5139 ) ;
#32780 = DIRECTION ( 'NONE',  ( -1.000000000000000000, 0.000000000000000000, -0.000000000000000000 ) ) ;
#32781 = EDGE_LOOP ( 'NONE', ( #34261, #6720, #12372, #11664 ) ) ;
#32782 = ORIENTED_EDGE ( 'NONE', *, *, #24185, .F. ) ;
#32783 = DIRECTION ( 'NONE',  ( 1.000000000000000000, 0.000000000000000000, 0.000000000000000000 ) ) ;
#32784 = ORIENTED_EDGE ( 'NONE', *, *, #11674, .T. ) ;
#32785 = EDGE_CURVE ( 'NONE', #29590, #23780, #1780, .T. ) ;
#32786 = COLOUR_RGB ( '', 0.66274510, 0.83137255, 0.94901961) ;
#32787 = CIRCLE ( 'NONE', #4045, 2.000000000000001776 ) ;
#32788 = ADVANCED_FACE ( 'NONE', ( #24477 ), #1948, .F. ) ;
#32789 = CARTESIAN_POINT ( 'NONE',  ( -2.500000000000022204, 4.330127018922177662, 0.000000000000000000 ) ) ;
#32790 = AXIS2_PLACEMENT_3D ( 'NONE', #20887, #32319, #3810 ) ;
#32791 = ADVANCED_FACE ( 'NONE', ( #30461 ), #12644, .F. ) ;
#32792 = CARTESIAN_POINT ( 'NONE',  ( 2.712167343862820434, 4.207632145829745873, -6.000000000000002665 ) ) ;
#32793 = DIRECTION ( 'NONE',  ( 0.000000000000000000, 0.000000000000000000, -1.000000000000000000 ) ) ;
#32794 = EDGE_LOOP ( 'NONE', ( #31423, #31400 ) ) ;
#32795 = DIRECTION ( 'NONE',  ( 0.000000000000000000, 0.000000000000000000, 1.000000000000000000 ) ) ;
#32796 = ORIENTED_EDGE ( 'NONE', *, *, #949, .T. ) ;
#32797 = ORIENTED_EDGE ( 'NONE', *, *, #4650, .F. ) ;
#32798 = ORIENTED_EDGE ( 'NONE', *, *, #30972, .T. ) ;
#32799 = CARTESIAN_POINT ( 'NONE',  ( 37.99999662536853151, 69.28203230275518365, -9.999999999999998224 ) ) ;
#32800 = CARTESIAN_POINT ( 'NONE',  ( 91.99999662536828282, 0.000000000000000000, 12.50000000000000000 ) ) ;
#32801 = ORIENTED_EDGE ( 'NONE', *, *, #17216, .F. ) ;
#32802 = AXIS2_PLACEMENT_3D ( 'NONE', #34079, #27684, #22426 ) ;
#32803 = AXIS2_PLACEMENT_3D ( 'NONE', #5080, #21768, #16168 ) ;
#32804 = DIRECTION ( 'NONE',  ( 0.000000000000000000, 0.000000000000000000, -1.000000000000000000 ) ) ;
#32805 = CARTESIAN_POINT ( 'NONE',  ( 67.99999662536836809, -51.96152422706639840, -9.999999999999998224 ) ) ;
#32806 = ORIENTED_EDGE ( 'NONE', *, *, #35183, .F. ) ;
#32807 = FACE_OUTER_BOUND ( 'NONE', #30035, .T. ) ;
#32808 = CIRCLE ( 'NONE', #13671, 2.000000000000001776 ) ;
#32809 = DIRECTION ( 'NONE',  ( 1.000000000000000000, 0.000000000000000000, 0.000000000000000000 ) ) ;
#32810 = EDGE_CURVE ( 'NONE', #30431, #33375, #34499, .T. ) ;
#32811 = AXIS2_PLACEMENT_3D ( 'NONE', #3978, #29648, #21217 ) ;
#32812 = CARTESIAN_POINT ( 'NONE',  ( -42.00000337463114164, -69.28203230275519786, -9.999999999999998224 ) ) ;
#32813 = DIRECTION ( 'NONE',  ( 1.000000000000000000, 0.000000000000000000, 0.000000000000000000 ) ) ;
#32814 = ADVANCED_FACE ( 'NONE', ( #7226 ), #4232, .F. ) ;
#32815 = FACE_OUTER_BOUND ( 'NONE', #34440, .T. ) ;
#32816 = CYLINDRICAL_SURFACE ( 'NONE', #31024, 2.000000000000001776 ) ;
#32817 = ORIENTED_EDGE ( 'NONE', *, *, #23763, .T. ) ;
#32818 = EDGE_LOOP ( 'NONE', ( #29781, #33558 ) ) ;
#32819 = AXIS2_PLACEMENT_3D ( 'NONE', #27170, #35829, #1691 ) ;
#32820 = CARTESIAN_POINT ( 'NONE',  ( 74.99999662536836809, 25.98076211353319565, 12.50000000000000000 ) ) ;
#32821 = CARTESIAN_POINT ( 'NONE',  ( 26.99999662536856704, 77.94228634059957983, -9.999999999999998224 ) ) ;
#32822 = DIRECTION ( 'NONE',  ( 0.000000000000000000, 0.000000000000000000, 1.000000000000000000 ) ) ;
#32823 = CARTESIAN_POINT ( 'NONE',  ( 64.99999662536839651, 60.62177826491078747, -5.000000000000000000 ) ) ;
#32824 = EDGE_CURVE ( 'NONE', #22858, #20479, #18268, .T. ) ;
#32825 = ORIENTED_EDGE ( 'NONE', *, *, #8535, .T. ) ;
#32826 = UNCERTAINTY_MEASURE_WITH_UNIT (LENGTH_MEASURE( 1.000000000000000082E-05 ), #26416, 'distance_accuracy_value', 'NONE');
#32827 = AXIS2_PLACEMENT_3D ( 'NONE', #23652, #27149, #33353 ) ;
#32828 = DIRECTION ( 'NONE',  ( -0.000000000000000000, 0.000000000000000000, -1.000000000000000000 ) ) ;
#32829 = CARTESIAN_POINT ( 'NONE',  ( 79.99999662536833966, 34.64101615137759183, 17.49999999999999645 ) ) ;
#32830 = AXIS2_PLACEMENT_3D ( 'NONE', #17841, #34908, #29273 ) ;
#32831 = ORIENTED_EDGE ( 'NONE', *, *, #19407, .F. ) ;
#32832 = AXIS2_PLACEMENT_3D ( 'NONE', #918, #12345, #23813 ) ;
#32833 = DIRECTION ( 'NONE',  ( 1.000000000000000000, 0.000000000000000000, 0.000000000000000000 ) ) ;
#32834 = EDGE_LOOP ( 'NONE', ( #255, #26168 ) ) ;
#32835 = EDGE_CURVE ( 'NONE', #36432, #29465, #36275, .T. ) ;
#32836 = DIRECTION ( 'NONE',  ( 0.000000000000000000, 0.000000000000000000, 1.000000000000000000 ) ) ;
#32837 = EDGE_CURVE ( 'NONE', #5148, #4, #18330, .T. ) ;
#32838 = CARTESIAN_POINT ( 'NONE',  ( 86.99999662536832545, 8.660254037844394404, 12.50000000000000000 ) ) ;
#32839 = AXIS2_PLACEMENT_3D ( 'NONE', #26064, #32034, #15011 ) ;
#32840 = ADVANCED_FACE ( 'NONE', ( #19037 ), #10029, .F. ) ;
#32841 = CARTESIAN_POINT ( 'NONE',  ( 4.084562121000262280, 3.415279651815005924, -1.156968425231149844 ) ) ;
#32842 = EDGE_CURVE ( 'NONE', #3287, #8594, #2165, .T. ) ;
#32843 = ORIENTED_EDGE ( 'NONE', *, *, #16279, .F. ) ;
#32844 = ORIENTED_EDGE ( 'NONE', *, *, #25267, .F. ) ;
#32845 = AXIS2_PLACEMENT_3D ( 'NONE', #14463, #32, #28877 ) ;
#32846 = CIRCLE ( 'NONE', #14297, 2.000000000000001776 ) ;
#32847 = ORIENTED_EDGE ( 'NONE', *, *, #29905, .T. ) ;
#32848 = CARTESIAN_POINT ( 'NONE',  ( 0.000000000000000000, 0.000000000000000000, -0.3851141460153411078 ) ) ;
#32849 = FACE_BOUND ( 'NONE', #28313, .T. ) ;
#32850 = DIRECTION ( 'NONE',  ( 1.000000000000000000, 0.000000000000000000, 0.000000000000000000 ) ) ;
#32851 = DIRECTION ( 'NONE',  ( 0.000000000000000000, 0.000000000000000000, 1.000000000000000000 ) ) ;
#32852 = DIRECTION ( 'NONE',  ( 0.000000000000000000, 0.000000000000000000, 1.000000000000000000 ) ) ;
#32853 = VERTEX_POINT ( 'NONE', #12817 ) ;
#32854 = CARTESIAN_POINT ( 'NONE',  ( 0.000000000000000000, 0.000000000000000000, 2.266666666667000563 ) ) ;
#32855 = PRODUCT_DEFINITION_SHAPE ( 'NONE', 'NONE',  #37128 ) ;
#32856 = CARTESIAN_POINT ( 'NONE',  ( 59.99999662536845335, 34.64101615137759893, -9.999999999999998224 ) ) ;
#32857 = AXIS2_PLACEMENT_3D ( 'NONE', #24965, #31130, #33590 ) ;
#32858 = FACE_OUTER_BOUND ( 'NONE', #3490, .T. ) ;
#32859 = VERTEX_POINT ( 'NONE', #27639 ) ;
#32860 = CARTESIAN_POINT ( 'NONE',  ( 62.99999662536842493, 43.30127018922200222, 12.50000000000000000 ) ) ;
#32861 = AXIS2_PLACEMENT_3D ( 'NONE', #1758, #4572, #35353 ) ;
#32862 = CARTESIAN_POINT ( 'NONE',  ( -52.39915983220772233, -35.19434990244957362, -49.22241343995298024 ) ) ;
#32863 = EDGE_CURVE ( 'NONE', #19047, #33610, #15328, .T. ) ;
#32864 = VERTEX_POINT ( 'NONE', #7583 ) ;
#32865 = ORIENTED_EDGE ( 'NONE', *, *, #31811, .T. ) ;
#32866 = AXIS2_PLACEMENT_3D ( 'NONE', #15063, #20877, #26489 ) ;
#32867 = CARTESIAN_POINT ( 'NONE',  ( -47.63139720814438505, -27.49999999999955591, -5.000000000000000888 ) ) ;
#32868 = LINE ( 'NONE', #3991, #26543 ) ;
#32869 = CARTESIAN_POINT ( 'NONE',  ( -68.00000000000000000, 0.000000000000000000, -4.999999999999997335 ) ) ;
#32870 = ORIENTED_EDGE ( 'NONE', *, *, #8541, .T. ) ;
#32871 = EDGE_LOOP ( 'NONE', ( #36840, #16469, #23851, #8318, #30576, #12750, #2855, #36092, #18662, #24681, #29983, #20292 ) ) ;
#32872 = EDGE_LOOP ( 'NONE', ( #36095, #10427, #21879, #14692 ) ) ;
#32873 = AXIS2_PLACEMENT_3D ( 'NONE', #23978, #9143, #32208 ) ;
#32874 = VECTOR ( 'NONE', #25370, 1000.000000000000000 ) ;
#32875 = CARTESIAN_POINT ( 'NONE',  ( -55.88972745734155012, 34.00000000000049027, -4.999999999999997335 ) ) ;
#32876 = CIRCLE ( 'NONE', #31077, 5.750000000000005329 ) ;
#32877 = ORIENTED_EDGE ( 'NONE', *, *, #22966, .F. ) ;
#32878 = ORIENTED_EDGE ( 'NONE', *, *, #3882, .T. ) ;
#32879 = CARTESIAN_POINT ( 'NONE',  ( -58.00000337463107059, -34.64101615137762025, -9.999999999999998224 ) ) ;
#32880 = EDGE_LOOP ( 'NONE', ( #10865, #30751, #35903, #726, #26063 ) ) ;
#32881 = ORIENTED_EDGE ( 'NONE', *, *, #150, .T. ) ;
#32882 = DIRECTION ( 'NONE',  ( 1.000000000000000000, 0.000000000000000000, 0.000000000000000000 ) ) ;
#32883 = CIRCLE ( 'NONE', #15515, 2.000000000000001776 ) ;
#32884 = DIRECTION ( 'NONE',  ( -0.000000000000000000, -0.000000000000000000, 1.000000000000000000 ) ) ;
#32885 = EDGE_CURVE ( 'NONE', #5353, #10671, #15475, .T. ) ;
#32886 = VERTEX_POINT ( 'NONE', #16222 ) ;
#32887 = VERTEX_POINT ( 'NONE', #4032 ) ;
#32888 = CARTESIAN_POINT ( 'NONE',  ( 65.44550000000002399, 3.673940397442060361E-16, -3.000000000000000444 ) ) ;
#32889 = CARTESIAN_POINT ( 'NONE',  ( 14.99999662536859901, 77.94228634059957983, 12.50000000000000000 ) ) ;
#32890 = DIRECTION ( 'NONE',  ( 0.000000000000000000, 0.000000000000000000, 1.000000000000000000 ) ) ;
#32891 = ORIENTED_EDGE ( 'NONE', *, *, #5981, .T. ) ;
#32892 = CARTESIAN_POINT ( 'NONE',  ( -6.123233995736731770E-16, 145.0000000000000568, 27.50000000000000000 ) ) ;
#32893 = AXIS2_PLACEMENT_3D ( 'NONE', #4047, #15287, #15487 ) ;
#32894 = VERTEX_POINT ( 'NONE', #18660 ) ;
#32895 = DIRECTION ( 'NONE',  ( 0.000000000000000000, 0.000000000000000000, 1.000000000000000000 ) ) ;
#32896 = DIRECTION ( 'NONE',  ( 1.000000000000000000, 0.000000000000000000, 0.000000000000000000 ) ) ;
#32897 = CARTESIAN_POINT ( 'NONE',  ( 95.00000000000000000, 1.163414459189985643E-14, 17.49999999999999645 ) ) ;
#32898 = DIRECTION ( 'NONE',  ( 0.000000000000000000, 0.000000000000000000, 1.000000000000000000 ) ) ;
#32899 = AXIS2_PLACEMENT_3D ( 'NONE', #25990, #5400, #8564 ) ;
#32900 = DIRECTION ( 'NONE',  ( 1.000000000000000000, 0.000000000000000000, 0.000000000000000000 ) ) ;
#32901 = CIRCLE ( 'NONE', #11348, 3.500000000000003109 ) ;
#32902 = CARTESIAN_POINT ( 'NONE',  ( 111.8061974404898962, 19.22934205794938478, 32.50000000000000000 ) ) ;
#32903 = PLANE ( 'NONE',  #24132 ) ;
#32904 = AXIS2_PLACEMENT_3D ( 'NONE', #21464, #7394, #9657 ) ;
#32905 = ORIENTED_EDGE ( 'NONE', *, *, #23329, .T. ) ;
#32906 = CARTESIAN_POINT ( 'NONE',  ( 71.99999662536839651, 34.64101615137758472, 12.50000000000000000 ) ) ;
#32907 = DIRECTION ( 'NONE',  ( 1.000000000000000000, 0.000000000000000000, 0.000000000000000000 ) ) ;
#32908 = DIRECTION ( 'NONE',  ( 0.000000000000000000, 0.000000000000000000, -1.000000000000000000 ) ) ;
#32909 = EDGE_CURVE ( 'NONE', #35698, #27018, #21921, .T. ) ;
#32910 = VERTEX_POINT ( 'NONE', #30079 ) ;
#32911 = VERTEX_POINT ( 'NONE', #4402 ) ;
#32912 = ORIENTED_EDGE ( 'NONE', *, *, #717, .T. ) ;
#32913 = AXIS2_PLACEMENT_3D ( 'NONE', #3864, #21117, #1426 ) ;
#32914 = FACE_OUTER_BOUND ( 'NONE', #34391, .T. ) ;
#32915 = DIRECTION ( 'NONE',  ( -1.000000000000000000, 0.000000000000000000, 0.000000000000000000 ) ) ;
#32916 = DIRECTION ( 'NONE',  ( -0.000000000000000000, -0.000000000000000000, 1.000000000000000000 ) ) ;
#32917 = ADVANCED_FACE ( 'NONE', ( #33470 ), #14120, .F. ) ;
#32918 = AXIS2_PLACEMENT_3D ( 'NONE', #25453, #11201, #11555 ) ;
#32919 = ORIENTED_EDGE ( 'NONE', *, *, #14017, .T. ) ;
#32920 = LINE ( 'NONE', #27091, #28097 ) ;
#32921 = EDGE_CURVE ( 'NONE', #16940, #13964, #2759, .T. ) ;
#32922 = LINE ( 'NONE', #13034, #14716 ) ;
#32923 = ORIENTED_EDGE ( 'NONE', *, *, #9990, .F. ) ;
#32924 = CARTESIAN_POINT ( 'NONE',  ( 44.13139720814400135, -27.50000000000022737, -5.000000000000000888 ) ) ;
#32925 = ORIENTED_EDGE ( 'NONE', *, *, #25251, .F. ) ;
#32926 = CARTESIAN_POINT ( 'NONE',  ( 4.390739357591696154E-15, -5.773502691896305272, -5.700000000000000178 ) ) ;
#32927 = AXIS2_PLACEMENT_3D ( 'NONE', #8152, #22953, #19596 ) ;
#32928 = AXIS2_PLACEMENT_3D ( 'NONE', #29176, #15112, #3683 ) ;
#32929 = FACE_OUTER_BOUND ( 'NONE', #23731, .T. ) ;
#32930 = DIRECTION ( 'NONE',  ( 0.000000000000000000, 0.000000000000000000, -1.000000000000000000 ) ) ;
#32931 = VECTOR ( 'NONE', #18979, 1000.000000000000000 ) ;
#32932 = EDGE_CURVE ( 'NONE', #32411, #13754, #25772, .T. ) ;
#32933 = ORIENTED_EDGE ( 'NONE', *, *, #35507, .F. ) ;
#32934 = DIRECTION ( 'NONE',  ( -0.000000000000000000, -0.000000000000000000, 1.000000000000000000 ) ) ;
#32935 = CIRCLE ( 'NONE', #31708, 2.000000000000001776 ) ;
#32936 = SHAPE_DEFINITION_REPRESENTATION ( #14547, #6396 ) ;
#32937 = DIRECTION ( 'NONE',  ( 1.000000000000000000, 0.000000000000000000, 0.000000000000000000 ) ) ;
#32938 = CIRCLE ( 'NONE', #34739, 2.000000000000001776 ) ;
#32939 = DIRECTION ( 'NONE',  ( 0.000000000000000000, 0.000000000000000000, 1.000000000000000000 ) ) ;
#32940 = DIRECTION ( 'NONE',  ( 0.000000000000000000, 0.000000000000000000, -1.000000000000000000 ) ) ;
#32941 = EDGE_LOOP ( 'NONE', ( #15107, #30027 ) ) ;
#32942 = CARTESIAN_POINT ( 'NONE',  ( -104.8061974404900241, -19.22934205794863516, 32.50000000000000000 ) ) ;
#32943 = AXIS2_PLACEMENT_3D ( 'NONE', #5924, #5175, #16612 ) ;
#32944 = DIRECTION ( 'NONE',  ( 0.000000000000000000, 0.000000000000000000, 1.000000000000000000 ) ) ;
#32945 = DIRECTION ( 'NONE',  ( 1.000000000000000000, 0.000000000000000000, 0.000000000000000000 ) ) ;
#32946 = EDGE_CURVE ( 'NONE', #10255, #36868, #33918, .T. ) ;
#32947 = VERTEX_POINT ( 'NONE', #31012 ) ;
#32948 = EDGE_CURVE ( 'NONE', #21723, #29660, #4559, .T. ) ;
#32949 = EDGE_LOOP ( 'NONE', ( #4889, #32517, #284, #18091 ) ) ;
#32950 = CARTESIAN_POINT ( 'NONE',  ( 36.99999662536855283, -60.62177826491080168, -9.999999999999998224 ) ) ;
#32951 = DIRECTION ( 'NONE',  ( -0.000000000000000000, -0.000000000000000000, 1.000000000000000000 ) ) ;
#32952 = AXIS2_PLACEMENT_3D ( 'NONE', #21941, #36025, #27577 ) ;
#32953 = DIRECTION ( 'NONE',  ( 0.000000000000000000, 0.000000000000000000, -1.000000000000000000 ) ) ;
#32954 = ORIENTED_EDGE ( 'NONE', *, *, #14566, .T. ) ;
#32955 = DIRECTION ( 'NONE',  ( 0.000000000000000000, 0.000000000000000000, 1.000000000000000000 ) ) ;
#32956 = CARTESIAN_POINT ( 'NONE',  ( 16.99999662536859901, 77.94228634059957983, -9.999999999999998224 ) ) ;
#32957 = EDGE_CURVE ( 'NONE', #5293, #28159, #9327, .T. ) ;
#32958 = DIRECTION ( 'NONE',  ( -1.000000000000000000, 0.000000000000000000, 0.000000000000000000 ) ) ;
#32959 = CARTESIAN_POINT ( 'NONE',  ( -79.75042228122002541, 72.37693729083288474, 32.50000000000000000 ) ) ;
#32960 = EDGE_LOOP ( 'NONE', ( #29276, #8428 ) ) ;
#32961 = ORIENTED_EDGE ( 'NONE', *, *, #3236, .T. ) ;
#32962 = DIRECTION ( 'NONE',  ( 0.000000000000000000, 0.000000000000000000, 1.000000000000000000 ) ) ;
#32963 = EDGE_CURVE ( 'NONE', #24230, #28140, #5170, .T. ) ;
#32964 = CARTESIAN_POINT ( 'NONE',  ( 9.999996625368618552, 69.28203230275516944, -9.999999999999998224 ) ) ;
#32965 = ORIENTED_EDGE ( 'NONE', *, *, #21442, .T. ) ;
#32966 = CARTESIAN_POINT ( 'NONE',  ( 0.1702248550645389935, -5.871782057790579934, -4.289066185948700038 ) ) ;
#32967 = ORIENTED_EDGE ( 'NONE', *, *, #4474, .F. ) ;
#32968 = CARTESIAN_POINT ( 'NONE',  ( -42.97377950131527058, 96.90768712682508124, 27.49999999999999645 ) ) ;
#32969 = DIRECTION ( 'NONE',  ( 0.000000000000000000, 0.000000000000000000, 1.000000000000000000 ) ) ;
#32970 = ORIENTED_EDGE ( 'NONE', *, *, #19858, .T. ) ;
#32971 = EDGE_LOOP ( 'NONE', ( #24727, #2530, #6676, #36044, #20880 ) ) ;
#32972 = DIRECTION ( 'NONE',  ( 1.000000000000000000, 0.000000000000000000, 0.000000000000000000 ) ) ;
#32973 = EDGE_LOOP ( 'NONE', ( #23420, #35645, #9078, #31803 ) ) ;
#32974 = CARTESIAN_POINT ( 'NONE',  ( 0.000000000000000000, 0.000000000000000000, -5.000000000000000000 ) ) ;
#32975 = EDGE_CURVE ( 'NONE', #29715, #34191, #12827, .T. ) ;
#32976 = CARTESIAN_POINT ( 'NONE',  ( 59.99999662536842493, -51.96152422706639840, -9.999999999999998224 ) ) ;
#32977 = FACE_OUTER_BOUND ( 'NONE', #17272, .T. ) ;
#32978 = AXIS2_PLACEMENT_3D ( 'NONE', #29602, #3927, #15371 ) ;
#32979 = ORIENTED_EDGE ( 'NONE', *, *, #13642, .F. ) ;
#32980 = DIRECTION ( 'NONE',  ( 0.000000000000000000, 0.000000000000000000, 1.000000000000000000 ) ) ;
#32981 = CARTESIAN_POINT ( 'NONE',  ( -107.2742589609544410, 47.50000425637879431, 32.50001250000000397 ) ) ;
#32982 = ORIENTED_EDGE ( 'NONE', *, *, #16804, .T. ) ;
#32983 = EDGE_CURVE ( 'NONE', #34152, #1959, #24930, .T. ) ;
#32984 = ORIENTED_EDGE ( 'NONE', *, *, #11463, .T. ) ;
#32985 = VERTEX_POINT ( 'NONE', #19386 ) ;
#32986 = DIRECTION ( 'NONE',  ( 0.000000000000000000, 0.000000000000000000, -1.000000000000000000 ) ) ;
#32987 = EDGE_CURVE ( 'NONE', #13225, #8340, #34216, .T. ) ;
#32988 = CARTESIAN_POINT ( 'NONE',  ( 64.99999662536839651, -43.30127018922199511, -9.999999999999998224 ) ) ;
#32989 = ORIENTED_EDGE ( 'NONE', *, *, #17155, .F. ) ;
#32990 = CARTESIAN_POINT ( 'NONE',  ( -94.40806000769299544, 12.15049814296761888, 32.50000000000000000 ) ) ;
#32991 = DIRECTION ( 'NONE',  ( -1.000000000000000000, 0.000000000000000000, 0.000000000000000000 ) ) ;
#32992 = EDGE_LOOP ( 'NONE', ( #20777, #18215, #35865, #33292 ) ) ;
#32993 = CARTESIAN_POINT ( 'NONE',  ( 0.000000000000000000, 0.000000000000000000, -15.00000000000000000 ) ) ;
#32994 = DIRECTION ( 'NONE',  ( -1.000000000000000000, 0.000000000000000000, -0.000000000000000000 ) ) ;
#32995 = CARTESIAN_POINT ( 'NONE',  ( -47.63139720814380951, 27.50000000000055422, 5.000000000000000888 ) ) ;
#32996 = DIRECTION ( 'NONE',  ( -1.000000000000000000, 0.000000000000000000, 0.000000000000000000 ) ) ;
#32997 = CARTESIAN_POINT ( 'NONE',  ( -48.00000337463112032, -51.96152422706641971, -9.999999999999998224 ) ) ;
#32998 = DIRECTION ( 'NONE',  ( 1.000000000000000000, 0.000000000000000000, 0.000000000000000000 ) ) ;
#32999 = ORIENTED_EDGE ( 'NONE', *, *, #10234, .T. ) ;
#33000 = EDGE_LOOP ( 'NONE', ( #33788, #26127, #35617 ) ) ;
#33001 = LINE ( 'NONE', #24942, #34426 ) ;
#33002 = EDGE_CURVE ( 'NONE', #5488, #1395, #23719, .T. ) ;
#33003 = CARTESIAN_POINT ( 'NONE',  ( 19.99999662536861678, -86.60254037844400443, 12.50000000000000000 ) ) ;
#33004 = DIRECTION ( 'NONE',  ( 0.000000000000000000, 0.000000000000000000, -1.000000000000000000 ) ) ;
#33005 = DIRECTION ( 'NONE',  ( 0.000000000000000000, 0.000000000000000000, 1.000000000000000000 ) ) ;
#33006 = VERTEX_POINT ( 'NONE', #22025 ) ;
#33007 = FACE_OUTER_BOUND ( 'NONE', #20885, .T. ) ;
#33008 = CARTESIAN_POINT ( 'NONE',  ( -60.00000337463107059, -34.64101615137762025, 12.50000000000000000 ) ) ;
#33009 = DIRECTION ( 'NONE',  ( -0.000000000000000000, -0.000000000000000000, -1.000000000000000000 ) ) ;
#33010 = EDGE_LOOP ( 'NONE', ( #33359, #24033 ) ) ;
#33011 = FACE_OUTER_BOUND ( 'NONE', #3638, .T. ) ;
#33012 = ORIENTED_EDGE ( 'NONE', *, *, #2027, .T. ) ;
#33013 = SURFACE_SIDE_STYLE ('',( #9638 ) ) ;
#33014 = DIRECTION ( 'NONE',  ( 0.000000000000000000, 0.000000000000000000, 1.000000000000000000 ) ) ;
#33015 = SHAPE_REPRESENTATION ( 'socket head cap screw_iso_ISO 4762 M6 x 60 - 24N', ( #21385 ), #2251 ) ;
#33016 = CARTESIAN_POINT ( 'NONE',  ( 47.99999662536848177, -51.96152422706640550, 12.50000000000000000 ) ) ;
#33017 = EDGE_CURVE ( 'NONE', #25535, #24313, #4951, .T. ) ;
#33018 = CARTESIAN_POINT ( 'NONE',  ( -30.00000337463118427, 69.28203230275516944, -9.999999999999998224 ) ) ;
#33019 = ORIENTED_EDGE ( 'NONE', *, *, #1639, .F. ) ;
#33020 = EDGE_CURVE ( 'NONE', #28380, #167, #26118, .T. ) ;
#33021 = ORIENTED_EDGE ( 'NONE', *, *, #18244, .F. ) ;
#33022 = VECTOR ( 'NONE', #33175, 1000.000000000000000 ) ;
#33023 = EDGE_CURVE ( 'NONE', #27930, #36161, #14741, .T. ) ;
#33024 = EDGE_LOOP ( 'NONE', ( #31666, #4866 ) ) ;
#33025 = CARTESIAN_POINT ( 'NONE',  ( 52.39915983220795681, 35.19434990244919703, 12.49999999999999822 ) ) ;
#33026 = DIRECTION ( 'NONE',  ( 0.000000000000000000, 0.000000000000000000, 1.000000000000000000 ) ) ;
#33027 = ADVANCED_FACE ( 'NONE', ( #5513 ), #28016, .F. ) ;
#33028 = CYLINDRICAL_SURFACE ( 'NONE', #2892, 2.000000000000001776 ) ;
#33029 = LINE ( 'NONE', #1904, #12105 ) ;
#33030 = DIRECTION ( 'NONE',  ( 1.000000000000000000, 0.000000000000000000, 0.000000000000000000 ) ) ;
#33031 = EDGE_CURVE ( 'NONE', #6351, #2856, #29104, .T. ) ;
#33032 = ORIENTED_EDGE ( 'NONE', *, *, #6043, .T. ) ;
#33033 = DIRECTION ( 'NONE',  ( 0.000000000000000000, 0.000000000000000000, -1.000000000000000000 ) ) ;
#33034 = CARTESIAN_POINT ( 'NONE',  ( 37.50000000000000000, -103.4105893997321743, 32.50000000000000000 ) ) ;
#33035 = EDGE_LOOP ( 'NONE', ( #12533, #21507, #31250 ) ) ;
#33036 = LINE ( 'NONE', #13520, #7655 ) ;
#33037 = DIRECTION ( 'NONE',  ( 0.6439740589782694258, 0.7650473262243666639, 0.000000000000000000 ) ) ;
#33038 = EDGE_CURVE ( 'NONE', #30836, #33241, #2516, .T. ) ;
#33039 = ORIENTED_EDGE ( 'NONE', *, *, #27532, .T. ) ;
#33040 = ADVANCED_FACE ( 'NONE', ( #11120 ), #22569, .F. ) ;
#33041 = EDGE_LOOP ( 'NONE', ( #10872, #25389, #28281, #6295 ) ) ;
#33042 = EDGE_CURVE ( 'NONE', #29078, #9029, #3242, .T. ) ;
#33043 = CIRCLE ( 'NONE', #15084, 2.000000000000001776 ) ;
#33044 = ADVANCED_FACE ( 'NONE', ( #3622, #32090, #11660, #6230, #5890, #9051, #15050, #26665, #18045 ), #23315, .F. ) ;
#33045 = DIRECTION ( 'NONE',  ( 0.000000000000000000, 0.000000000000000000, 1.000000000000000000 ) ) ;
#33046 = CARTESIAN_POINT ( 'NONE',  ( -6.532899837730827386, 8.119260925317680943E-16, -5.700000000000001066 ) ) ;
#33047 = CARTESIAN_POINT ( 'NONE',  ( -105.2710652963492208, -37.58057717672379994, 32.50000000000000711 ) ) ;
#33048 = ORIENTED_EDGE ( 'NONE', *, *, #30932, .F. ) ;
#33049 = ORIENTED_EDGE ( 'NONE', *, *, #7395, .T. ) ;
#33050 = VERTEX_POINT ( 'NONE', #14666 ) ;
#33051 = FACE_OUTER_BOUND ( 'NONE', #11617, .T. ) ;
#33052 = EDGE_LOOP ( 'NONE', ( #36789, #1872 ) ) ;
#33053 = ORIENTED_EDGE ( 'NONE', *, *, #24026, .F. ) ;
#33054 = FACE_BOUND ( 'NONE', #29170, .T. ) ;
#33055 = ORIENTED_EDGE ( 'NONE', *, *, #8229, .T. ) ;
#33056 = ORIENTED_EDGE ( 'NONE', *, *, #20630, .F. ) ;
#33057 = DIRECTION ( 'NONE',  ( 1.000000000000000000, 0.000000000000000000, 0.000000000000000000 ) ) ;
#33058 = FACE_OUTER_BOUND ( 'NONE', #2289, .T. ) ;
#33059 = VERTEX_POINT ( 'NONE', #26113 ) ;
#33060 = ORIENTED_EDGE ( 'NONE', *, *, #25628, .F. ) ;
#33061 = CYLINDRICAL_SURFACE ( 'NONE', #1733, 2.000000000000001776 ) ;
#33062 = DIRECTION ( 'NONE',  ( 0.000000000000000000, 0.000000000000000000, 1.000000000000000000 ) ) ;
#33063 = DIRECTION ( 'NONE',  ( 0.000000000000000000, 0.000000000000000000, 1.000000000000000000 ) ) ;
#33064 = CARTESIAN_POINT ( 'NONE',  ( -5.238715782502663565, 1.018209582082210352, -4.086015505371660694 ) ) ;
#33065 = VERTEX_POINT ( 'NONE', #31733 ) ;
#33066 = DIRECTION ( 'NONE',  ( 1.000000000000000000, 0.000000000000000000, 0.000000000000000000 ) ) ;
#33067 = CIRCLE ( 'NONE', #16298, 2.000000000000001776 ) ;
#33068 = VERTEX_POINT ( 'NONE', #15222 ) ;
#33069 = DIRECTION ( 'NONE',  ( 1.000000000000000000, 0.000000000000000000, 0.000000000000000000 ) ) ;
#33070 = FACE_OUTER_BOUND ( 'NONE', #4745, .T. ) ;
#33071 = DIRECTION ( 'NONE',  ( 0.000000000000000000, 0.000000000000000000, 1.000000000000000000 ) ) ;
#33072 = CARTESIAN_POINT ( 'NONE',  ( 47.63139720814400846, -27.50000000000022737, -10.00000000000000000 ) ) ;
#33073 = DIRECTION ( 'NONE',  ( 0.000000000000000000, 0.000000000000000000, 1.000000000000000000 ) ) ;
#33074 = DIRECTION ( 'NONE',  ( 0.000000000000000000, 0.000000000000000000, 1.000000000000000000 ) ) ;
#33075 = DIRECTION ( 'NONE',  ( -0.000000000000000000, -0.000000000000000000, 1.000000000000000000 ) ) ;
#33076 = EDGE_LOOP ( 'NONE', ( #24194, #33828, #7924, #14054 ) ) ;
#33077 = DIRECTION ( 'NONE',  ( -0.000000000000000000, -0.000000000000000000, 1.000000000000000000 ) ) ;
#33078 = DIRECTION ( 'NONE',  ( 1.000000000000000000, 0.000000000000000000, 0.000000000000000000 ) ) ;
#33079 = CARTESIAN_POINT ( 'NONE',  ( -43.00000337463112743, -60.62177826491080168, 12.50000000000000000 ) ) ;
#33080 = VERTEX_POINT ( 'NONE', #11495 ) ;
#33081 = AXIS2_PLACEMENT_3D ( 'NONE', #12412, #32476, #14505 ) ;
#33082 = VERTEX_POINT ( 'NONE', #23119 ) ;
#33083 = EDGE_LOOP ( 'NONE', ( #866, #34456, #13977, #12137 ) ) ;
#33084 = EDGE_CURVE ( 'NONE', #23027, #25033, #9428, .T. ) ;
#33085 = DIRECTION ( 'NONE',  ( 0.000000000000000000, -0.000000000000000000, -1.000000000000000000 ) ) ;
#33086 = CYLINDRICAL_SURFACE ( 'NONE', #31615, 2.000000000000000000 ) ;
#33087 = EDGE_LOOP ( 'NONE', ( #33154, #34275, #37059, #9091 ) ) ;
#33088 = DIRECTION ( 'NONE',  ( 0.000000000000000000, 0.000000000000000000, 1.000000000000000000 ) ) ;
#33089 = CIRCLE ( 'NONE', #19923, 95.00000000000001421 ) ;
#33090 = CYLINDRICAL_SURFACE ( 'NONE', #23716, 1.999999999999998224 ) ;
#33091 = VERTEX_POINT ( 'NONE', #786 ) ;
#33092 = CIRCLE ( 'NONE', #11537, 2.000000000000001776 ) ;
#33093 = PLANE ( 'NONE',  #36524 ) ;
#33094 = VERTEX_POINT ( 'NONE', #25936 ) ;
#33095 = FACE_OUTER_BOUND ( 'NONE', #10463, .T. ) ;
#33096 = CYLINDRICAL_SURFACE ( 'NONE', #33358, 1.999999999999998224 ) ;
#33097 = DIRECTION ( 'NONE',  ( 1.000000000000000000, 0.000000000000000000, 0.000000000000000000 ) ) ;
#33098 = DIRECTION ( 'NONE',  ( 1.000000000000000000, 0.000000000000000000, 0.000000000000000000 ) ) ;
#33099 = EDGE_LOOP ( 'NONE', ( #4801, #9600, #27079, #6158 ) ) ;
#33100 = DIRECTION ( 'NONE',  ( 1.000000000000000000, 0.000000000000000000, 0.000000000000000000 ) ) ;
#33101 = EDGE_CURVE ( 'NONE', #23066, #1626, #23747, .T. ) ;
#33102 = ITEM_DEFINED_TRANSFORMATION ( 'NONE', 'NONE', #13560,  #21385 ) ;
#33103 = EDGE_CURVE ( 'NONE', #7750, #22308, #33331, .T. ) ;
#33104 = DIRECTION ( 'NONE',  ( 0.000000000000000000, 0.4999999999999959477, -0.8660254037844409281 ) ) ;
#33105 = FACE_OUTER_BOUND ( 'NONE', #75, .T. ) ;
#33106 = AXIS2_PLACEMENT_3D ( 'NONE', #17823, #20819, #29055 ) ;
#33107 = DIRECTION ( 'NONE',  ( 0.000000000000000000, 0.000000000000000000, 1.000000000000000000 ) ) ;
#33108 = DIRECTION ( 'NONE',  ( 1.000000000000000000, 0.000000000000000000, 0.000000000000000000 ) ) ;
#33109 = VERTEX_POINT ( 'NONE', #34761 ) ;
#33110 = DIRECTION ( 'NONE',  ( 0.000000000000000000, 0.000000000000000000, 1.000000000000000000 ) ) ;
#33111 = CARTESIAN_POINT ( 'NONE',  ( 4.279621169095998212, -62.97617850287780072, -49.86561046011506448 ) ) ;
#33112 = CARTESIAN_POINT ( 'NONE',  ( 36.99999662536853862, 77.94228634059959404, 12.50000000000000000 ) ) ;
#33113 = EDGE_CURVE ( 'NONE', #23645, #16885, #35120, .T. ) ;
#33114 = EDGE_LOOP ( 'NONE', ( #4965, #8220, #18636, #18657, #34231 ) ) ;
#33115 = VECTOR ( 'NONE', #29151, 1000.000000000000000 ) ;
#33116 = ORIENTED_EDGE ( 'NONE', *, *, #32220, .T. ) ;
#33117 = DIRECTION ( 'NONE',  ( 0.000000000000000000, 0.000000000000000000, 1.000000000000000000 ) ) ;
#33118 = CARTESIAN_POINT ( 'NONE',  ( -45.00000337463111322, 77.94228634059959404, -9.999999999999998224 ) ) ;
#33119 = DIRECTION ( 'NONE',  ( 1.000000000000000000, 0.000000000000000000, 0.000000000000000000 ) ) ;
#33120 = ORIENTED_EDGE ( 'NONE', *, *, #20497, .F. ) ;
#33121 = EDGE_CURVE ( 'NONE', #15905, #9326, #8198, .T. ) ;
#33122 = DIRECTION ( 'NONE',  ( 0.000000000000000000, 0.000000000000000000, 1.000000000000000000 ) ) ;
#33123 = FACE_OUTER_BOUND ( 'NONE', #36112, .T. ) ;
#33124 = CARTESIAN_POINT ( 'NONE',  ( 34.99999662536855283, -77.94228634059960825, -5.000000000000000000 ) ) ;
#33125 = AXIS2_PLACEMENT_3D ( 'NONE', #28565, #16949, #17494 ) ;
#33126 = CARTESIAN_POINT ( 'NONE',  ( -73.90204618161054384, 6.988581222280664917, -5.000000000000000000 ) ) ;
#33127 = ORIENTED_EDGE ( 'NONE', *, *, #26715, .F. ) ;
#33128 = ORIENTED_EDGE ( 'NONE', *, *, #13642, .T. ) ;
#33129 = AXIS2_PLACEMENT_3D ( 'NONE', #26225, #14417, #535 ) ;
#33130 = DIRECTION ( 'NONE',  ( -0.7071067811865439090, 0.7071067811865512365, 0.000000000000000000 ) ) ;
#33131 = DIRECTION ( 'NONE',  ( 0.000000000000000000, 0.000000000000000000, -1.000000000000000000 ) ) ;
#33132 = ORIENTED_EDGE ( 'NONE', *, *, #28335, .T. ) ;
#33133 = PLANE ( 'NONE',  #5975 ) ;
#33134 = ORIENTED_EDGE ( 'NONE', *, *, #1079, .T. ) ;
#33135 = CARTESIAN_POINT ( 'NONE',  ( -35.19434990244938888, 52.39915983220783602, -4.999999999999997335 ) ) ;
#33136 = AXIS2_PLACEMENT_3D ( 'NONE', #2596, #17024, #16248 ) ;
#33137 = DIRECTION ( 'NONE',  ( 1.000000000000000000, 0.000000000000000000, 0.000000000000000000 ) ) ;
#33138 = ORIENTED_EDGE ( 'NONE', *, *, #5717, .T. ) ;
#33139 = CIRCLE ( 'NONE', #27755, 2.000000000000001776 ) ;
#33140 = EDGE_CURVE ( 'NONE', #12474, #20714, #27352, .T. ) ;
#33141 = DIRECTION ( 'NONE',  ( -1.000000000000000000, 0.000000000000000000, 0.000000000000000000 ) ) ;
#33142 = ORIENTED_EDGE ( 'NONE', *, *, #2765, .F. ) ;
#33143 = EDGE_CURVE ( 'NONE', #10852, #30836, #21354, .T. ) ;
#33144 = VECTOR ( 'NONE', #29155, 1000.000000000000000 ) ;
#33145 = CARTESIAN_POINT ( 'NONE',  ( 67.99999662536836809, -34.64101615137759183, 17.49999999999999645 ) ) ;
#33146 = CARTESIAN_POINT ( 'NONE',  ( 1.999996625368710257, -69.28203230275519786, -9.999999999999998224 ) ) ;
#33147 = DIRECTION ( 'NONE',  ( 0.000000000000000000, 0.000000000000000000, 1.000000000000000000 ) ) ;
#33148 = VERTEX_POINT ( 'NONE', #29467 ) ;
#33149 = DIRECTION ( 'NONE',  ( 0.5000000000000038858, 0.8660254037844363761, 0.000000000000000000 ) ) ;
#33150 = EDGE_CURVE ( 'NONE', #8319, #4953, #28911, .T. ) ;
#33151 = AXIS2_PLACEMENT_3D ( 'NONE', #19187, #13527, #10737 ) ;
#33152 = DIRECTION ( 'NONE',  ( -1.000000000000000000, 0.000000000000000000, 0.000000000000000000 ) ) ;
#33153 = CARTESIAN_POINT ( 'NONE',  ( 31.02796211690949235, -59.29837256189548356, -4.999999999999997335 ) ) ;
#33154 = ORIENTED_EDGE ( 'NONE', *, *, #20307, .F. ) ;
#33155 = ORIENTED_EDGE ( 'NONE', *, *, #34019, .F. ) ;
#33156 = AXIS2_PLACEMENT_3D ( 'NONE', #23407, #4836, #21518 ) ;
#33157 = EDGE_CURVE ( 'NONE', #4442, #15311, #5199, .T. ) ;
#33158 = EDGE_LOOP ( 'NONE', ( #29651, #28976, #33177, #20610, #30437, #2702, #11534 ) ) ;
#33159 = DIRECTION ( 'NONE',  ( 1.000000000000000000, 0.000000000000000000, 0.000000000000000000 ) ) ;
#33160 = ORIENTED_EDGE ( 'NONE', *, *, #2164, .T. ) ;
#33161 = CARTESIAN_POINT ( 'NONE',  ( 0.000000000000000000, 0.000000000000000000, 2.266666666666999674 ) ) ;
#33162 = CARTESIAN_POINT ( 'NONE',  ( 42.97377950131529190, 96.90768712682505281, -11.00000000000000000 ) ) ;
#33163 = VECTOR ( 'NONE', #4424, 1000.000000000000000 ) ;
#33164 = CARTESIAN_POINT ( 'NONE',  ( -70.47608876694631874, -59.13646009116124702, 12.49999999999999822 ) ) ;
#33165 = CIRCLE ( 'NONE', #833, 27.00000000000001421 ) ;
#33166 = DIRECTION ( 'NONE',  ( 1.000000000000000000, 0.000000000000000000, 0.000000000000000000 ) ) ;
#33167 = DIRECTION ( 'NONE',  ( 1.000000000000000000, 0.000000000000000000, 0.000000000000000000 ) ) ;
#33168 = CARTESIAN_POINT ( 'NONE',  ( -69.13212189986965939, -2.778182860042805125, -4.999999999999997335 ) ) ;
#33169 = DIRECTION ( 'NONE',  ( 1.000000000000000000, 0.000000000000000000, 0.000000000000000000 ) ) ;
#33170 = ORIENTED_EDGE ( 'NONE', *, *, #21867, .T. ) ;
#33171 = ORIENTED_EDGE ( 'NONE', *, *, #26597, .F. ) ;
#33172 = EDGE_CURVE ( 'NONE', #15802, #17855, #30698, .T. ) ;
#33173 = SURFACE_STYLE_FILL_AREA ( #10139 ) ;
#33174 = CYLINDRICAL_SURFACE ( 'NONE', #169, 2.000000000000001776 ) ;
#33175 = DIRECTION ( 'NONE',  ( 0.000000000000000000, 0.000000000000000000, 1.000000000000000000 ) ) ;
#33176 = LINE ( 'NONE', #24754, #31076 ) ;
#33177 = ORIENTED_EDGE ( 'NONE', *, *, #15358, .T. ) ;
#33178 = UNCERTAINTY_MEASURE_WITH_UNIT (LENGTH_MEASURE( 1.000000000000000082E-05 ), #285, 'distance_accuracy_value', 'NONE');
#33179 = ADVANCED_FACE ( 'NONE', ( #21419, #21778, #26864, #30412, #18428, #30034, #23875 ), #12597, .F. ) ;
#33180 = PLANE ( 'NONE',  #11732 ) ;
#33181 = CARTESIAN_POINT ( 'NONE',  ( 56.67878100130369035, -27.78182860042797131, -4.999999999999997335 ) ) ;
#33182 = AXIS2_PLACEMENT_3D ( 'NONE', #13984, #25260, #25429 ) ;
#33183 = DIRECTION ( 'NONE',  ( 1.000000000000000000, 0.000000000000000000, 0.000000000000000000 ) ) ;
#33184 = ORIENTED_EDGE ( 'NONE', *, *, #20128, .F. ) ;
#33185 = ADVANCED_FACE ( 'NONE', ( #7179 ), #9975, .F. ) ;
#33186 = DIRECTION ( 'NONE',  ( 0.000000000000000000, 0.000000000000000000, 1.000000000000000000 ) ) ;
#33187 = ORIENTED_EDGE ( 'NONE', *, *, #5384, .T. ) ;
#33188 = DIRECTION ( 'NONE',  ( -1.000000000000000000, 0.000000000000000000, 0.000000000000000000 ) ) ;
#33189 = AXIS2_PLACEMENT_3D ( 'NONE', #24030, #12177, #9397 ) ;
#33190 = CARTESIAN_POINT ( 'NONE',  ( -82.00000337463094979, 17.32050807568878525, -9.999999999999998224 ) ) ;
#33191 = CIRCLE ( 'NONE', #17023, 3.500000000000003109 ) ;
#33192 = CARTESIAN_POINT ( 'NONE',  ( 0.1709976663248966577, 5.674777143212787145, -1.879366290983712107 ) ) ;
#33193 = ORIENTED_EDGE ( 'NONE', *, *, #3696, .F. ) ;
#33194 = ORIENTED_EDGE ( 'NONE', *, *, #20191, .F. ) ;
#33195 = DIRECTION ( 'NONE',  ( 1.000000000000000000, 0.000000000000000000, 0.000000000000000000 ) ) ;
#33196 = EDGE_CURVE ( 'NONE', #30803, #8170, #20728, .T. ) ;
#33197 = VERTEX_POINT ( 'NONE', #6782 ) ;
#33199 = CARTESIAN_POINT ( 'NONE',  ( -82.27241335952113843, 47.50000000000096634, 27.50000000000000000 ) ) ;
#33198 = CIRCLE ( 'NONE', #18324, 30.00000000000000000 ) ;
#33200 = CARTESIAN_POINT ( 'NONE',  ( 76.99999662536835388, -25.98076211353319565, -5.000000000000000000 ) ) ;
#33201 = AXIS2_PLACEMENT_3D ( 'NONE', #17993, #9163, #3369 ) ;
#33202 = DIRECTION ( 'NONE',  ( 0.000000000000000000, 0.000000000000000000, 1.000000000000000000 ) ) ;
#33203 = DIRECTION ( 'NONE',  ( -0.000000000000000000, -0.000000000000000000, 1.000000000000000000 ) ) ;
#33204 = CARTESIAN_POINT ( 'NONE',  ( -2.448772250512182280E-15, 99.94802294027086020, -19.99999999999999645 ) ) ;
#33205 = ORIENTED_EDGE ( 'NONE', *, *, #15246, .F. ) ;
#33206 = CARTESIAN_POINT ( 'NONE',  ( 44.13139720814400135, -27.50000000000022737, -15.00000000000000000 ) ) ;
#33207 = CIRCLE ( 'NONE', #14037, 2.000000000000001776 ) ;
#33208 = DIRECTION ( 'NONE',  ( 1.000000000000000000, 0.000000000000000000, 0.000000000000000000 ) ) ;
#33209 =( LENGTH_UNIT ( ) NAMED_UNIT ( * ) SI_UNIT ( .MILLI., .METRE. ) );
#33210 = ORIENTED_EDGE ( 'NONE', *, *, #36645, .T. ) ;
#33211 = DIRECTION ( 'NONE',  ( -1.000000000000000000, 0.000000000000000000, 0.000000000000000000 ) ) ;
#33212 = DIRECTION ( 'NONE',  ( 0.000000000000000000, 0.000000000000000000, -1.000000000000000000 ) ) ;
#33213 = AXIS2_PLACEMENT_3D ( 'NONE', #15722, #32585, #18725 ) ;
#33214 = ORIENTED_EDGE ( 'NONE', *, *, #12561, .F. ) ;
#33215 = AXIS2_PLACEMENT_3D ( 'NONE', #22691, #36747, #11046 ) ;
#33216 = AXIS2_PLACEMENT_3D ( 'NONE', #19820, #13822, #37071 ) ;
#33217 = EDGE_LOOP ( 'NONE', ( #7370, #7919, #31990, #28830 ) ) ;
#33218 = EDGE_CURVE ( 'NONE', #32300, #2420, #36942, .T. ) ;
#33219 = AXIS2_PLACEMENT_3D ( 'NONE', #5540, #17165, #5371 ) ;
#33220 = FACE_OUTER_BOUND ( 'NONE', #27604, .T. ) ;
#33221 = LINE ( 'NONE', #13174, #23570 ) ;
#33222 = EDGE_CURVE ( 'NONE', #10069, #34770, #2196, .T. ) ;
#33223 = CARTESIAN_POINT ( 'NONE',  ( -101.4252628994512833, -31.43180897937256191, 32.50001250000000397 ) ) ;
#33224 = ORIENTED_EDGE ( 'NONE', *, *, #30723, .T. ) ;
#33225 = EDGE_LOOP ( 'NONE', ( #32485, #25492 ) ) ;
#33226 = ORIENTED_EDGE ( 'NONE', *, *, #10352, .T. ) ;
#33227 = EDGE_CURVE ( 'NONE', #20954, #28688, #29649, .T. ) ;
#33228 = DIRECTION ( 'NONE',  ( 1.000000000000000000, 0.000000000000000000, 0.000000000000000000 ) ) ;
#33229 = CIRCLE ( 'NONE', #3280, 2.000000000000001776 ) ;
#33230 = ORIENTED_EDGE ( 'NONE', *, *, #9420, .T. ) ;
#33231 = CIRCLE ( 'NONE', #17642, 1.999999999999998224 ) ;
#33232 = EDGE_CURVE ( 'NONE', #14569, #24516, #27939, .T. ) ;
#33233 = CARTESIAN_POINT ( 'NONE',  ( 19.99999662536861678, -69.28203230275519786, 17.49999999999999645 ) ) ;
#33234 = ORIENTED_EDGE ( 'NONE', *, *, #9478, .F. ) ;
#33235 = EDGE_CURVE ( 'NONE', #23645, #36034, #21218, .T. ) ;
#33236 = EDGE_LOOP ( 'NONE', ( #3814, #29103 ) ) ;
#33237 = AXIS2_PLACEMENT_3D ( 'NONE', #24750, #27173, #22131 ) ;
#33238 = CARTESIAN_POINT ( 'NONE',  ( 0.000000000000000000, 0.000000000000000000, 12.49999999999999822 ) ) ;
#33239 = CARTESIAN_POINT ( 'NONE',  ( 0.000000000000000000, 0.000000000000000000, -5.000000000000000000 ) ) ;
#33240 = ORIENTED_EDGE ( 'NONE', *, *, #9994, .F. ) ;
#33241 = VERTEX_POINT ( 'NONE', #3980 ) ;
#33242 = DIRECTION ( 'NONE',  ( 1.000000000000000000, 0.000000000000000000, 0.000000000000000000 ) ) ;
#33243 = CYLINDRICAL_SURFACE ( 'NONE', #27935, 2.000000000000001776 ) ;
#33244 = ADVANCED_FACE ( 'NONE', ( #29855 ), #18791, .F. ) ;
#33245 = CIRCLE ( 'NONE', #16465, 2.000000000000001776 ) ;
#33246 = DIRECTION ( 'NONE',  ( 0.000000000000000000, 0.000000000000000000, 1.000000000000000000 ) ) ;
#33247 = EDGE_CURVE ( 'NONE', #16797, #5699, #11757, .T. ) ;
#33248 = CARTESIAN_POINT ( 'NONE',  ( -5.000003374631269537, -77.94228634059960825, 12.50000000000000000 ) ) ;
#33249 = EDGE_CURVE ( 'NONE', #22725, #5854, #12336, .T. ) ;
#33250 = EDGE_LOOP ( 'NONE', ( #28961, #2409 ) ) ;
#33251 = DIRECTION ( 'NONE',  ( 0.000000000000000000, 0.000000000000000000, 1.000000000000000000 ) ) ;
#33252 = ORIENTED_EDGE ( 'NONE', *, *, #15377, .F. ) ;
#33253 = CARTESIAN_POINT ( 'NONE',  ( -110.2237710830543733, -101.7384897088139724, 32.55002500000000509 ) ) ;
#33254 = ADVANCED_FACE ( 'NONE', ( #35868 ), #12769, .F. ) ;
#33255 = CARTESIAN_POINT ( 'NONE',  ( 24.99999662536859546, -77.94228634059960825, 17.49999999999999645 ) ) ;
#33256 = DIRECTION ( 'NONE',  ( 0.000000000000000000, 0.000000000000000000, 1.000000000000000000 ) ) ;
#33257 = DIRECTION ( 'NONE',  ( 1.000000000000000000, 0.000000000000000000, 0.000000000000000000 ) ) ;
#33258 = DIRECTION ( 'NONE',  ( -0.000000000000000000, -0.000000000000000000, 1.000000000000000000 ) ) ;
#33259 = DIRECTION ( 'NONE',  ( 1.000000000000000000, 0.000000000000000000, 0.000000000000000000 ) ) ;
#33260 = AXIS2_PLACEMENT_3D ( 'NONE', #28223, #22231, #36665 ) ;
#33261 = DIRECTION ( 'NONE',  ( -0.000000000000000000, -0.000000000000000000, -1.000000000000000000 ) ) ;
#33262 = ORIENTED_EDGE ( 'NONE', *, *, #4856, .F. ) ;
#33264 = AXIS2_PLACEMENT_3D ( 'NONE', #28550, #31192, #13931 ) ;
#33263 = CARTESIAN_POINT ( 'NONE',  ( -10.00000337463125000, -86.60254037844400443, 12.50000000000000000 ) ) ;
#33265 = DIRECTION ( 'NONE',  ( 1.000000000000000000, 0.000000000000000000, 0.000000000000000000 ) ) ;
#33266 = LINE ( 'NONE', #7584, #20526 ) ;
#33267 = AXIS2_PLACEMENT_3D ( 'NONE', #13535, #30978, #28169 ) ;
#33268 = AXIS2_PLACEMENT_3D ( 'NONE', #29760, #18539, #4097 ) ;
#33269 = ORIENTED_EDGE ( 'NONE', *, *, #11812, .F. ) ;
#33270 = AXIS2_PLACEMENT_3D ( 'NONE', #4456, #7274, #7091 ) ;
#33271 = VERTEX_POINT ( 'NONE', #9618 ) ;
#33272 = ADVANCED_FACE ( 'NONE', ( #10346 ), #24220, .F. ) ;
#33273 = ORIENTED_EDGE ( 'NONE', *, *, #215, .T. ) ;
#33274 = CIRCLE ( 'NONE', #26680, 33.00000000000001421 ) ;
#33275 = PLANE ( 'NONE',  #24329 ) ;
#33276 = DIRECTION ( 'NONE',  ( -1.000000000000000000, 0.000000000000000000, 0.000000000000000000 ) ) ;
#33277 = ORIENTED_EDGE ( 'NONE', *, *, #33421, .T. ) ;
#33278 = VECTOR ( 'NONE', #4065, 1000.000000000000000 ) ;
#33279 = CIRCLE ( 'NONE', #8731, 95.00000000000000000 ) ;
#33280 = CARTESIAN_POINT ( 'NONE',  ( -4.279621169095561228, 62.97617850287782915, 12.49999999999999822 ) ) ;
#33281 = DIRECTION ( 'NONE',  ( 0.000000000000000000, 0.000000000000000000, -1.000000000000000000 ) ) ;
#33282 = ORIENTED_EDGE ( 'NONE', *, *, #25228, .F. ) ;
#33283 = DIRECTION ( 'NONE',  ( -1.000000000000000000, 0.000000000000000000, 0.000000000000000000 ) ) ;
#33285 = EDGE_CURVE ( 'NONE', #5530, #25623, #13167, .T. ) ;
#33284 = VERTEX_POINT ( 'NONE', #1734 ) ;
#33286 = FACE_OUTER_BOUND ( 'NONE', #11157, .T. ) ;
#33287 = CARTESIAN_POINT ( 'NONE',  ( -40.00000337463113453, 69.28203230275516944, 12.50000000000000000 ) ) ;
#33288 = FACE_OUTER_BOUND ( 'NONE', #30235, .T. ) ;
#33289 = AXIS2_PLACEMENT_3D ( 'NONE', #14315, #17315, #5132 ) ;
#33290 = DIRECTION ( 'NONE',  ( 1.000000000000000000, 0.000000000000000000, 0.000000000000000000 ) ) ;
#33291 = CIRCLE ( 'NONE', #24924, 2.000000000000001776 ) ;
#33292 = ORIENTED_EDGE ( 'NONE', *, *, #2987, .T. ) ;
#33293 = CARTESIAN_POINT ( 'NONE',  ( -56.67878100130369035, 27.78182860042797131, -49.86348611802629449 ) ) ;
#33294 = CIRCLE ( 'NONE', #30873, 5.000000000000000888 ) ;
#33295 = AXIS2_PLACEMENT_3D ( 'NONE', #946, #9756, #758 ) ;
#33296 = AXIS2_PLACEMENT_3D ( 'NONE', #19581, #7951, #28366 ) ;
#33297 = LINE ( 'NONE', #2716, #27857 ) ;
#33298 = ADVANCED_FACE ( 'NONE', ( #4743 ), #22339, .F. ) ;
#33299 = DIRECTION ( 'NONE',  ( 0.000000000000000000, 0.000000000000000000, 1.000000000000000000 ) ) ;
#33300 = VECTOR ( 'NONE', #24731, 1000.000000000000000 ) ;
#33301 = ADVANCED_FACE ( 'NONE', ( #5295 ), #10529, .F. ) ;
#33302 = VERTEX_POINT ( 'NONE', #28321 ) ;
#33303 = CARTESIAN_POINT ( 'NONE',  ( 34.00000000000068923, 58.88972745734143643, -49.22241343995293761 ) ) ;
#33304 = CARTESIAN_POINT ( 'NONE',  ( 14.80603122773119118, -87.83969979969866415, 12.49999999999999645 ) ) ;
#33305 = EDGE_CURVE ( 'NONE', #36242, #29705, #30959, .T. ) ;
#33306 = ORIENTED_EDGE ( 'NONE', *, *, #15478, .F. ) ;
#33307 = DIRECTION ( 'NONE',  ( 1.000000000000000000, 0.000000000000000000, 0.000000000000000000 ) ) ;
#33308 = CIRCLE ( 'NONE', #4564, 2.000000000000001776 ) ;
#33309 = DIRECTION ( 'NONE',  ( 1.000000000000000000, 0.000000000000000000, 0.000000000000000000 ) ) ;
#33310 = DIRECTION ( 'NONE',  ( 3.469446951953612611E-15, 1.000000000000000000, 0.000000000000000000 ) ) ;
#33311 = VECTOR ( 'NONE', #21333, 1000.000000000000000 ) ;
#33312 = VERTEX_POINT ( 'NONE', #7733 ) ;
#33313 = EDGE_LOOP ( 'NONE', ( #4728, #33778 ) ) ;
#33314 = LINE ( 'NONE', #32950, #18361 ) ;
#33315 = DIRECTION ( 'NONE',  ( -0.000000000000000000, -0.000000000000000000, -1.000000000000000000 ) ) ;
#33316 = CIRCLE ( 'NONE', #6944, 2.000000000000001776 ) ;
#33317 = CARTESIAN_POINT ( 'NONE',  ( 68.19434990244977257, -52.39915983220758022, -49.22241343995298024 ) ) ;
#33318 = ORIENTED_EDGE ( 'NONE', *, *, #2648, .T. ) ;
#33319 = VERTEX_POINT ( 'NONE', #16899 ) ;
#33320 = AXIS2_PLACEMENT_3D ( 'NONE', #24975, #22329, #17067 ) ;
#33321 = FACE_OUTER_BOUND ( 'NONE', #20670, .T. ) ;
#33322 = LINE ( 'NONE', #16267, #14224 ) ;
#33323 = STYLED_ITEM ( 'NONE', ( #10109 ), #30477 ) ;
#33324 = DIRECTION ( 'NONE',  ( 0.000000000000000000, 0.000000000000000000, 1.000000000000000000 ) ) ;
#33325 = CIRCLE ( 'NONE', #17159, 2.000000000000001776 ) ;
#33326 = AXIS2_PLACEMENT_3D ( 'NONE', #19369, #8321, #13751 ) ;
#33327 = CARTESIAN_POINT ( 'NONE',  ( -107.2742589609544410, 47.50000425637879431, 32.50001250000000397 ) ) ;
#33328 = CIRCLE ( 'NONE', #16548, 2.000000000000001776 ) ;
#33329 = EDGE_CURVE ( 'NONE', #27967, #14230, #13722, .T. ) ;
#33330 = ORIENTED_EDGE ( 'NONE', *, *, #3960, .T. ) ;
#33331 = CIRCLE ( 'NONE', #23150, 33.00000000000001421 ) ;
#33332 = VERTEX_POINT ( 'NONE', #16350 ) ;
#33333 = CARTESIAN_POINT ( 'NONE',  ( -5.000003374631269537, -77.94228634059960825, -9.999999999999998224 ) ) ;
#33334 = CIRCLE ( 'NONE', #11185, 2.000000000000001776 ) ;
#33335 = LINE ( 'NONE', #13992, #21269 ) ;
#33336 = VERTEX_POINT ( 'NONE', #13521 ) ;
#33337 = CARTESIAN_POINT ( 'NONE',  ( -3.401922400365994026, -3.809401878283186882, -3.971474537230573532 ) ) ;
#33338 = VERTEX_POINT ( 'NONE', #33418 ) ;
#33339 = CARTESIAN_POINT ( 'NONE',  ( 5.750000000000000000, 89.94802294027094547, 32.49999999999999289 ) ) ;
#33340 = AXIS2_PLACEMENT_3D ( 'NONE', #17686, #15242, #1001 ) ;
#33341 = CARTESIAN_POINT ( 'NONE',  ( -3.351853367131006234, 3.838309248099018411, -6.000000000000003553 ) ) ;
#33342 = VERTEX_POINT ( 'NONE', #19346 ) ;
#33343 = CARTESIAN_POINT ( 'NONE',  ( 0.8441225671308623113, 5.568793373801118385, -4.176900509771833470 ) ) ;
#33344 = ORIENTED_EDGE ( 'NONE', *, *, #22291, .T. ) ;
#33345 =( LENGTH_UNIT ( ) NAMED_UNIT ( * ) SI_UNIT ( .MILLI., .METRE. ) );
#33346 = VECTOR ( 'NONE', #14484, 1000.000000000000000 ) ;
#33347 = LINE ( 'NONE', #4673, #18219 ) ;
#33348 = CIRCLE ( 'NONE', #16593, 2.000000000000001776 ) ;
#33349 = DIRECTION ( 'NONE',  ( -0.000000000000000000, -0.000000000000000000, 1.000000000000000000 ) ) ;
#33350 = CARTESIAN_POINT ( 'NONE',  ( -8.000003374631287301, 69.28203230275516944, -9.999999999999998224 ) ) ;
#33351 = EDGE_CURVE ( 'NONE', #21860, #36148, #9979, .T. ) ;
#33352 = ORIENTED_EDGE ( 'NONE', *, *, #2258, .F. ) ;
#33353 = DIRECTION ( 'NONE',  ( -1.000000000000000000, 0.000000000000000000, 0.000000000000000000 ) ) ;
#33354 = FACE_OUTER_BOUND ( 'NONE', #31121, .T. ) ;
#33355 = LINE ( 'NONE', #12184, #14814 ) ;
#33356 = DIRECTION ( 'NONE',  ( -0.000000000000000000, -0.000000000000000000, 1.000000000000000000 ) ) ;
#33357 = EDGE_LOOP ( 'NONE', ( #33193, #19908, #13216, #30540 ) ) ;
#33358 = AXIS2_PLACEMENT_3D ( 'NONE', #4807, #24115, #1415 ) ;
#33359 = ORIENTED_EDGE ( 'NONE', *, *, #35360, .T. ) ;
#33360 = VECTOR ( 'NONE', #11164, 1000.000000000000000 ) ;
#33361 = ORIENTED_EDGE ( 'NONE', *, *, #4596, .F. ) ;
#33362 = DIRECTION ( 'NONE',  ( 1.000000000000000000, 0.000000000000000000, 0.000000000000000000 ) ) ;
#33363 = ORIENTED_EDGE ( 'NONE', *, *, #8399, .T. ) ;
#33364 = DIRECTION ( 'NONE',  ( 0.000000000000000000, 0.000000000000000000, 1.000000000000000000 ) ) ;
#33365 = FACE_OUTER_BOUND ( 'NONE', #25941, .T. ) ;
#33366 = AXIS2_PLACEMENT_3D ( 'NONE', #19552, #33998, #10911 ) ;
#33367 = DIRECTION ( 'NONE',  ( -1.000000000000000000, 0.000000000000000000, 0.000000000000000000 ) ) ;
#33368 = CYLINDRICAL_SURFACE ( 'NONE', #9229, 2.000000000000001776 ) ;
#33369 = DIRECTION ( 'NONE',  ( 0.000000000000000000, 0.000000000000000000, 1.000000000000000000 ) ) ;
#33370 = CARTESIAN_POINT ( 'NONE',  ( -104.5390599191612182, -58.87763622169656941, 32.50000000000000000 ) ) ;
#33371 = CARTESIAN_POINT ( 'NONE',  ( -1.074820392479180450E-14, 5.987020429981924075, -4.330720594357048370 ) ) ;
#33372 = VECTOR ( 'NONE', #4777, 1000.000000000000114 ) ;
#33373 = ADVANCED_FACE ( 'NONE', ( #24983 ), #2475, .F. ) ;
#33374 = DIRECTION ( 'NONE',  ( 1.000000000000000000, 0.000000000000000000, 0.000000000000000000 ) ) ;
#33375 = VERTEX_POINT ( 'NONE', #36421 ) ;
#33376 = CIRCLE ( 'NONE', #17207, 2.000000000000001776 ) ;
#33377 = ORIENTED_EDGE ( 'NONE', *, *, #13517, .T. ) ;
#33378 = SURFACE_STYLE_USAGE ( .BOTH. , #7881 ) ;
#33379 = DIRECTION ( 'NONE',  ( 0.000000000000000000, 0.000000000000000000, -1.000000000000000000 ) ) ;
#33380 = CARTESIAN_POINT ( 'NONE',  ( -80.00000337463094979, -2.428612866367529932E-14, -9.999999999999998224 ) ) ;
#33381 = DIRECTION ( 'NONE',  ( 0.000000000000000000, 0.000000000000000000, 1.000000000000000000 ) ) ;
#33382 = ORIENTED_EDGE ( 'NONE', *, *, #35810, .T. ) ;
#33383 = CIRCLE ( 'NONE', #2222, 2.000000000000001776 ) ;
#33384 = CIRCLE ( 'NONE', #1660, 30.00000000000000000 ) ;
#33385 = DIRECTION ( 'NONE',  ( 1.000000000000000000, 0.000000000000000000, 0.000000000000000000 ) ) ;
#33386 = AXIS2_PLACEMENT_3D ( 'NONE', #11145, #17347, #22594 ) ;
#33387 = ADVANCED_FACE ( 'NONE', ( #2642 ), #9357, .T. ) ;
#33388 = CARTESIAN_POINT ( 'NONE',  ( 5.000000000000000000, -1.472375319565264684, -0.9369361380397587258 ) ) ;
#33389 = ORIENTED_EDGE ( 'NONE', *, *, #19467, .F. ) ;
#33390 = CARTESIAN_POINT ( 'NONE',  ( 3.000000000000000000, -1.467624384280027172, 2.542000000000001592 ) ) ;
#33391 = VERTEX_POINT ( 'NONE', #5091 ) ;
#33392 = CIRCLE ( 'NONE', #23194, 65.00000000000000000 ) ;
#33393 = FILL_AREA_STYLE_COLOUR ( '', #6353 ) ;
#33394 = CARTESIAN_POINT ( 'NONE',  ( 81.86307328356784296, -18.04779437809804321, 12.50000000000000000 ) ) ;
#33395 = DIRECTION ( 'NONE',  ( -0.000000000000000000, -0.000000000000000000, 1.000000000000000000 ) ) ;
#33396 = CARTESIAN_POINT ( 'NONE',  ( 0.3000000000000016542, 0.000000000000000000, 0.000000000000000000 ) ) ;
#33397 = ADVANCED_FACE ( 'NONE', ( #36970 ), #19722, .F. ) ;
#33398 = ORIENTED_EDGE ( 'NONE', *, *, #2572, .T. ) ;
#33399 = ORIENTED_EDGE ( 'NONE', *, *, #23802, .F. ) ;
#33400 = AXIS2_PLACEMENT_3D ( 'NONE', #9282, #5745, #3292 ) ;
#33401 = AXIS2_PLACEMENT_3D ( 'NONE', #34197, #6050, #20461 ) ;
#33402 = AXIS2_PLACEMENT_3D ( 'NONE', #33417, #4742, #24789 ) ;
#33403 = ORIENTED_EDGE ( 'NONE', *, *, #23113, .T. ) ;
#33404 = CARTESIAN_POINT ( 'NONE',  ( -67.00000337463102085, 43.30127018922198801, 12.50000000000000000 ) ) ;
#33405 = DIRECTION ( 'NONE',  ( 0.000000000000000000, 0.000000000000000000, 1.000000000000000000 ) ) ;
#33406 = CARTESIAN_POINT ( 'NONE',  ( -45.00000337463112743, -60.62177826491080168, -5.000000000000000000 ) ) ;
#33407 = CARTESIAN_POINT ( 'NONE',  ( -42.00000337463114164, -69.28203230275519786, -5.000000000000000000 ) ) ;
#33408 = DIRECTION ( 'NONE',  ( 0.000000000000000000, 0.000000000000000000, 1.000000000000000000 ) ) ;
#33409 = ORIENTED_EDGE ( 'NONE', *, *, #36476, .T. ) ;
#33410 = CYLINDRICAL_SURFACE ( 'NONE', #17704, 2.000000000000001776 ) ;
#33411 = ADVANCED_FACE ( 'NONE', ( #25524 ), #13895, .T. ) ;
#33412 = CIRCLE ( 'NONE', #13652, 5.750000000000002665 ) ;
#33413 = CARTESIAN_POINT ( 'NONE',  ( 67.99999662536838230, 17.32050807568879236, 12.50000000000000000 ) ) ;
#33414 = EDGE_CURVE ( 'NONE', #5018, #33284, #14153, .T. ) ;
#33415 = CARTESIAN_POINT ( 'NONE',  ( -15.00000337463126066, 77.94228634059957983, -9.999999999999998224 ) ) ;
#33416 = ORIENTED_EDGE ( 'NONE', *, *, #13799, .T. ) ;
#33417 = CARTESIAN_POINT ( 'NONE',  ( 44.99999662536849598, 60.62177826491077326, 12.50000000000000000 ) ) ;
#33418 = CARTESIAN_POINT ( 'NONE',  ( -33.00000337463116296, -60.62177826491080168, -9.999999999999998224 ) ) ;
#33419 = AXIS2_PLACEMENT_3D ( 'NONE', #36080, #1213, #10377 ) ;
#33420 = ORIENTED_EDGE ( 'NONE', *, *, #34396, .T. ) ;
#33421 = EDGE_CURVE ( 'NONE', #10270, #30265, #12970, .T. ) ;
#33422 = ORIENTED_EDGE ( 'NONE', *, *, #36750, .F. ) ;
#33423 = AXIS2_PLACEMENT_3D ( 'NONE', #4521, #9956, #1330 ) ;
#33424 = FACE_OUTER_BOUND ( 'NONE', #2897, .T. ) ;
#33425 = CARTESIAN_POINT ( 'NONE',  ( 37.50000000000000000, -103.4105893997321743, 32.50000000000000000 ) ) ;
#33426 = CARTESIAN_POINT ( 'NONE',  ( 149.8799519615616020, -6.000000000000508038, 27.50000000000000000 ) ) ;
#33427 = EDGE_CURVE ( 'NONE', #40, #7276, #27963, .T. ) ;
#33428 = ORIENTED_EDGE ( 'NONE', *, *, #23763, .F. ) ;
#33429 = ORIENTED_EDGE ( 'NONE', *, *, #32637, .F. ) ;
#33430 = AXIS2_PLACEMENT_3D ( 'NONE', #1957, #2522, #33276 ) ;
#33431 = CIRCLE ( 'NONE', #14259, 2.000000000000001776 ) ;
#33432 = VERTEX_POINT ( 'NONE', #5472 ) ;
#33433 = CIRCLE ( 'NONE', #34640, 2.000000000000001776 ) ;
#33434 = CARTESIAN_POINT ( 'NONE',  ( -35.00000337463116296, 77.94228634059957983, -5.000000000000000000 ) ) ;
#33435 = EDGE_CURVE ( 'NONE', #13680, #3339, #35744, .T. ) ;
#33436 = VECTOR ( 'NONE', #3931, 1000.000000000000000 ) ;
#33437 = ORIENTED_EDGE ( 'NONE', *, *, #34206, .T. ) ;
#33438 = CARTESIAN_POINT ( 'NONE',  ( -45.00000337463111322, 77.94228634059959404, -9.999999999999998224 ) ) ;
#33439 = ORIENTED_EDGE ( 'NONE', *, *, #34909, .F. ) ;
#33440 = ORIENTED_EDGE ( 'NONE', *, *, #4592, .F. ) ;
#33441 = VECTOR ( 'NONE', #30621, 1000.000000000000000 ) ;
#33442 = DIRECTION ( 'NONE',  ( 0.000000000000000000, 0.000000000000000000, 1.000000000000000000 ) ) ;
#33443 = LINE ( 'NONE', #1754, #17079 ) ;
#33444 = ORIENTED_EDGE ( 'NONE', *, *, #23414, .F. ) ;
#33445 = VERTEX_POINT ( 'NONE', #27602 ) ;
#33446 = CARTESIAN_POINT ( 'NONE',  ( 95.00000000000000000, 1.163414459189985643E-14, 12.49999999999999822 ) ) ;
#33447 = AXIS2_PLACEMENT_3D ( 'NONE', #31088, #5771, #5417 ) ;
#33448 = CARTESIAN_POINT ( 'NONE',  ( 45.00000000000000000, 5.510910596163089556E-15, 15.00000000000000000 ) ) ;
#33449 = DIRECTION ( 'NONE',  ( -0.000000000000000000, -0.000000000000000000, 1.000000000000000000 ) ) ;
#33450 = DIRECTION ( 'NONE',  ( 1.000000000000000000, 0.000000000000000000, 0.000000000000000000 ) ) ;
#33451 = EDGE_CURVE ( 'NONE', #5475, #21277, #24361, .T. ) ;
#33452 = EDGE_LOOP ( 'NONE', ( #19095, #3634 ) ) ;
#33453 = CARTESIAN_POINT ( 'NONE',  ( -65.00000337463104927, -25.98076211353322051, -9.999999999999998224 ) ) ;
#33454 = AXIS2_PLACEMENT_3D ( 'NONE', #19158, #16333, #22319 ) ;
#33455 = FACE_BOUND ( 'NONE', #31552, .T. ) ;
#33456 = CIRCLE ( 'NONE', #26834, 1.999999999999998224 ) ;
#33457 = CARTESIAN_POINT ( 'NONE',  ( 79.99999662536833966, -3.469446951953614189E-15, -9.999999999999998224 ) ) ;
#33458 = DIRECTION ( 'NONE',  ( 0.000000000000000000, 0.000000000000000000, -1.000000000000000000 ) ) ;
#33459 = DIRECTION ( 'NONE',  ( 1.000000000000000000, 0.000000000000000000, 0.000000000000000000 ) ) ;
#33461 = AXIS2_PLACEMENT_3D ( 'NONE', #655, #15088, #2932 ) ;
#33460 = DIRECTION ( 'NONE',  ( 1.000000000000000000, 0.000000000000000000, 0.000000000000000000 ) ) ;
#33462 = EDGE_CURVE ( 'NONE', #10417, #35979, #17761, .T. ) ;
#33463 = CARTESIAN_POINT ( 'NONE',  ( -16.42335909229131374, 114.0197456316801237, 27.49998799999999477 ) ) ;
#33464 = CIRCLE ( 'NONE', #17872, 2.000000000000001776 ) ;
#33465 = ADVANCED_FACE ( 'NONE', ( #17448 ), #6027, .F. ) ;
#33466 = CARTESIAN_POINT ( 'NONE',  ( 33.21453428580180400, -78.84346569788027637, 12.50000000000000000 ) ) ;
#33467 = ORIENTED_EDGE ( 'NONE', *, *, #29664, .T. ) ;
#33468 = CARTESIAN_POINT ( 'NONE',  ( 69.99999662536839651, 34.64101615137758472, -9.999999999999998224 ) ) ;
#33469 = ADVANCED_FACE ( 'NONE', ( #14453 ), #23624, .F. ) ;
#33470 = FACE_OUTER_BOUND ( 'NONE', #18674, .T. ) ;
#33471 = CARTESIAN_POINT ( 'NONE',  ( 67.99999662536838230, -3.224517592124143893E-15, -9.999999999999998224 ) ) ;
#33472 = VECTOR ( 'NONE', #11455, 1000.000000000000000 ) ;
#33473 = ORIENTED_EDGE ( 'NONE', *, *, #347, .F. ) ;
#33474 = SHAPE_REPRESENTATION ( 'rotor hub', ( #21385 ), #22589 ) ;
#33475 = VECTOR ( 'NONE', #18251, 1000.000000000000000 ) ;
#33476 = EDGE_LOOP ( 'NONE', ( #3306, #37052 ) ) ;
#33477 = ORIENTED_EDGE ( 'NONE', *, *, #32957, .T. ) ;
#33478 = FACE_OUTER_BOUND ( 'NONE', #24606, .T. ) ;
#33479 = DIRECTION ( 'NONE',  ( 0.000000000000000000, 0.000000000000000000, 1.000000000000000000 ) ) ;
#33480 = VERTEX_POINT ( 'NONE', #32246 ) ;
#33481 = PRODUCT_DEFINITION_SHAPE ( 'NONE', 'NONE',  #37110 ) ;
#33482 = CARTESIAN_POINT ( 'NONE',  ( -15.00000337463125710, -77.94228634059960825, -5.000000000000000000 ) ) ;
#33483 = ADVANCED_FACE ( 'NONE', ( #29251 ), #5838, .F. ) ;
#33484 = CIRCLE ( 'NONE', #16112, 33.00000000000001421 ) ;
#33485 = CARTESIAN_POINT ( 'NONE',  ( -78.00000337463094979, 17.32050807568878525, -9.999999999999998224 ) ) ;
#33486 = ORIENTED_EDGE ( 'NONE', *, *, #9337, .F. ) ;
#33487 = FACE_OUTER_BOUND ( 'NONE', #2797, .T. ) ;
#33488 = ORIENTED_EDGE ( 'NONE', *, *, #25374, .F. ) ;
#33489 = AXIS2_PLACEMENT_3D ( 'NONE', #818, #18070, #15252 ) ;
#33490 = FACE_BOUND ( 'NONE', #19000, .T. ) ;
#33491 = CYLINDRICAL_SURFACE ( 'NONE', #12394, 2.000000000000001776 ) ;
#33492 = CYLINDRICAL_SURFACE ( 'NONE', #21526, 2.000000000000000000 ) ;
#33493 = AXIS2_PLACEMENT_3D ( 'NONE', #22038, #36100, #10400 ) ;
#33494 = CARTESIAN_POINT ( 'NONE',  ( 7.999996625368625658, 86.60254037844397601, -9.999999999999998224 ) ) ;
#33495 = ORIENTED_EDGE ( 'NONE', *, *, #34866, .F. ) ;
#33496 = CARTESIAN_POINT ( 'NONE',  ( -34.00000000000000000, -103.4105893997321743, 32.50000000000000000 ) ) ;
#33497 = CONTEXT_DEPENDENT_SHAPE_REPRESENTATION ( #30518, #24157 ) ;
#33498 = CIRCLE ( 'NONE', #22118, 8.500000000000000000 ) ;
#33499 = LINE ( 'NONE', #16416, #34461 ) ;
#33500 = DIRECTION ( 'NONE',  ( 1.000000000000000000, 1.422473250300981817E-14, 0.000000000000000000 ) ) ;
#33501 = AXIS2_PLACEMENT_3D ( 'NONE', #13646, #36537, #19110 ) ;
#33502 = ADVANCED_FACE ( 'NONE', ( #32035 ), #31497, .F. ) ;
#33503 = ORIENTED_EDGE ( 'NONE', *, *, #28832, .F. ) ;
#33504 = DIRECTION ( 'NONE',  ( 0.000000000000000000, 0.000000000000000000, 1.000000000000000000 ) ) ;
#33505 = DIRECTION ( 'NONE',  ( 0.000000000000000000, 0.000000000000000000, 1.000000000000000000 ) ) ;
#33506 = VERTEX_POINT ( 'NONE', #184 ) ;
#33507 = EDGE_CURVE ( 'NONE', #8634, #598, #8825, .T. ) ;
#33508 = CARTESIAN_POINT ( 'NONE',  ( -80.00000337463094979, 17.32050807568878525, 17.49999999999999645 ) ) ;
#33509 = DIRECTION ( 'NONE',  ( 1.000000000000000000, 0.000000000000000000, 0.000000000000000000 ) ) ;
#33510 = DIRECTION ( 'NONE',  ( 0.000000000000000000, 0.000000000000000000, -1.000000000000000000 ) ) ;
#33511 = ADVANCED_FACE ( 'NONE', ( #12159 ), #6375, .F. ) ;
#33512 = VECTOR ( 'NONE', #35646, 1000.000000000000000 ) ;
#33513 = ORIENTED_EDGE ( 'NONE', *, *, #7559, .F. ) ;
#33514 = CIRCLE ( 'NONE', #11361, 2.000000000000001776 ) ;
#33515 = ORIENTED_EDGE ( 'NONE', *, *, #23625, .T. ) ;
#33516 = EDGE_CURVE ( 'NONE', #15574, #31133, #27966, .T. ) ;
#33517 = CIRCLE ( 'NONE', #15518, 3.500000000000003109 ) ;
#33518 = LINE ( 'NONE', #4993, #1602 ) ;
#33519 = DIRECTION ( 'NONE',  ( -1.000000000000000000, 0.000000000000000000, 0.000000000000000000 ) ) ;
#33520 = EDGE_CURVE ( 'NONE', #13843, #26293, #31693, .T. ) ;
#33521 = DIRECTION ( 'NONE',  ( -1.000000000000000000, 0.000000000000000000, 0.000000000000000000 ) ) ;
#33522 = ORIENTED_EDGE ( 'NONE', *, *, #17202, .T. ) ;
#33523 = ORIENTED_EDGE ( 'NONE', *, *, #3048, .F. ) ;
#33524 = DIRECTION ( 'NONE',  ( -0.000000000000000000, -0.000000000000000000, 1.000000000000000000 ) ) ;
#33525 = DIRECTION ( 'NONE',  ( 0.000000000000000000, 0.000000000000000000, 1.000000000000000000 ) ) ;
#33526 = CARTESIAN_POINT ( 'NONE',  ( 67.99999662536838230, -3.224517592124143893E-15, -5.000000000000000000 ) ) ;
#33528 = CARTESIAN_POINT ( 'NONE',  ( -87.00000337463093558, -8.660254037844422825, -9.999999999999998224 ) ) ;
#33527 = CIRCLE ( 'NONE', #1181, 2.000000000000001776 ) ;
#33529 = EDGE_CURVE ( 'NONE', #35441, #28925, #2223, .T. ) ;
#33530 = VERTEX_POINT ( 'NONE', #17279 ) ;
#33532 = ORIENTED_EDGE ( 'NONE', *, *, #18390, .T. ) ;
#33531 = ADVANCED_FACE ( 'NONE', ( #31854 ), #11807, .F. ) ;
#33533 = DIRECTION ( 'NONE',  ( 1.000000000000000000, 0.000000000000000000, 0.000000000000000000 ) ) ;
#33534 = CIRCLE ( 'NONE', #25155, 2.000000000000001776 ) ;
#33535 = ADVANCED_FACE ( 'NONE', ( #6187 ), #747, .F. ) ;
#33536 = CARTESIAN_POINT ( 'NONE',  ( 19.99999662536857770, 86.60254037844397601, -9.999999999999998224 ) ) ;
#33538 = EDGE_CURVE ( 'NONE', #8984, #30547, #23266, .T. ) ;
#33537 = EDGE_LOOP ( 'NONE', ( #7537, #28030 ) ) ;
#33539 = DIRECTION ( 'NONE',  ( 0.000000000000000000, 0.000000000000000000, 1.000000000000000000 ) ) ;
#33540 = EDGE_LOOP ( 'NONE', ( #5608, #7118, #6577, #28643 ) ) ;
#33542 = CIRCLE ( 'NONE', #28137, 2.000000000000001776 ) ;
#33541 = CYLINDRICAL_SURFACE ( 'NONE', #15336, 2.000000000000001776 ) ;
#33543 = CARTESIAN_POINT ( 'NONE',  ( 14.99999662536859901, 77.94228634059957983, -5.000000000000000000 ) ) ;
#33544 = CIRCLE ( 'NONE', #10782, 2.000000000000001776 ) ;
#33545 = AXIS2_PLACEMENT_3D ( 'NONE', #20545, #18305, #26198 ) ;
#33546 = DIRECTION ( 'NONE',  ( 0.000000000000000000, 0.000000000000000000, 1.000000000000000000 ) ) ;
#33547 = ORIENTED_EDGE ( 'NONE', *, *, #2470, .F. ) ;
#33548 =( NAMED_UNIT ( * ) SI_UNIT ( $, .STERADIAN. ) SOLID_ANGLE_UNIT ( ) );
#33549 = CARTESIAN_POINT ( 'NONE',  ( 56.67878100130369035, -27.78182860042797131, -4.999999999999997335 ) ) ;
#33550 = DIRECTION ( 'NONE',  ( -1.000000000000000000, 0.000000000000000000, 0.000000000000000000 ) ) ;
#33551 = CARTESIAN_POINT ( 'NONE',  ( 35.44550000000001688, 0.000000000000000000, 0.000000000000000000 ) ) ;
#33552 = ORIENTED_EDGE ( 'NONE', *, *, #932, .T. ) ;
#33553 = CARTESIAN_POINT ( 'NONE',  ( 74.99999662536835388, -25.98076211353319565, 12.50000000000000000 ) ) ;
#33554 = DIRECTION ( 'NONE',  ( 0.000000000000000000, 0.000000000000000000, 1.000000000000000000 ) ) ;
#33555 = CARTESIAN_POINT ( 'NONE',  ( 47.63139720814418610, 27.49999999999988987, 5.000000000000000888 ) ) ;
#33556 = AXIS2_PLACEMENT_3D ( 'NONE', #24494, #16049, #21487 ) ;
#33557 = ORIENTED_EDGE ( 'NONE', *, *, #13552, .F. ) ;
#33558 = ORIENTED_EDGE ( 'NONE', *, *, #2444, .F. ) ;
#33559 = STYLED_ITEM ( 'NONE', ( #18040 ), #7743 ) ;
#33560 = CYLINDRICAL_SURFACE ( 'NONE', #3623, 3.000000000000002665 ) ;
#33561 = ORIENTED_EDGE ( 'NONE', *, *, #29115, .T. ) ;
#33562 = CARTESIAN_POINT ( 'NONE',  ( -15.00000337463126066, 77.94228634059957983, -5.000000000000000000 ) ) ;
#33563 = CIRCLE ( 'NONE', #23384, 2.000000000000001776 ) ;
#33564 = CYLINDRICAL_SURFACE ( 'NONE', #12385, 2.000000000000000000 ) ;
#33565 = FACE_OUTER_BOUND ( 'NONE', #23209, .T. ) ;
#33566 = AXIS2_PLACEMENT_3D ( 'NONE', #9707, #32568, #7643 ) ;
#33567 = CARTESIAN_POINT ( 'NONE',  ( 21.99999662536862033, -86.60254037844400443, 12.50000000000000000 ) ) ;
#33568 = DIRECTION ( 'NONE',  ( 0.000000000000000000, 0.000000000000000000, 1.000000000000000000 ) ) ;
#33569 = DIRECTION ( 'NONE',  ( 1.000000000000000000, 0.000000000000000000, 0.000000000000000000 ) ) ;
#33570 = DIRECTION ( 'NONE',  ( 1.000000000000000000, 0.000000000000000000, 0.000000000000000000 ) ) ;
#33571 = FACE_OUTER_BOUND ( 'NONE', #27369, .T. ) ;
#33572 = ORIENTED_EDGE ( 'NONE', *, *, #12081, .T. ) ;
#33573 = ORIENTED_EDGE ( 'NONE', *, *, #11291, .T. ) ;
#33574 = DIRECTION ( 'NONE',  ( 0.000000000000000000, 0.000000000000000000, 1.000000000000000000 ) ) ;
#33575 = CARTESIAN_POINT ( 'NONE',  ( 36.99999662536855283, 60.62177826491078747, 12.50000000000000000 ) ) ;
#33576 = EDGE_CURVE ( 'NONE', #755, #36148, #8633, .T. ) ;
#33577 = LINE ( 'NONE', #30370, #17436 ) ;
#33578 = CIRCLE ( 'NONE', #11396, 27.00000000000001421 ) ;
#33579 = CARTESIAN_POINT ( 'NONE',  ( -67.00000337463106348, -60.62177826491083010, -9.999999999999998224 ) ) ;
#33580 = ORIENTED_EDGE ( 'NONE', *, *, #9585, .T. ) ;
#33581 = DIRECTION ( 'NONE',  ( 0.000000000000000000, 0.000000000000000000, 1.000000000000000000 ) ) ;
#33582 = CYLINDRICAL_SURFACE ( 'NONE', #13791, 27.00000000000001066 ) ;
#33583 = ORIENTED_EDGE ( 'NONE', *, *, #25679, .F. ) ;
#33584 = VECTOR ( 'NONE', #28151, 1000.000000000000000 ) ;
#33585 = DIRECTION ( 'NONE',  ( 0.000000000000000000, 0.000000000000000000, 1.000000000000000000 ) ) ;
#33586 = EDGE_LOOP ( 'NONE', ( #35477, #2739 ) ) ;
#33587 = SURFACE_STYLE_USAGE ( .BOTH. , #33013 ) ;
#33588 = CARTESIAN_POINT ( 'NONE',  ( 32.99999662536855283, -60.62177826491080168, -9.999999999999998224 ) ) ;
#33589 = DIRECTION ( 'NONE',  ( 0.000000000000000000, 0.000000000000000000, -1.000000000000000000 ) ) ;
#33590 = DIRECTION ( 'NONE',  ( 0.8660254037844347108, -0.5000000000000067724, 0.000000000000000000 ) ) ;
#33591 = ORIENTED_EDGE ( 'NONE', *, *, #34659, .T. ) ;
#33592 = ORIENTED_EDGE ( 'NONE', *, *, #19474, .F. ) ;
#33593 = EDGE_CURVE ( 'NONE', #24047, #20316, #11613, .T. ) ;
#33594 = EDGE_CURVE ( 'NONE', #7804, #30855, #11993, .T. ) ;
#33595 = VERTEX_POINT ( 'NONE', #24181 ) ;
#33596 = DIRECTION ( 'NONE',  ( 1.000000000000000000, 0.000000000000000000, 0.000000000000000000 ) ) ;
#33597 = CARTESIAN_POINT ( 'NONE',  ( -37.00000337463117717, -77.94228634059963667, -5.000000000000000000 ) ) ;
#33598 = DIRECTION ( 'NONE',  ( 0.000000000000000000, 0.000000000000000000, 1.000000000000000000 ) ) ;
#33599 = FACE_OUTER_BOUND ( 'NONE', #24546, .T. ) ;
#33600 = DIRECTION ( 'NONE',  ( -0.000000000000000000, -0.000000000000000000, 1.000000000000000000 ) ) ;
#33601 = VERTEX_POINT ( 'NONE', #35278 ) ;
#33602 = DIRECTION ( 'NONE',  ( 1.000000000000000000, 0.000000000000000000, 0.000000000000000000 ) ) ;
#33603 = DIRECTION ( 'NONE',  ( -1.000000000000000000, 0.000000000000000000, 0.000000000000000000 ) ) ;
#33604 = ADVANCED_FACE ( 'NONE', ( #27168 ), #24378, .F. ) ;
#33605 = CIRCLE ( 'NONE', #21009, 2.000000000000001776 ) ;
#33606 = DIRECTION ( 'NONE',  ( 1.000000000000000000, 0.000000000000000000, 0.000000000000000000 ) ) ;
#33607 = ORIENTED_EDGE ( 'NONE', *, *, #13537, .F. ) ;
#33608 = FACE_OUTER_BOUND ( 'NONE', #16122, .T. ) ;
#33609 = CARTESIAN_POINT ( 'NONE',  ( -15.97563234535668109, 90.60231327712331506, 12.49999999999999822 ) ) ;
#33610 = VERTEX_POINT ( 'NONE', #35828 ) ;
#33611 = ORIENTED_EDGE ( 'NONE', *, *, #9099, .F. ) ;
#33612 = FACE_OUTER_BOUND ( 'NONE', #18059, .T. ) ;
#33613 = CARTESIAN_POINT ( 'NONE',  ( 27.99999662536855993, 69.28203230275518365, -9.999999999999998224 ) ) ;
#33614 = EDGE_CURVE ( 'NONE', #8438, #30579, #17788, .T. ) ;
#33615 = CARTESIAN_POINT ( 'NONE',  ( 1.721886139903932023, -5.052888355616823368, -4.057689166958430960 ) ) ;
#33616 = FACE_OUTER_BOUND ( 'NONE', #36285, .T. ) ;
#33617 = ORIENTED_EDGE ( 'NONE', *, *, #37060, .T. ) ;
#33618 = ORIENTED_EDGE ( 'NONE', *, *, #25633, .T. ) ;
#33619 = DIRECTION ( 'NONE',  ( 0.000000000000000000, 0.000000000000000000, 1.000000000000000000 ) ) ;
#33620 = ORIENTED_EDGE ( 'NONE', *, *, #28920, .F. ) ;
#33621 = AXIS2_PLACEMENT_3D ( 'NONE', #11998, #26444, #32618 ) ;
#33622 = CARTESIAN_POINT ( 'NONE',  ( 32.99999662536855283, -77.94228634059960825, 17.49999999999999645 ) ) ;
#33623 = ORIENTED_EDGE ( 'NONE', *, *, #16271, .T. ) ;
#33624 = ORIENTED_EDGE ( 'NONE', *, *, #34537, .T. ) ;
#33625 = DIRECTION ( 'NONE',  ( -1.000000000000000000, 0.000000000000000000, 0.000000000000000000 ) ) ;
#33626 = EDGE_CURVE ( 'NONE', #28925, #31383, #29431, .T. ) ;
#33627 = DIRECTION ( 'NONE',  ( 1.000000000000000000, 0.000000000000000000, 0.000000000000000000 ) ) ;
#33628 = EDGE_LOOP ( 'NONE', ( #7843, #17564 ) ) ;
#33629 = EDGE_LOOP ( 'NONE', ( #1448, #10686, #1740, #19876 ) ) ;
#33630 = CARTESIAN_POINT ( 'NONE',  ( 49.99999662536848177, -51.96152422706640550, 17.49999999999999645 ) ) ;
#33631 = FACE_OUTER_BOUND ( 'NONE', #31199, .T. ) ;
#33632 = CARTESIAN_POINT ( 'NONE',  ( -40.00000337463113453, -69.28203230275519786, -9.999999999999998224 ) ) ;
#33633 = DIRECTION ( 'NONE',  ( 0.000000000000000000, 0.000000000000000000, 1.000000000000000000 ) ) ;
#33634 = ORIENTED_EDGE ( 'NONE', *, *, #14498, .F. ) ;
#33635 = DIRECTION ( 'NONE',  ( 1.000000000000000000, 0.000000000000000000, 0.000000000000000000 ) ) ;
#33636 = PRODUCT_RELATED_PRODUCT_CATEGORY ( 'part', '', ( #160 ) ) ;
#33637 =( REPRESENTATION_RELATIONSHIP ('NONE','NONE', #15268, #33015 ) REPRESENTATION_RELATIONSHIP_WITH_TRANSFORMATION ( #24299 )SHAPE_REPRESENTATION_RELATIONSHIP( ) );
#33638 = FACE_BOUND ( 'NONE', #2224, .T. ) ;
#33639 = EDGE_CURVE ( 'NONE', #28376, #12615, #1690, .T. ) ;
#33640 = FACE_OUTER_BOUND ( 'NONE', #15452, .T. ) ;
#33641 = CARTESIAN_POINT ( 'NONE',  ( -34.00000000000000000, 103.4105893997321743, 32.50000000000000000 ) ) ;
#33642 = DIRECTION ( 'NONE',  ( 1.000000000000000000, 0.000000000000000000, 0.000000000000000000 ) ) ;
#33643 = CARTESIAN_POINT ( 'NONE',  ( 5.253368672218635460, -3.033033817057790404, -4.359491423763655504 ) ) ;
#33644 = CARTESIAN_POINT ( 'NONE',  ( 2.545083245400402649, 119.9999999808429294, 27.49998800000000188 ) ) ;
#33645 = ADVANCED_FACE ( 'NONE', ( #6575 ), #21372, .F. ) ;
#33646 = CARTESIAN_POINT ( 'NONE',  ( 61.99999662536845335, 34.64101615137759893, -9.999999999999998224 ) ) ;
#33647 = ORIENTED_EDGE ( 'NONE', *, *, #9265, .F. ) ;
#33648 = CARTESIAN_POINT ( 'NONE',  ( -5.000000000000000000, -2.886751345948137981, -5.553418012614792509 ) ) ;
#33649 = AXIS2_PLACEMENT_3D ( 'NONE', #21187, #29056, #26624 ) ;
#33650 = DIRECTION ( 'NONE',  ( 0.000000000000000000, 0.000000000000000000, 1.000000000000000000 ) ) ;
#33651 = CARTESIAN_POINT ( 'NONE',  ( -78.00000337463096400, -34.64101615137762025, 12.50000000000000000 ) ) ;
#33652 = ORIENTED_EDGE ( 'NONE', *, *, #36651, .T. ) ;
#33653 = EDGE_LOOP ( 'NONE', ( #9516, #31200, #10404, #26302, #22941, #797 ) ) ;
#33654 = VERTEX_POINT ( 'NONE', #6744 ) ;
#33655 = DIRECTION ( 'NONE',  ( -1.000000000000000000, 0.000000000000000000, 0.000000000000000000 ) ) ;
#33656 = CARTESIAN_POINT ( 'NONE',  ( -85.00000337463092137, 25.98076211353317433, 12.50000000000000000 ) ) ;
#33657 = EDGE_LOOP ( 'NONE', ( #35079, #14515, #26116, #8608, #7285, #2519, #6809 ) ) ;
#33658 = CARTESIAN_POINT ( 'NONE',  ( -77.00000337463097821, -8.660254037844422825, 17.49999999999999645 ) ) ;
#33659 = ADVANCED_FACE ( 'NONE', ( #32815 ), #21003, .F. ) ;
#33660 = DIRECTION ( 'NONE',  ( -1.000000000000000000, 0.000000000000000000, 0.000000000000000000 ) ) ;
#33661 = ORIENTED_EDGE ( 'NONE', *, *, #419, .F. ) ;
#33662 = DIRECTION ( 'NONE',  ( 0.000000000000000000, 0.000000000000000000, 1.000000000000000000 ) ) ;
#33663 = VERTEX_POINT ( 'NONE', #21570 ) ;
#33664 = DIRECTION ( 'NONE',  ( 0.000000000000000000, 0.000000000000000000, 1.000000000000000000 ) ) ;
#33665 = EDGE_CURVE ( 'NONE', #32142, #8319, #21977, .T. ) ;
#33666 = DIRECTION ( 'NONE',  ( 0.000000000000000000, 0.000000000000000000, -1.000000000000000000 ) ) ;
#33667 = CARTESIAN_POINT ( 'NONE',  ( -10.00000337463125000, -86.60254037844400443, -9.999999999999998224 ) ) ;
#33668 = CIRCLE ( 'NONE', #1323, 5.000000000000000000 ) ;
#33669 = EDGE_CURVE ( 'NONE', #19159, #22352, #16014, .T. ) ;
#33670 = ORIENTED_EDGE ( 'NONE', *, *, #27718, .F. ) ;
#33671 = CARTESIAN_POINT ( 'NONE',  ( -12.00000337463127842, -69.28203230275519786, 12.50000000000000000 ) ) ;
#33672 = DIRECTION ( 'NONE',  ( 0.000000000000000000, 0.000000000000000000, 1.000000000000000000 ) ) ;
#33673 = CARTESIAN_POINT ( 'NONE',  ( -58.00000337463108480, -51.96152422706641971, 12.50000000000000000 ) ) ;
#33674 = ORIENTED_EDGE ( 'NONE', *, *, #14932, .F. ) ;
#33675 = CYLINDRICAL_SURFACE ( 'NONE', #23367, 2.000000000000001776 ) ;
#33676 = DIRECTION ( 'NONE',  ( 1.000000000000000000, 0.000000000000000000, 0.000000000000000000 ) ) ;
#33677 = ORIENTED_EDGE ( 'NONE', *, *, #17151, .F. ) ;
#33678 = CARTESIAN_POINT ( 'NONE',  ( 67.30619744049005249, 84.18124734178236679, 32.50000000000000000 ) ) ;
#33679 = CARTESIAN_POINT ( 'NONE',  ( 24.99999662536859546, -77.94228634059960825, -5.000000000000000000 ) ) ;
#33680 = FACE_OUTER_BOUND ( 'NONE', #25982, .T. ) ;
#33681 = DIRECTION ( 'NONE',  ( 1.000000000000000000, 0.000000000000000000, 0.000000000000000000 ) ) ;
#33682 = CIRCLE ( 'NONE', #17498, 2.000000000000001776 ) ;
#33683 = AXIS2_PLACEMENT_3D ( 'NONE', #25530, #25184, #7916 ) ;
#33684 = VERTEX_POINT ( 'NONE', #36010 ) ;
#33685 = EDGE_CURVE ( 'NONE', #34111, #5560, #32612, .T. ) ;
#33686 = EDGE_LOOP ( 'NONE', ( #32645, #14053, #20974, #32225 ) ) ;
#33687 = CARTESIAN_POINT ( 'NONE',  ( 0.000000000000000000, 0.000000000000000000, 3.400000000000000355 ) ) ;
#33688 = DIRECTION ( 'NONE',  ( 0.000000000000000000, 0.000000000000000000, -1.000000000000000000 ) ) ;
#33689 = DIRECTION ( 'NONE',  ( 0.000000000000000000, 0.000000000000000000, 1.000000000000000000 ) ) ;
#33690 = ORIENTED_EDGE ( 'NONE', *, *, #6435, .T. ) ;
#33691 = ORIENTED_EDGE ( 'NONE', *, *, #7457, .T. ) ;
#33692 = AXIS2_PLACEMENT_3D ( 'NONE', #16890, #33964, #31145 ) ;
#33693 = PLANE ( 'NONE',  #8004 ) ;
#33694 = CARTESIAN_POINT ( 'NONE',  ( 0.000000000000000000, 0.000000000000000000, 0.000000000000000000 ) ) ;
#33695 = DIRECTION ( 'NONE',  ( 0.000000000000000000, 0.000000000000000000, 1.000000000000000000 ) ) ;
#33696 = ORIENTED_EDGE ( 'NONE', *, *, #37042, .F. ) ;
#33697 = EDGE_LOOP ( 'NONE', ( #7989, #12785, #32518, #12267 ) ) ;
#33698 = DIRECTION ( 'NONE',  ( 0.000000000000000000, 0.000000000000000000, 1.000000000000000000 ) ) ;
#33699 = EDGE_CURVE ( 'NONE', #15126, #33094, #18747, .T. ) ;
#33700 = DIRECTION ( 'NONE',  ( -0.000000000000000000, -0.000000000000000000, 1.000000000000000000 ) ) ;
#33701 = EDGE_LOOP ( 'NONE', ( #3257, #6344, #18265, #18855, #26412, #25094, #14343, #20694, #7049 ) ) ;
#33702 = EDGE_CURVE ( 'NONE', #1764, #26494, #26764, .T. ) ;
#33703 = FACE_OUTER_BOUND ( 'NONE', #31476, .T. ) ;
#33704 = EDGE_LOOP ( 'NONE', ( #24239, #12063, #12995, #2350 ) ) ;
#33705 = FACE_BOUND ( 'NONE', #24454, .T. ) ;
#33706 = EDGE_CURVE ( 'NONE', #13025, #17798, #31541, .T. ) ;
#33707 = CIRCLE ( 'NONE', #17527, 3.000000000000002665 ) ;
#33708 = CYLINDRICAL_SURFACE ( 'NONE', #16715, 2.000000000000001776 ) ;
#33709 = EDGE_CURVE ( 'NONE', #4217, #5741, #21736, .T. ) ;
#33710 = CARTESIAN_POINT ( 'NONE',  ( 5.170224855064532221, 2.788471980053852217, -4.289066185948682275 ) ) ;
#33711 = ORIENTED_EDGE ( 'NONE', *, *, #20335, .T. ) ;
#33712 = B_SPLINE_CURVE_WITH_KNOTS ( 'NONE', 3,
 ( #34346, #31515, #20280, #25738, #12003, #31330 ),
 .UNSPECIFIED., .F., .F.,
 ( 4, 2, 4 ),
 ( 0.005150343764683553392, 0.006610526168996383109, 0.008070708573309213693 ),
 .UNSPECIFIED. ) ;
#33713 = EDGE_CURVE ( 'NONE', #21017, #19227, #36360, .T. ) ;
#33714 = DIRECTION ( 'NONE',  ( 0.000000000000000000, 0.000000000000000000, 1.000000000000000000 ) ) ;
#33715 = CARTESIAN_POINT ( 'NONE',  ( -35.19434990244938888, 52.39915983220783602, -4.999999999999997335 ) ) ;
#33716 = AXIS2_PLACEMENT_3D ( 'NONE', #6481, #18475, #26710 ) ;
#33717 = DIRECTION ( 'NONE',  ( -0.000000000000000000, 0.000000000000000000, -1.000000000000000000 ) ) ;
#33718 = CARTESIAN_POINT ( 'NONE',  ( 19.99999662536861678, -86.60254037844400443, -9.999999999999998224 ) ) ;
#33719 = EDGE_LOOP ( 'NONE', ( #33981, #2315 ) ) ;
#33720 = VECTOR ( 'NONE', #16943, 1000.000000000000000 ) ;
#33721 = CARTESIAN_POINT ( 'NONE',  ( -73.00000337463097821, 43.30127018922197379, -5.000000000000000000 ) ) ;
#33722 = DIRECTION ( 'NONE',  ( 0.000000000000000000, 0.000000000000000000, -1.000000000000000000 ) ) ;
#33723 = DIRECTION ( 'NONE',  ( 0.000000000000000000, 0.000000000000000000, -1.000000000000000000 ) ) ;
#33724 = EDGE_CURVE ( 'NONE', #29503, #7561, #26618, .T. ) ;
#33725 = EDGE_CURVE ( 'NONE', #13179, #20167, #10007, .T. ) ;
#33726 = ORIENTED_EDGE ( 'NONE', *, *, #12341, .F. ) ;
#33727 = ORIENTED_EDGE ( 'NONE', *, *, #8737, .F. ) ;
#33728 = EDGE_CURVE ( 'NONE', #30219, #23050, #26819, .T. ) ;
#33729 = EDGE_CURVE ( 'NONE', #29705, #25264, #32156, .T. ) ;
#33730 = DIRECTION ( 'NONE',  ( -0.000000000000000000, -0.000000000000000000, 1.000000000000000000 ) ) ;
#33732 = EDGE_CURVE ( 'NONE', #9870, #16004, #2599, .T. ) ;
#33731 = ORIENTED_EDGE ( 'NONE', *, *, #31274, .T. ) ;
#33733 = CARTESIAN_POINT ( 'NONE',  ( -65.00000337463102085, 43.30127018922198801, -5.000000000000000000 ) ) ;
#33734 = VECTOR ( 'NONE', #11131, 1000.000000000000000 ) ;
#33735 = FACE_OUTER_BOUND ( 'NONE', #14678, .T. ) ;
#33736 = AXIS2_PLACEMENT_3D ( 'NONE', #29212, #28833, #25686 ) ;
#33737 = DIRECTION ( 'NONE',  ( -1.000000000000000000, 0.000000000000000000, 0.000000000000000000 ) ) ;
#33738 = CARTESIAN_POINT ( 'NONE',  ( -22.00000337463124112, 69.28203230275516944, 17.49999999999999645 ) ) ;
#33739 = CYLINDRICAL_SURFACE ( 'NONE', #9503, 2.000000000000001776 ) ;
#33740 = CARTESIAN_POINT ( 'NONE',  ( 81.86307328356785717, -18.04779437809804676, -5.000000000000000000 ) ) ;
#33741 = CARTESIAN_POINT ( 'NONE',  ( -6.216324218022825094E-15, 6.066067634115565710, -4.359491423763658169 ) ) ;
#33742 = CARTESIAN_POINT ( 'NONE',  ( -75.00000337463100664, -43.30127018922202353, -9.999999999999998224 ) ) ;
#33743 = ORIENTED_EDGE ( 'NONE', *, *, #27502, .F. ) ;
#33744 = ORIENTED_EDGE ( 'NONE', *, *, #27, .T. ) ;
#33745 =( NAMED_UNIT ( * ) SI_UNIT ( $, .STERADIAN. ) SOLID_ANGLE_UNIT ( ) );
#33746 = AXIS2_PLACEMENT_3D ( 'NONE', #7176, #26305, #35493 ) ;
#33747 = LINE ( 'NONE', #11037, #24741 ) ;
#33748 = CYLINDRICAL_SURFACE ( 'NONE', #10861, 2.000000000000000000 ) ;
#33749 = CARTESIAN_POINT ( 'NONE',  ( -78.00000337463094979, -2.428612866367529932E-14, -9.999999999999998224 ) ) ;
#33750 = ORIENTED_EDGE ( 'NONE', *, *, #29584, .F. ) ;
#33751 = CYLINDRICAL_SURFACE ( 'NONE', #26366, 2.000000000000001776 ) ;
#33752 = ORIENTED_EDGE ( 'NONE', *, *, #30146, .F. ) ;
#33753 = ORIENTED_EDGE ( 'NONE', *, *, #9481, .T. ) ;
#33754 = CARTESIAN_POINT ( 'NONE',  ( -6.726859516510129922, 0.000000000000000000, -4.599999999999999645 ) ) ;
#33755 = AXIS2_PLACEMENT_3D ( 'NONE', #3793, #15795, #628 ) ;
#33756 = VERTEX_POINT ( 'NONE', #36375 ) ;
#33757 = CARTESIAN_POINT ( 'NONE',  ( 19.99999662536861678, -69.28203230275519786, -5.000000000000000000 ) ) ;
#33758 = AXIS2_PLACEMENT_3D ( 'NONE', #22626, #33876, #5000 ) ;
#33759 = CARTESIAN_POINT ( 'NONE',  ( 0.000000000000000000, 0.000000000000000000, -5.000000000000000000 ) ) ;
#33760 = FACE_OUTER_BOUND ( 'NONE', #20813, .T. ) ;
#33761 = EDGE_LOOP ( 'NONE', ( #22895, #23962 ) ) ;
#33762 = EDGE_CURVE ( 'NONE', #3254, #15973, #22591, .T. ) ;
#33763 = ORIENTED_EDGE ( 'NONE', *, *, #14456, .F. ) ;
#33764 = ORIENTED_EDGE ( 'NONE', *, *, #15522, .F. ) ;
#33765 = EDGE_CURVE ( 'NONE', #23824, #18795, #11226, .T. ) ;
#33766 = ORIENTED_EDGE ( 'NONE', *, *, #12311, .F. ) ;
#33767 = CARTESIAN_POINT ( 'NONE',  ( 72.99999662536836809, -8.660254037844401509, -5.000000000000000000 ) ) ;
#33768 = TOROIDAL_SURFACE ( 'NONE', #27784, 3.250000000000001332, 0.2500000000000000000 ) ;
#33769 = EDGE_CURVE ( 'NONE', #15901, #10971, #8226, .T. ) ;
#33770 = LINE ( 'NONE', #19519, #35945 ) ;
#33771 = CARTESIAN_POINT ( 'NONE',  ( -77.00000337463097821, -8.660254037844422825, -9.999999999999998224 ) ) ;
#33772 = DIRECTION ( 'NONE',  ( 0.000000000000000000, 0.000000000000000000, 1.000000000000000000 ) ) ;
#33773 = CARTESIAN_POINT ( 'NONE',  ( 32.99999662536855283, -77.94228634059960825, -9.999999999999998224 ) ) ;
#33774 = EDGE_LOOP ( 'NONE', ( #16259, #5200, #36900 ) ) ;
#33775 = DIRECTION ( 'NONE',  ( 0.000000000000000000, 0.000000000000000000, 1.000000000000000000 ) ) ;
#33776 = DIRECTION ( 'NONE',  ( -0.000000000000000000, -0.000000000000000000, -1.000000000000000000 ) ) ;
#33777 = CARTESIAN_POINT ( 'NONE',  ( 44.13139720814418610, 27.49999999999988987, -15.00000000000000000 ) ) ;
#33778 = ORIENTED_EDGE ( 'NONE', *, *, #16747, .T. ) ;
#33779 = DIRECTION ( 'NONE',  ( 0.000000000000000000, -0.000000000000000000, -1.000000000000000000 ) ) ;
#33780 = CARTESIAN_POINT ( 'NONE',  ( -35.19434990244938888, 52.39915983220783602, -49.22241343995295892 ) ) ;
#33781 = ORIENTED_EDGE ( 'NONE', *, *, #24113, .T. ) ;
#33782 = VECTOR ( 'NONE', #7835, 1000.000000000000000 ) ;
#33783 = ORIENTED_EDGE ( 'NONE', *, *, #33157, .T. ) ;
#33784 = CARTESIAN_POINT ( 'NONE',  ( 76.99999662536835388, -43.30127018922199511, -9.999999999999998224 ) ) ;
#33785 = DIRECTION ( 'NONE',  ( 0.8660254037844415942, 0.4999999999999949485, 0.000000000000000000 ) ) ;
#33786 = CARTESIAN_POINT ( 'NONE',  ( -68.00000000000000000, 0.000000000000000000, -49.86348611802629449 ) ) ;
#33787 = CARTESIAN_POINT ( 'NONE',  ( -4.651285141664999401, -3.088081963278269004, -1.686035282245272215 ) ) ;
#33788 = ORIENTED_EDGE ( 'NONE', *, *, #11493, .F. ) ;
#33789 = ORIENTED_EDGE ( 'NONE', *, *, #13494, .F. ) ;
#33790 = EDGE_CURVE ( 'NONE', #22817, #24238, #13677, .T. ) ;
#33791 = CIRCLE ( 'NONE', #27186, 2.000000000000001776 ) ;
#33792 = FACE_BOUND ( 'NONE', #17543, .T. ) ;
#33793 = VECTOR ( 'NONE', #2639, 1000.000000000000000 ) ;
#33794 = EDGE_LOOP ( 'NONE', ( #9935, #36134, #35884, #3986, #35606 ) ) ;
#33795 = DIRECTION ( 'NONE',  ( -0.000000000000000000, -0.000000000000000000, 1.000000000000000000 ) ) ;
#33796 = ORIENTED_EDGE ( 'NONE', *, *, #31672, .F. ) ;
#33797 = ORIENTED_EDGE ( 'NONE', *, *, #8150, .T. ) ;
#33798 = EDGE_CURVE ( 'NONE', #28579, #10948, #11208, .T. ) ;
#33799 = DIRECTION ( 'NONE',  ( 1.000000000000000000, 0.000000000000000000, 0.000000000000000000 ) ) ;
#33800 = LINE ( 'NONE', #8317, #36427 ) ;
#33801 = VERTEX_POINT ( 'NONE', #13473 ) ;
#33802 = VECTOR ( 'NONE', #3915, 1000.000000000000000 ) ;
#33803 = VERTEX_POINT ( 'NONE', #33168 ) ;
#33804 = DIRECTION ( 'NONE',  ( 1.000000000000000000, 0.000000000000000000, 0.000000000000000000 ) ) ;
#33805 = CARTESIAN_POINT ( 'NONE',  ( 17.99999662536858125, 86.60254037844397601, -9.999999999999998224 ) ) ;
#33806 = CARTESIAN_POINT ( 'NONE',  ( -37.00000337463116296, -60.62177826491080168, -9.999999999999998224 ) ) ;
#33807 = CARTESIAN_POINT ( 'NONE',  ( 4.185558440016312609, 3.356969399843928059, -0.2680587191991100071 ) ) ;
#33808 = CIRCLE ( 'NONE', #15218, 3.000000000000002665 ) ;
#33809 = EDGE_LOOP ( 'NONE', ( #1923, #29839, #14055, #3977, #4203, #16901 ) ) ;
#33810 = CYLINDRICAL_SURFACE ( 'NONE', #18349, 2.000000000000001776 ) ;
#33811 = EDGE_CURVE ( 'NONE', #35409, #12497, #19483, .T. ) ;
#33812 = FACE_BOUND ( 'NONE', #22315, .T. ) ;
#33813 = DIRECTION ( 'NONE',  ( 0.000000000000000000, 0.000000000000000000, 1.000000000000000000 ) ) ;
#33814 = FACE_OUTER_BOUND ( 'NONE', #1782, .T. ) ;
#33815 = DIRECTION ( 'NONE',  ( -1.000000000000000000, 0.000000000000000000, 0.000000000000000000 ) ) ;
#33816 = CARTESIAN_POINT ( 'NONE',  ( 79.99999662536833966, -3.469446951953614189E-15, 17.49999999999999645 ) ) ;
#33817 = AXIS2_PLACEMENT_3D ( 'NONE', #26040, #23045, #18154 ) ;
#33818 = AXIS2_PLACEMENT_3D ( 'NONE', #35607, #29969, #1457 ) ;
#33819 = DIRECTION ( 'NONE',  ( 0.000000000000000000, 0.000000000000000000, 1.000000000000000000 ) ) ;
#33820 = CIRCLE ( 'NONE', #17631, 2.000000000000000000 ) ;
#33821 = DIRECTION ( 'NONE',  ( 1.000000000000000000, 0.000000000000000000, 0.000000000000000000 ) ) ;
#33822 = EDGE_LOOP ( 'NONE', ( #16449, #5536 ) ) ;
#33823 = FACE_OUTER_BOUND ( 'NONE', #7337, .T. ) ;
#33824 = CARTESIAN_POINT ( 'NONE',  ( 62.97617850287784336, 4.279621169095339184, 12.49999999999999822 ) ) ;
#33825 = DIRECTION ( 'NONE',  ( -1.000000000000000000, 0.000000000000000000, 0.000000000000000000 ) ) ;
#33826 = ORIENTED_EDGE ( 'NONE', *, *, #2006, .T. ) ;
#33827 = ORIENTED_EDGE ( 'NONE', *, *, #33725, .T. ) ;
#33828 = ORIENTED_EDGE ( 'NONE', *, *, #9178, .T. ) ;
#33829 = AXIS2_PLACEMENT_3D ( 'NONE', #7128, #10129, #21562 ) ;
#33830 = EDGE_CURVE ( 'NONE', #14157, #28556, #13623, .T. ) ;
#33831 = FACE_OUTER_BOUND ( 'NONE', #25356, .T. ) ;
#33832 = CARTESIAN_POINT ( 'NONE',  ( 47.63139720814400846, -27.50000000000022737, 5.000000000000000888 ) ) ;
#33833 = AXIS2_PLACEMENT_3D ( 'NONE', #19977, #23163, #2548 ) ;
#33834 = ORIENTED_EDGE ( 'NONE', *, *, #10098, .F. ) ;
#33835 = ADVANCED_FACE ( 'NONE', ( #7489 ), #7687, .F. ) ;
#33836 = AXIS2_PLACEMENT_3D ( 'NONE', #26442, #23453, #6939 ) ;
#33837 = CARTESIAN_POINT ( 'NONE',  ( 37.99999662536853151, -69.28203230275519786, -9.999999999999998224 ) ) ;
#33838 = ORIENTED_EDGE ( 'NONE', *, *, #4077, .F. ) ;
#33839 = CARTESIAN_POINT ( 'NONE',  ( -75.00000337463099243, -25.98076211353322051, -9.999999999999998224 ) ) ;
#33840 = EDGE_CURVE ( 'NONE', #15693, #12600, #445, .T. ) ;
#33841 = ORIENTED_EDGE ( 'NONE', *, *, #33865, .T. ) ;
#33842 = DIRECTION ( 'NONE',  ( 0.000000000000000000, 0.000000000000000000, 1.000000000000000000 ) ) ;
#33843 = AXIS2_PLACEMENT_3D ( 'NONE', #25657, #24909, #8018 ) ;
#33844 = AXIS2_PLACEMENT_3D ( 'NONE', #6638, #12431, #23343 ) ;
#33845 = EDGE_CURVE ( 'NONE', #17855, #30871, #25331, .T. ) ;
#33846 = DIRECTION ( 'NONE',  ( 0.000000000000000000, 0.000000000000000000, 1.000000000000000000 ) ) ;
#33847 = CARTESIAN_POINT ( 'NONE',  ( 46.99999662536849598, 60.62177826491077326, 12.50000000000000000 ) ) ;
#33848 = ORIENTED_EDGE ( 'NONE', *, *, #1611, .F. ) ;
#33849 = CARTESIAN_POINT ( 'NONE',  ( -85.00000337463092137, -8.660254037844422825, -9.999999999999998224 ) ) ;
#33850 = DIRECTION ( 'NONE',  ( -1.000000000000000000, 0.000000000000000000, 0.000000000000000000 ) ) ;
#33851 = CARTESIAN_POINT ( 'NONE',  ( 46.99999662536851019, 77.94228634059959404, -5.000000000000000000 ) ) ;
#33852 = ORIENTED_EDGE ( 'NONE', *, *, #6392, .T. ) ;
#33853 = DIRECTION ( 'NONE',  ( 0.000000000000000000, -0.000000000000000000, -1.000000000000000000 ) ) ;
#33854 = DIRECTION ( 'NONE',  ( 0.000000000000000000, 0.000000000000000000, -1.000000000000000000 ) ) ;
#33855 = VERTEX_POINT ( 'NONE', #16138 ) ;
#33856 = EDGE_CURVE ( 'NONE', #22350, #24339, #30405, .T. ) ;
#33857 = DIRECTION ( 'NONE',  ( 0.000000000000000000, 0.000000000000000000, -1.000000000000000000 ) ) ;
#33858 = CIRCLE ( 'NONE', #22470, 3.500000000000003109 ) ;
#33859 = DIRECTION ( 'NONE',  ( 0.000000000000000000, 0.000000000000000000, -1.000000000000000000 ) ) ;
#33860 = CARTESIAN_POINT ( 'NONE',  ( 0.000000000000000000, 0.000000000000000000, -5.000000000000000000 ) ) ;
#33861 = VECTOR ( 'NONE', #18998, 1000.000000000000000 ) ;
#33862 = CIRCLE ( 'NONE', #35063, 25.00000000000000000 ) ;
#33863 = FACE_OUTER_BOUND ( 'NONE', #20780, .T. ) ;
#33864 = COLOUR_RGB ( '', 0.66274510, 0.83137255, 0.94901961) ;
#33865 = EDGE_CURVE ( 'NONE', #20872, #22736, #10862, .T. ) ;
#33866 = ORIENTED_EDGE ( 'NONE', *, *, #24016, .T. ) ;
#33867 = ORIENTED_EDGE ( 'NONE', *, *, #31286, .T. ) ;
#33868 = DIRECTION ( 'NONE',  ( -0.000000000000000000, -0.000000000000000000, 1.000000000000000000 ) ) ;
#33869 = CIRCLE ( 'NONE', #11682, 33.00000000000001421 ) ;
#33870 = DIRECTION ( 'NONE',  ( 0.000000000000000000, 0.000000000000000000, 1.000000000000000000 ) ) ;
#33871 = AXIS2_PLACEMENT_3D ( 'NONE', #24864, #36303, #10612 ) ;
#33872 = EDGE_CURVE ( 'NONE', #7967, #23429, #32787, .T. ) ;
#33873 = ORIENTED_EDGE ( 'NONE', *, *, #22291, .F. ) ;
#33874 = ORIENTED_EDGE ( 'NONE', *, *, #19544, .T. ) ;
#33875 = EDGE_CURVE ( 'NONE', #12924, #22186, #16682, .T. ) ;
#33876 = DIRECTION ( 'NONE',  ( -0.000000000000000000, -0.000000000000000000, 1.000000000000000000 ) ) ;
#33877 = DIRECTION ( 'NONE',  ( -0.000000000000000000, -0.000000000000000000, -1.000000000000000000 ) ) ;
#33878 = CYLINDRICAL_SURFACE ( 'NONE', #881, 2.000000000000001776 ) ;
#33879 = VERTEX_POINT ( 'NONE', #16309 ) ;
#33880 = EDGE_CURVE ( 'NONE', #25896, #30809, #22126, .T. ) ;
#33881 = ORIENTED_EDGE ( 'NONE', *, *, #13231, .F. ) ;
#33882 = CARTESIAN_POINT ( 'NONE',  ( -56.13646009116099123, 70.47608876694653190, -49.22241343995295892 ) ) ;
#33883 = CIRCLE ( 'NONE', #17698, 2.000000000000000000 ) ;
#33884 = CARTESIAN_POINT ( 'NONE',  ( -75.00000337463097821, 8.660254037844374864, -9.999999999999998224 ) ) ;
#33885 = EDGE_LOOP ( 'NONE', ( #13789, #21910 ) ) ;
#33886 = AXIS2_PLACEMENT_3D ( 'NONE', #17441, #15178, #14448 ) ;
#33887 = DIRECTION ( 'NONE',  ( -0.000000000000000000, -0.000000000000000000, 1.000000000000000000 ) ) ;
#33888 = EDGE_CURVE ( 'NONE', #20625, #14287, #17818, .T. ) ;
#33889 = ORIENTED_EDGE ( 'NONE', *, *, #1622, .F. ) ;
#33890 = FACE_BOUND ( 'NONE', #7224, .T. ) ;
#33891 = CIRCLE ( 'NONE', #24928, 2.000000000000001776 ) ;
#33892 = VECTOR ( 'NONE', #22220, 1000.000000000000000 ) ;
#33893 = AXIS2_PLACEMENT_3D ( 'NONE', #32770, #30128, #2005 ) ;
#33894 = EDGE_CURVE ( 'NONE', #29300, #19586, #18422, .T. ) ;
#33895 = LINE ( 'NONE', #5570, #35300 ) ;
#33896 = VERTEX_POINT ( 'NONE', #9136 ) ;
#33897 = DIRECTION ( 'NONE',  ( 0.6664934940021842724, -0.7455108466365599762, 0.000000000000000000 ) ) ;
#33898 = AXIS2_PLACEMENT_3D ( 'NONE', #7455, #27694, #30692 ) ;
#33899 = DIRECTION ( 'NONE',  ( 1.000000000000000000, 0.000000000000000000, 0.000000000000000000 ) ) ;
#33900 = DIRECTION ( 'NONE',  ( 0.4999999999999919509, -0.8660254037844432595, 0.000000000000000000 ) ) ;
#33901 = CARTESIAN_POINT ( 'NONE',  ( 95.00000000000001421, 0.000000000000000000, -10.00000000000000000 ) ) ;
#33902 = ORIENTED_EDGE ( 'NONE', *, *, #8726, .F. ) ;
#33903 = CARTESIAN_POINT ( 'NONE',  ( 37.27962116909601065, -62.97617850287780072, -4.999999999999997335 ) ) ;
#33904 = FACE_OUTER_BOUND ( 'NONE', #27744, .T. ) ;
#33905 = DIRECTION ( 'NONE',  ( 0.000000000000000000, 0.000000000000000000, 1.000000000000000000 ) ) ;
#33906 = EDGE_LOOP ( 'NONE', ( #3088, #36413, #4406, #10221 ) ) ;
#33907 = EDGE_CURVE ( 'NONE', #13265, #36317, #33384, .T. ) ;
#33908 = ORIENTED_EDGE ( 'NONE', *, *, #34071, .T. ) ;
#33909 = AXIS2_PLACEMENT_3D ( 'NONE', #26105, #34753, #32077 ) ;
#33910 = DIRECTION ( 'NONE',  ( 0.000000000000000000, 0.000000000000000000, -1.000000000000000000 ) ) ;
#33911 = ORIENTED_EDGE ( 'NONE', *, *, #4256, .T. ) ;
#33912 = PRESENTATION_LAYER_ASSIGNMENT (  '', '', ( #5256 ) ) ;
#33913 = DIRECTION ( 'NONE',  ( 0.000000000000000000, 0.000000000000000000, 1.000000000000000000 ) ) ;
#33914 = AXIS2_PLACEMENT_3D ( 'NONE', #10230, #30469, #4603 ) ;
#33915 = CARTESIAN_POINT ( 'NONE',  ( 16.99999662536863454, -77.94228634059960825, -5.000000000000000000 ) ) ;
#33916 = CIRCLE ( 'NONE', #32697, 30.00000000000000000 ) ;
#33917 = ADVANCED_FACE ( 'NONE', ( #23219 ), #17027, .F. ) ;
#33918 = CIRCLE ( 'NONE', #21323, 2.000000000000001776 ) ;
#33919 = DIRECTION ( 'NONE',  ( 1.000000000000000000, 0.000000000000000000, 0.000000000000000000 ) ) ;
#33920 = CYLINDRICAL_SURFACE ( 'NONE', #17053, 2.000000000000001776 ) ;
#33921 = ADVANCED_FACE ( 'NONE', ( #31649 ), #14771, .F. ) ;
#33922 = CARTESIAN_POINT ( 'NONE',  ( 88.66502283662251216, -71.67713940050370525, 32.50000000000000000 ) ) ;
#33923 = CARTESIAN_POINT ( 'NONE',  ( -97.64058335231293029, -67.22370022648394183, 32.49999999999999289 ) ) ;
#33924 = EDGE_CURVE ( 'NONE', #31223, #29568, #2848, .T. ) ;
#33925 = DIRECTION ( 'NONE',  ( 0.9396926207859139790, 1.150791560227857172E-16, -0.3420201433256533918 ) ) ;
#33926 = DIRECTION ( 'NONE',  ( 0.000000000000000000, 0.000000000000000000, -1.000000000000000000 ) ) ;
#33927 = EDGE_LOOP ( 'NONE', ( #8960, #34428, #11959, #6189 ) ) ;
#33928 = VECTOR ( 'NONE', #31565, 1000.000000000000000 ) ;
#33929 = ORIENTED_EDGE ( 'NONE', *, *, #404, .T. ) ;
#33930 = CARTESIAN_POINT ( 'NONE',  ( -18.00000337463123756, -69.28203230275522628, -9.999999999999998224 ) ) ;
#33931 = DIRECTION ( 'NONE',  ( 0.000000000000000000, 0.000000000000000000, 1.000000000000000000 ) ) ;
#33932 = CARTESIAN_POINT ( 'NONE',  ( 19.99999662536858835, 69.28203230275516944, -5.000000000000000000 ) ) ;
#33933 = CARTESIAN_POINT ( 'NONE',  ( 24.99999662536859546, -77.94228634059960825, -9.999999999999998224 ) ) ;
#33934 = VERTEX_POINT ( 'NONE', #25680 ) ;
#33935 = UNCERTAINTY_MEASURE_WITH_UNIT (LENGTH_MEASURE( 1.000000000000000082E-05 ), #21900, 'distance_accuracy_value', 'NONE');
#33936 = VECTOR ( 'NONE', #20845, 1000.000000000000000 ) ;
#33937 = EDGE_CURVE ( 'NONE', #15730, #31817, #36998, .T. ) ;
#33938 = CIRCLE ( 'NONE', #5805, 2.000000000000001776 ) ;
#33939 = FACE_BOUND ( 'NONE', #12395, .T. ) ;
#33940 = ORIENTED_EDGE ( 'NONE', *, *, #3236, .F. ) ;
#33941 = ORIENTED_EDGE ( 'NONE', *, *, #34196, .T. ) ;
#33942 =( GEOMETRIC_REPRESENTATION_CONTEXT ( 3 ) GLOBAL_UNCERTAINTY_ASSIGNED_CONTEXT ( ( #4708 ) ) GLOBAL_UNIT_ASSIGNED_CONTEXT ( ( #33345, #24156, #27885 ) ) REPRESENTATION_CONTEXT ( 'NONE', 'WORKASPACE' ) );
#33943 = CARTESIAN_POINT ( 'NONE',  ( -15.97563234535668109, 90.60231327712331506, -49.86561046011506448 ) ) ;
#33944 = ORIENTED_EDGE ( 'NONE', *, *, #6554, .T. ) ;
#33945 = AXIS2_PLACEMENT_3D ( 'NONE', #34744, #14305, #11836 ) ;
#33947 = AXIS2_PLACEMENT_3D ( 'NONE', #19983, #31405, #13620 ) ;
#33946 =( NAMED_UNIT ( * ) PLANE_ANGLE_UNIT ( ) SI_UNIT ( $, .RADIAN. ) );
#33948 = DIRECTION ( 'NONE',  ( 0.000000000000000000, 0.000000000000000000, 1.000000000000000000 ) ) ;
#33949 = AXIS2_PLACEMENT_3D ( 'NONE', #1912, #24790, #36223 ) ;
#33950 = PLANE ( 'NONE',  #3244 ) ;
#33951 = AXIS2_PLACEMENT_3D ( 'NONE', #33860, #16074, #24874 ) ;
#33952 = LINE ( 'NONE', #2454, #23271 ) ;
#33953 = ORIENTED_EDGE ( 'NONE', *, *, #4764, .T. ) ;
#33954 = ORIENTED_EDGE ( 'NONE', *, *, #33451, .F. ) ;
#33955 = ORIENTED_EDGE ( 'NONE', *, *, #27943, .T. ) ;
#33956 = CIRCLE ( 'NONE', #4026, 2.000000000000001776 ) ;
#33957 = ORIENTED_EDGE ( 'NONE', *, *, #27873, .F. ) ;
#33958 = EDGE_CURVE ( 'NONE', #30809, #9993, #23798, .T. ) ;
#33959 = ORIENTED_EDGE ( 'NONE', *, *, #642, .T. ) ;
#33960 = CARTESIAN_POINT ( 'NONE',  ( 3.000000000000000000, 4.131365146527188963E-15, 2.541999999999999371 ) ) ;
#33961 = DIRECTION ( 'NONE',  ( 1.000000000000000000, 0.000000000000000000, 0.000000000000000000 ) ) ;
#33962 = ADVANCED_FACE ( 'NONE', ( #33354 ), #28460, .F. ) ;
#33963 = DIRECTION ( 'NONE',  ( 0.000000000000000000, 0.000000000000000000, 1.000000000000000000 ) ) ;
#33964 = DIRECTION ( 'NONE',  ( 0.000000000000000000, 0.000000000000000000, 1.000000000000000000 ) ) ;
#33965 = DIRECTION ( 'NONE',  ( 1.000000000000000000, 0.000000000000000000, 0.000000000000000000 ) ) ;
#33966 = VECTOR ( 'NONE', #17376, 1000.000000000000000 ) ;
#33967 = ORIENTED_EDGE ( 'NONE', *, *, #28451, .T. ) ;
#33968 = DIRECTION ( 'NONE',  ( 0.000000000000000000, 0.000000000000000000, 1.000000000000000000 ) ) ;
#33969 = CIRCLE ( 'NONE', #36964, 2.000000000000001776 ) ;
#33970 = DIRECTION ( 'NONE',  ( -0.000000000000000000, -0.000000000000000000, 1.000000000000000000 ) ) ;
#33971 = AXIS2_PLACEMENT_3D ( 'NONE', #836, #18088, #9485 ) ;
#33972 = AXIS2_PLACEMENT_3D ( 'NONE', #30984, #28338, #5316 ) ;
#33973 = CARTESIAN_POINT ( 'NONE',  ( -40.98360655737705827, 111.1639425680974398, 27.49999999999999645 ) ) ;
#33974 = ORIENTED_EDGE ( 'NONE', *, *, #18253, .F. ) ;
#33975 = CARTESIAN_POINT ( 'NONE',  ( 5.999999999999999112, 0.000000000000000000, -3.250000000000001332 ) ) ;
#33976 = EDGE_CURVE ( 'NONE', #29874, #25059, #29776, .T. ) ;
#33977 = DIRECTION ( 'NONE',  ( -0.000000000000000000, -0.000000000000000000, 1.000000000000000000 ) ) ;
#33978 = DIRECTION ( 'NONE',  ( 0.000000000000000000, 0.000000000000000000, 1.000000000000000000 ) ) ;
#33979 = ORIENTED_EDGE ( 'NONE', *, *, #18555, .F. ) ;
#33980 = AXIS2_PLACEMENT_3D ( 'NONE', #29996, #18008, #15185 ) ;
#33981 = ORIENTED_EDGE ( 'NONE', *, *, #27672, .T. ) ;
#33982 = CIRCLE ( 'NONE', #14211, 2.445500000000000007 ) ;
#33983 = CYLINDRICAL_SURFACE ( 'NONE', #9871, 2.000000000000001776 ) ;
#33984 = CARTESIAN_POINT ( 'NONE',  ( -3.417629563431864526, 3.800333343458438762, -3.719399823475518119 ) ) ;
#33985 = CARTESIAN_POINT ( 'NONE',  ( -20.00000337463124112, 69.28203230275516944, -9.999999999999998224 ) ) ;
#33986 = DIRECTION ( 'NONE',  ( 1.000000000000000000, 0.000000000000000000, 0.000000000000000000 ) ) ;
#33987 = ORIENTED_EDGE ( 'NONE', *, *, #1219, .T. ) ;
#33988 = VERTEX_POINT ( 'NONE', #17575 ) ;
#33989 = EDGE_CURVE ( 'NONE', #29105, #32624, #16044, .T. ) ;
#33990 = TOROIDAL_SURFACE ( 'NONE', #10022, 17.55872235085560007, 2.000000000000000000 ) ;
#33991 = EDGE_CURVE ( 'NONE', #31244, #17078, #5595, .T. ) ;
#33992 = FACE_OUTER_BOUND ( 'NONE', #17501, .T. ) ;
#33993 = EDGE_CURVE ( 'NONE', #7521, #17956, #6326, .T. ) ;
#33994 = AXIS2_PLACEMENT_3D ( 'NONE', #4195, #32101, #15623 ) ;
#33995 = ORIENTED_EDGE ( 'NONE', *, *, #9882, .T. ) ;
#33996 = ADVANCED_FACE ( 'NONE', ( #22855 ), #34123, .T. ) ;
#33997 = AXIS2_PLACEMENT_3D ( 'NONE', #7023, #7386, #16023 ) ;
#33998 = DIRECTION ( 'NONE',  ( 0.000000000000000000, 0.000000000000000000, 1.000000000000000000 ) ) ;
#33999 = ORIENTED_EDGE ( 'NONE', *, *, #9041, .T. ) ;
#34000 = AXIS2_PLACEMENT_3D ( 'NONE', #27707, #2024, #23653 ) ;
#34001 = ORIENTED_EDGE ( 'NONE', *, *, #15653, .T. ) ;
#34002 = DIRECTION ( 'NONE',  ( 0.000000000000000000, 0.000000000000000000, 1.000000000000000000 ) ) ;
#34003 = CIRCLE ( 'NONE', #33402, 2.000000000000001776 ) ;
#34004 = DIRECTION ( 'NONE',  ( 3.491481338843133355E-15, 1.000000000000000000, 0.000000000000000000 ) ) ;
#34005 = ORIENTED_EDGE ( 'NONE', *, *, #16403, .F. ) ;
#34006 = VERTEX_POINT ( 'NONE', #31988 ) ;
#34007 = CARTESIAN_POINT ( 'NONE',  ( -65.00000337463102085, 25.98076211353317433, -9.999999999999998224 ) ) ;
#34008 = DIRECTION ( 'NONE',  ( 0.000000000000000000, 0.000000000000000000, 1.000000000000000000 ) ) ;
#34009 = CARTESIAN_POINT ( 'NONE',  ( 34.99999662536855283, -77.94228634059960825, 12.50000000000000000 ) ) ;
#34010 = CARTESIAN_POINT ( 'NONE',  ( -77.00000337463099243, -25.98076211353322051, -9.999999999999998224 ) ) ;
#34011 = AXIS2_PLACEMENT_3D ( 'NONE', #31176, #25007, #33625 ) ;
#34012 = ORIENTED_EDGE ( 'NONE', *, *, #13537, .T. ) ;
#34013 = LINE ( 'NONE', #17114, #34518 ) ;
#34014 = FACE_BOUND ( 'NONE', #22093, .T. ) ;
#34015 = CARTESIAN_POINT ( 'NONE',  ( 49.99999662536848177, -51.96152422706640550, -9.999999999999998224 ) ) ;
#34016 = DIRECTION ( 'NONE',  ( 0.000000000000000000, 0.000000000000000000, 1.000000000000000000 ) ) ;
#34017 = AXIS2_PLACEMENT_3D ( 'NONE', #27071, #24083, #21077 ) ;
#34018 = CARTESIAN_POINT ( 'NONE',  ( 86.45172111230354517, -31.46585318596159553, 12.49999999999999822 ) ) ;
#34019 = EDGE_CURVE ( 'NONE', #22880, #18795, #14223, .T. ) ;
#34020 = CARTESIAN_POINT ( 'NONE',  ( 84.99999662536832545, 25.98076211353319565, -9.999999999999998224 ) ) ;
#34021 = PRODUCT ( 'torque nut 04-2_iso_ISO 7043-M6-N', 'torque nut 04-2_iso_ISO 7043-M6-N', '', ( #28979 ) ) ;
#34022 = DIRECTION ( 'NONE',  ( 1.000000000000000000, 0.000000000000000000, 0.000000000000000000 ) ) ;
#34023 = AXIS2_PLACEMENT_3D ( 'NONE', #35873, #991, #9792 ) ;
#34024 = DIRECTION ( 'NONE',  ( 0.000000000000000000, 0.000000000000000000, 1.000000000000000000 ) ) ;
#34025 = ORIENTED_EDGE ( 'NONE', *, *, #27656, .F. ) ;
#34026 = DIRECTION ( 'NONE',  ( 0.000000000000000000, 0.000000000000000000, 1.000000000000000000 ) ) ;
#34027 = CIRCLE ( 'NONE', #9473, 2.000000000000001776 ) ;
#34028 = CARTESIAN_POINT ( 'NONE',  ( -40.00000337463113453, -69.28203230275519786, 12.50000000000000000 ) ) ;
#34029 = CARTESIAN_POINT ( 'NONE',  ( 4.999996625368676284, -77.94228634059960825, 17.49999999999999645 ) ) ;
#34030 = AXIS2_PLACEMENT_3D ( 'NONE', #8955, #9307, #20549 ) ;
#34031 = VERTEX_POINT ( 'NONE', #25851 ) ;
#34032 = ORIENTED_EDGE ( 'NONE', *, *, #30016, .F. ) ;
#34033 = ORIENTED_EDGE ( 'NONE', *, *, #10024, .F. ) ;
#34034 = AXIS2_PLACEMENT_3D ( 'NONE', #35670, #21611, #7353 ) ;
#34035 = DIRECTION ( 'NONE',  ( -0.000000000000000000, -0.000000000000000000, -1.000000000000000000 ) ) ;
#34036 = DIRECTION ( 'NONE',  ( 0.000000000000000000, 0.000000000000000000, -1.000000000000000000 ) ) ;
#34037 = EDGE_LOOP ( 'NONE', ( #5544, #32881, #19112, #12029 ) ) ;
#34038 = AXIS2_PLACEMENT_3D ( 'NONE', #30986, #5115, #33799 ) ;
#34039 = CYLINDRICAL_SURFACE ( 'NONE', #26897, 2.000000000000001776 ) ;
#34040 = VERTEX_POINT ( 'NONE', #14968 ) ;
#34041 = EDGE_CURVE ( 'NONE', #9761, #32663, #14824, .T. ) ;
#34042 = CARTESIAN_POINT ( 'NONE',  ( 14.38872371163433428, -115.5691697732052177, 32.49999999999999289 ) ) ;
#34043 = ORIENTED_EDGE ( 'NONE', *, *, #32627, .T. ) ;
#34044 = DIRECTION ( 'NONE',  ( 0.000000000000000000, 0.000000000000000000, -1.000000000000000000 ) ) ;
#34045 = AXIS2_PLACEMENT_3D ( 'NONE', #30150, #10665, #15911 ) ;
#34046 = EDGE_LOOP ( 'NONE', ( #22797, #4141, #9754, #29852 ) ) ;
#34047 = DIRECTION ( 'NONE',  ( 0.000000000000000000, 0.000000000000000000, 1.000000000000000000 ) ) ;
#34048 = CARTESIAN_POINT ( 'NONE',  ( 5.000000000000000888, -2.886751345948134873, -2.080000000000000071 ) ) ;
#34049 = CIRCLE ( 'NONE', #23240, 2.000000000000001776 ) ;
#34050 = ORIENTED_EDGE ( 'NONE', *, *, #13268, .T. ) ;
#34051 = DIRECTION ( 'NONE',  ( 1.000000000000000000, 0.000000000000000000, 0.000000000000000000 ) ) ;
#34052 = AXIS2_PLACEMENT_3D ( 'NONE', #6734, #22832, #8756 ) ;
#34053 = CIRCLE ( 'NONE', #3507, 1.999999999999998224 ) ;
#34054 = CYLINDRICAL_SURFACE ( 'NONE', #2737, 2.000000000000001776 ) ;
#34055 = CARTESIAN_POINT ( 'NONE',  ( 0.000000000000000000, 0.000000000000000000, 0.000000000000000000 ) ) ;
#34056 = CIRCLE ( 'NONE', #18501, 2.000000000000001776 ) ;
#34057 = ORIENTED_EDGE ( 'NONE', *, *, #18175, .F. ) ;
#34058 = CARTESIAN_POINT ( 'NONE',  ( -75.00000337463099243, -25.98076211353322051, -9.999999999999998224 ) ) ;
#34059 = CARTESIAN_POINT ( 'NONE',  ( 72.72667006429115588, 101.6652913307178636, 32.50002500000000083 ) ) ;
#34060 = ORIENTED_EDGE ( 'NONE', *, *, #20287, .F. ) ;
#34061 = CARTESIAN_POINT ( 'NONE',  ( 23.49187040204899546, -103.5527524078059400, 32.50001250000000397 ) ) ;
#34062 = DIRECTION ( 'NONE',  ( -1.000000000000000000, 0.000000000000000000, -0.000000000000000000 ) ) ;
#34063 = DIRECTION ( 'NONE',  ( 0.000000000000000000, 0.000000000000000000, 1.000000000000000000 ) ) ;
#34064 = EDGE_CURVE ( 'NONE', #30348, #5113, #19015, .T. ) ;
#34065 = CIRCLE ( 'NONE', #30463, 2.000000000000001776 ) ;
#34066 = ADVANCED_FACE ( 'NONE', ( #11570 ), #8780, .F. ) ;
#34067 = DIRECTION ( 'NONE',  ( 0.000000000000000000, 0.000000000000000000, -1.000000000000000000 ) ) ;
#34068 = CIRCLE ( 'NONE', #13089, 2.000000000000001776 ) ;
#34069 = ORIENTED_EDGE ( 'NONE', *, *, #8740, .T. ) ;
#34070 = ORIENTED_EDGE ( 'NONE', *, *, #1988, .T. ) ;
#34071 = EDGE_CURVE ( 'NONE', #23292, #12699, #3459, .T. ) ;
#34072 = CARTESIAN_POINT ( 'NONE',  ( 3.500000000000000888, 55.00000000000000000, -15.00000000000000000 ) ) ;
#34073 = DIRECTION ( 'NONE',  ( 0.000000000000000000, 0.000000000000000000, 1.000000000000000000 ) ) ;
#34075 = ORIENTED_EDGE ( 'NONE', *, *, #5044, .T. ) ;
#34074 = ADVANCED_FACE ( 'NONE', ( #32914 ), #16227, .F. ) ;
#34076 = ORIENTED_EDGE ( 'NONE', *, *, #13882, .T. ) ;
#34077 = CIRCLE ( 'NONE', #13099, 2.000000000000001776 ) ;
#34078 = DIRECTION ( 'NONE',  ( 0.000000000000000000, 0.000000000000000000, -1.000000000000000000 ) ) ;
#34079 = CARTESIAN_POINT ( 'NONE',  ( -70.00000337463099243, 51.96152422706637708, -5.000000000000000000 ) ) ;
#34080 = VECTOR ( 'NONE', #4212, 1000.000000000000000 ) ;
#34081 = DIRECTION ( 'NONE',  ( 0.000000000000000000, 0.000000000000000000, 1.000000000000000000 ) ) ;
#34082 = EDGE_LOOP ( 'NONE', ( #29005, #18845, #20747, #3115, #27679, #11805 ) ) ;
#34083 = VERTEX_POINT ( 'NONE', #27645 ) ;
#34084 = CYLINDRICAL_SURFACE ( 'NONE', #3926, 2.000000000000001776 ) ;
#34085 = CARTESIAN_POINT ( 'NONE',  ( -35.00000337463116296, -60.62177826491080168, -9.999999999999998224 ) ) ;
#34086 = VERTEX_POINT ( 'NONE', #19045 ) ;
#34087 = AXIS2_PLACEMENT_3D ( 'NONE', #36828, #10949, #10787 ) ;
#34088 = EDGE_CURVE ( 'NONE', #8936, #7710, #4672, .T. ) ;
#34089 = DIRECTION ( 'NONE',  ( 0.000000000000000000, 0.000000000000000000, 1.000000000000000000 ) ) ;
#34090 = VERTEX_POINT ( 'NONE', #4409 ) ;
#34091 = FACE_BOUND ( 'NONE', #17080, .T. ) ;
#34092 = CIRCLE ( 'NONE', #35297, 2.000000000000001776 ) ;
#34093 = AXIS2_PLACEMENT_3D ( 'NONE', #1278, #5016, #16451 ) ;
#34094 = CARTESIAN_POINT ( 'NONE',  ( -5.000003374631269537, -77.94228634059960825, -9.999999999999998224 ) ) ;
#34095 = VECTOR ( 'NONE', #20166, 1000.000000000000000 ) ;
#34096 = ORIENTED_EDGE ( 'NONE', *, *, #3033, .T. ) ;
#34097 = CARTESIAN_POINT ( 'NONE',  ( -70.80619744049063513, -84.18124734178186941, 38.50000000000000711 ) ) ;
#34098 = CARTESIAN_POINT ( 'NONE',  ( -3.000003374631269981, -77.94228634059960825, -9.999999999999998224 ) ) ;
#34099 = AXIS2_PLACEMENT_3D ( 'NONE', #18557, #4473, #1108 ) ;
#34100 = DIRECTION ( 'NONE',  ( 0.8660254037844413721, 0.4999999999999950595, 0.000000000000000000 ) ) ;
#34101 = CARTESIAN_POINT ( 'NONE',  ( -75.00000337463097821, 25.98076211353318854, -5.000000000000000000 ) ) ;
#34102 = EDGE_CURVE ( 'NONE', #32493, #5473, #11809, .T. ) ;
#34103 = ORIENTED_EDGE ( 'NONE', *, *, #25651, .F. ) ;
#34104 = DIRECTION ( 'NONE',  ( 0.000000000000000000, 0.000000000000000000, 1.000000000000000000 ) ) ;
#34105 = VECTOR ( 'NONE', #30788, 1000.000000000000000 ) ;
#34106 = CYLINDRICAL_SURFACE ( 'NONE', #14261, 2.000000000000000000 ) ;
#34107 = DIRECTION ( 'NONE',  ( 0.000000000000000000, 0.000000000000000000, 1.000000000000000000 ) ) ;
#34108 = ORIENTED_EDGE ( 'NONE', *, *, #36428, .F. ) ;
#34109 = ORIENTED_EDGE ( 'NONE', *, *, #1709, .T. ) ;
#34110 = CIRCLE ( 'NONE', #31096, 3.499999999999996003 ) ;
#34111 = VERTEX_POINT ( 'NONE', #35728 ) ;
#34112 = EDGE_CURVE ( 'NONE', #5803, #1959, #10043, .T. ) ;
#34113 = DIRECTION ( 'NONE',  ( 0.000000000000000000, 0.000000000000000000, 1.000000000000000000 ) ) ;
#34114 = CARTESIAN_POINT ( 'NONE',  ( 3.499999999999991562, 55.00000000000000000, -10.00000000000000000 ) ) ;
#34115 = CIRCLE ( 'NONE', #37105, 2.000000000000001776 ) ;
#34116 = FACE_BOUND ( 'NONE', #35662, .T. ) ;
#34117 = AXIS2_PLACEMENT_3D ( 'NONE', #9851, #29726, #35563 ) ;
#34118 = EDGE_CURVE ( 'NONE', #34784, #17325, #18666, .T. ) ;
#34119 = CARTESIAN_POINT ( 'NONE',  ( -31.74999999999995737, 0.000000000000000000, 3.000000000000000888 ) ) ;
#34120 = CIRCLE ( 'NONE', #29305, 2.000000000000001776 ) ;
#34121 = CARTESIAN_POINT ( 'NONE',  ( 77.93337651276290501, -72.12094976675109592, 32.50001250000000397 ) ) ;
#34122 = CARTESIAN_POINT ( 'NONE',  ( -15.00000337463125710, -77.94228634059960825, -9.999999999999998224 ) ) ;
#34123 = CYLINDRICAL_SURFACE ( 'NONE', #26787, 150.0000000000000284 ) ;
#34124 = CARTESIAN_POINT ( 'NONE',  ( 108.3061974404898820, 19.22934205794938478, 32.50000000000000000 ) ) ;
#34125 = ORIENTED_EDGE ( 'NONE', *, *, #8493, .F. ) ;
#34126 = ORIENTED_EDGE ( 'NONE', *, *, #35419, .T. ) ;
#34127 = LINE ( 'NONE', #11575, #31998 ) ;
#34128 = AXIS2_PLACEMENT_3D ( 'NONE', #27294, #13055, #23757 ) ;
#34129 = CARTESIAN_POINT ( 'NONE',  ( -83.00000337463092137, 8.660254037844389075, 12.50000000000000000 ) ) ;
#34130 = DIRECTION ( 'NONE',  ( 0.000000000000000000, 0.000000000000000000, 1.000000000000000000 ) ) ;
#34131 = CARTESIAN_POINT ( 'NONE',  ( 4.279621169095998212, -62.97617850287780072, -4.999999999999997335 ) ) ;
#34132 = ORIENTED_EDGE ( 'NONE', *, *, #22748, .F. ) ;
#34133 = AXIS2_PLACEMENT_3D ( 'NONE', #8405, #23006, #5965 ) ;
#34134 = EDGE_CURVE ( 'NONE', #22352, #19159, #25629, .T. ) ;
#34135 = FACE_BOUND ( 'NONE', #840, .T. ) ;
#34136 = EDGE_LOOP ( 'NONE', ( #36385, #14073, #25291, #11423, #12018 ) ) ;
#34137 = ORIENTED_EDGE ( 'NONE', *, *, #7736, .T. ) ;
#34138 = CARTESIAN_POINT ( 'NONE',  ( 3.000000000000000000, 2.935248768560057453, -3.903127820947815962E-15 ) ) ;
#34139 = ORIENTED_EDGE ( 'NONE', *, *, #10867, .T. ) ;
#34140 = CIRCLE ( 'NONE', #5393, 6.000000000000005329 ) ;
#34141 = DIRECTION ( 'NONE',  ( 1.000000000000000000, 0.000000000000000000, 0.000000000000000000 ) ) ;
#34142 = ADVANCED_FACE ( 'NONE', ( #24665 ), #1589, .F. ) ;
#34143 = DIRECTION ( 'NONE',  ( 1.000000000000000000, 0.000000000000000000, 0.000000000000000000 ) ) ;
#34144 = CIRCLE ( 'NONE', #2934, 2.000000000000001776 ) ;
#34145 = DIRECTION ( 'NONE',  ( 1.000000000000000000, 0.000000000000000000, 0.000000000000000000 ) ) ;
#34146 = ADVANCED_FACE ( 'NONE', ( #33478 ), #27409, .F. ) ;
#34147 = CIRCLE ( 'NONE', #23354, 2.000000000000001776 ) ;
#34148 = EDGE_LOOP ( 'NONE', ( #18392, #25428, #4302, #25946, #6095, #12110, #12013, #13305, #30941 ) ) ;
#34149 = EDGE_LOOP ( 'NONE', ( #6998, #243, #16818 ) ) ;
#34150 = AXIS2_PLACEMENT_3D ( 'NONE', #19709, #30943, #36763 ) ;
#34151 = VERTEX_POINT ( 'NONE', #21477 ) ;
#34152 = VERTEX_POINT ( 'NONE', #15666 ) ;
#34153 = ORIENTED_EDGE ( 'NONE', *, *, #3172, .F. ) ;
#34154 = CARTESIAN_POINT ( 'NONE',  ( 44.99999662536849598, -77.94228634059960825, -5.000000000000000000 ) ) ;
#34155 = AXIS2_PLACEMENT_3D ( 'NONE', #8972, #35231, #6146 ) ;
#34156 = PRESENTATION_STYLE_ASSIGNMENT (( #11602 ) ) ;
#34157 = CIRCLE ( 'NONE', #9344, 2.000000000000001776 ) ;
#34158 = CARTESIAN_POINT ( 'NONE',  ( 0.000000000000000000, 0.000000000000000000, -5.000000000000000000 ) ) ;
#34159 = CARTESIAN_POINT ( 'NONE',  ( -55.00000337463109901, -60.62177826491083010, -5.000000000000000000 ) ) ;
#34160 = CARTESIAN_POINT ( 'NONE',  ( 90.60231327712337190, 15.97563234535636134, -49.86561046011506448 ) ) ;
#34161 = ORIENTED_EDGE ( 'NONE', *, *, #17999, .T. ) ;
#34162 = CARTESIAN_POINT ( 'NONE',  ( 7.999996625368618552, 69.28203230275516944, -9.999999999999998224 ) ) ;
#34163 = LINE ( 'NONE', #28315, #33584 ) ;
#34164 = ADVANCED_FACE ( 'NONE', ( #21658 ), #4794, .F. ) ;
#34165 = CARTESIAN_POINT ( 'NONE',  ( 0.000000000000000000, 0.000000000000000000, 0.000000000000000000 ) ) ;
#34166 = VERTEX_POINT ( 'NONE', #13027 ) ;
#34167 = CIRCLE ( 'NONE', #25785, 2.000000000000000000 ) ;
#34168 = DIRECTION ( 'NONE',  ( 0.000000000000000000, 0.000000000000000000, 1.000000000000000000 ) ) ;
#34169 = DIRECTION ( 'NONE',  ( 0.000000000000000000, -0.000000000000000000, 1.000000000000000000 ) ) ;
#34170 = EDGE_LOOP ( 'NONE', ( #18449, #1171, #21656, #5527 ) ) ;
#34171 = ORIENTED_EDGE ( 'NONE', *, *, #36839, .F. ) ;
#34172 = CARTESIAN_POINT ( 'NONE',  ( -70.00000337463099243, -2.428612866367529932E-14, -9.999999999999998224 ) ) ;
#34173 = CARTESIAN_POINT ( 'NONE',  ( 82.99999662536832545, 8.660254037844394404, 12.50000000000000000 ) ) ;
#34174 = AXIS2_PLACEMENT_3D ( 'NONE', #24786, #36219, #33603 ) ;
#34175 = CARTESIAN_POINT ( 'NONE',  ( 61.99999662536845335, 34.64101615137759893, 17.49999999999999645 ) ) ;
#34176 = CARTESIAN_POINT ( 'NONE',  ( -3.374631334790434423E-06, 69.28203230275516944, -9.999999999999998224 ) ) ;
#34177 = ORIENTED_EDGE ( 'NONE', *, *, #6127, .T. ) ;
#34178 = ORIENTED_EDGE ( 'NONE', *, *, #16633, .T. ) ;
#34179 = DIRECTION ( 'NONE',  ( -1.000000000000000000, 0.000000000000000000, 0.000000000000000000 ) ) ;
#34180 = CARTESIAN_POINT ( 'NONE',  ( 0.000000000000000000, 0.000000000000000000, 32.50000000000000000 ) ) ;
#34181 = ADVANCED_FACE ( 'NONE', ( #27469 ), #27087, .F. ) ;
#34182 = VERTEX_POINT ( 'NONE', #10589 ) ;
#34183 = EDGE_CURVE ( 'NONE', #30962, #4217, #32092, .T. ) ;
#34184 = LINE ( 'NONE', #19739, #21987 ) ;
#34185 = VERTEX_POINT ( 'NONE', #35546 ) ;
#34186 = VERTEX_POINT ( 'NONE', #21832 ) ;
#34187 = ADVANCED_FACE ( 'NONE', ( #24484 ), #33275, .F. ) ;
#34188 = DIRECTION ( 'NONE',  ( 1.000000000000000000, 0.000000000000000000, 0.000000000000000000 ) ) ;
#34189 = CYLINDRICAL_SURFACE ( 'NONE', #34038, 2.000000000000001776 ) ;
#34190 = CARTESIAN_POINT ( 'NONE',  ( 51.99999662536847467, 69.28203230275516944, -5.000000000000000000 ) ) ;
#34191 = VERTEX_POINT ( 'NONE', #21274 ) ;
#34192 = ORIENTED_EDGE ( 'NONE', *, *, #1103, .F. ) ;
#34193 = EDGE_CURVE ( 'NONE', #27668, #35643, #19542, .T. ) ;
#34194 = DIRECTION ( 'NONE',  ( 0.000000000000000000, 0.000000000000000000, 1.000000000000000000 ) ) ;
#34195 = DIRECTION ( 'NONE',  ( 0.000000000000000000, 0.000000000000000000, 1.000000000000000000 ) ) ;
#34196 = EDGE_CURVE ( 'NONE', #29936, #21303, #24958, .T. ) ;
#34197 = CARTESIAN_POINT ( 'NONE',  ( -45.00000337463111322, 60.62177826491077326, 17.49999999999999645 ) ) ;
#34198 = LINE ( 'NONE', #34010, #35273 ) ;
#34199 = ORIENTED_EDGE ( 'NONE', *, *, #34845, .T. ) ;
#34200 = CARTESIAN_POINT ( 'NONE',  ( -65.00000337463104927, -43.30127018922202353, -9.999999999999998224 ) ) ;
#34201 = AXIS2_PLACEMENT_3D ( 'NONE', #17570, #25845, #29197 ) ;
#34202 = FACE_BOUND ( 'NONE', #33586, .T. ) ;
#34203 = DIRECTION ( 'NONE',  ( 1.000000000000000000, 0.000000000000000000, 0.000000000000000000 ) ) ;
#34204 = DIRECTION ( 'NONE',  ( 0.000000000000000000, 0.000000000000000000, 1.000000000000000000 ) ) ;
#34205 = CARTESIAN_POINT ( 'NONE',  ( -67.30619744049063513, -84.18124734178186941, 32.50000000000000000 ) ) ;
#34206 = EDGE_CURVE ( 'NONE', #10748, #3694, #29100, .T. ) ;
#34207 = DIRECTION ( 'NONE',  ( 0.000000000000000000, 0.000000000000000000, -1.000000000000000000 ) ) ;
#34208 = ADVANCED_FACE ( 'NONE', ( #33831 ), #8346, .F. ) ;
#34209 = CARTESIAN_POINT ( 'NONE',  ( 16.42335937861835049, 114.0197453844396591, 27.49998800000000898 ) ) ;
#34210 = EDGE_CURVE ( 'NONE', #32620, #9158, #21947, .T. ) ;
#34211 = EDGE_CURVE ( 'NONE', #21629, #28577, #25536, .T. ) ;
#34212 = DIRECTION ( 'NONE',  ( 0.000000000000000000, 0.000000000000000000, -1.000000000000000000 ) ) ;
#34213 = ORIENTED_EDGE ( 'NONE', *, *, #29868, .T. ) ;
#34214 = EDGE_CURVE ( 'NONE', #26470, #6533, #5782, .T. ) ;
#34215 = CARTESIAN_POINT ( 'NONE',  ( 0.000000000000000000, 0.000000000000000000, -5.132899837730832360 ) ) ;
#34216 = LINE ( 'NONE', #19774, #6955 ) ;
#34217 = DIRECTION ( 'NONE',  ( 1.000000000000000000, 0.000000000000000000, 0.000000000000000000 ) ) ;
#34218 = EDGE_LOOP ( 'NONE', ( #20863, #23817, #9183, #3245 ) ) ;
#34219 = EDGE_LOOP ( 'NONE', ( #35260, #15400, #24804, #36132 ) ) ;
#34220 = ORIENTED_EDGE ( 'NONE', *, *, #21954, .F. ) ;
#34221 = CARTESIAN_POINT ( 'NONE',  ( -87.00000337463093558, 25.98076211353317433, 12.50000000000000000 ) ) ;
#34222 = CARTESIAN_POINT ( 'NONE',  ( -47.63139720814380951, 27.50000000000055422, -5.000000000000000000 ) ) ;
#34223 = DIRECTION ( 'NONE',  ( 0.000000000000000000, 0.000000000000000000, 1.000000000000000000 ) ) ;
#34224 = ORIENTED_EDGE ( 'NONE', *, *, #16828, .F. ) ;
#34225 = DIRECTION ( 'NONE',  ( 1.000000000000000000, 0.000000000000000000, 0.000000000000000000 ) ) ;
#34226 = EDGE_LOOP ( 'NONE', ( #14726, #19404, #31409, #5264 ) ) ;
#34227 = CARTESIAN_POINT ( 'NONE',  ( 22.49971464476085359, -105.9191578779291802, 32.49999999999999289 ) ) ;
#34228 = ORIENTED_EDGE ( 'NONE', *, *, #15694, .F. ) ;
#34229 = FACE_OUTER_BOUND ( 'NONE', #1004, .T. ) ;
#34230 = ORIENTED_EDGE ( 'NONE', *, *, #16868, .F. ) ;
#34231 = ORIENTED_EDGE ( 'NONE', *, *, #9519, .T. ) ;
#34232 = CARTESIAN_POINT ( 'NONE',  ( -124.4080600076929954, 12.15049814296761888, 32.50000000000000000 ) ) ;
#34233 = DIRECTION ( 'NONE',  ( 0.000000000000000000, 0.000000000000000000, 1.000000000000000000 ) ) ;
#34234 = ORIENTED_EDGE ( 'NONE', *, *, #31934, .T. ) ;
#34235 = DIRECTION ( 'NONE',  ( -1.000000000000000000, -0.000000000000000000, -0.000000000000000000 ) ) ;
#34236 = CONTEXT_DEPENDENT_SHAPE_REPRESENTATION ( #25958, #32855 ) ;
#34237 = DIRECTION ( 'NONE',  ( 0.000000000000000000, 0.000000000000000000, 1.000000000000000000 ) ) ;
#34238 = DIRECTION ( 'NONE',  ( 0.000000000000000000, -0.000000000000000000, -1.000000000000000000 ) ) ;
#34239 = VERTEX_POINT ( 'NONE', #30813 ) ;
#34240 = DIRECTION ( 'NONE',  ( 0.000000000000000000, 0.000000000000000000, 1.000000000000000000 ) ) ;
#34241 = DIRECTION ( 'NONE',  ( 1.000000000000000000, 0.000000000000000000, 0.000000000000000000 ) ) ;
#34242 = CIRCLE ( 'NONE', #18050, 2.000000000000001776 ) ;
#34243 = ORIENTED_EDGE ( 'NONE', *, *, #12131, .F. ) ;
#34244 = DIRECTION ( 'NONE',  ( 0.000000000000000000, 0.000000000000000000, 1.000000000000000000 ) ) ;
#34245 = AXIS2_PLACEMENT_3D ( 'NONE', #9381, #20820, #32254 ) ;
#34246 = DIRECTION ( 'NONE',  ( 0.000000000000000000, 0.000000000000000000, 1.000000000000000000 ) ) ;
#34247 = CARTESIAN_POINT ( 'NONE',  ( -5.248984340851196251, -2.531668808681923899, -4.266868479993930485 ) ) ;
#34248 = CYLINDRICAL_SURFACE ( 'NONE', #33833, 2.000000000000001776 ) ;
#34249 = B_SPLINE_CURVE_WITH_KNOTS ( 'NONE', 3,
 ( #34372, #17124, #25571, #6060, #2888 ),
 .UNSPECIFIED., .F., .F.,
 ( 4, 1, 4 ),
 ( 0.000000000000000000, 0.002886751345948135490, 0.005773502691896270980 ),
 .UNSPECIFIED. ) ;
#34250 = VERTEX_POINT ( 'NONE', #8145 ) ;
#34251 = EDGE_CURVE ( 'NONE', #18020, #26782, #23745, .T. ) ;
#34252 = ORIENTED_EDGE ( 'NONE', *, *, #23889, .T. ) ;
#34253 = DIRECTION ( 'NONE',  ( 1.000000000000000000, 0.000000000000000000, 0.000000000000000000 ) ) ;
#34254 = CARTESIAN_POINT ( 'NONE',  ( 42.99999662536848888, -77.94228634059960825, -9.999999999999998224 ) ) ;
#34255 = EDGE_LOOP ( 'NONE', ( #34260, #1657 ) ) ;
#34256 = ORIENTED_EDGE ( 'NONE', *, *, #3879, .T. ) ;
#34257 = CARTESIAN_POINT ( 'NONE',  ( 56.99999662536846046, -43.30127018922200222, 17.49999999999999645 ) ) ;
#34258 = DIRECTION ( 'NONE',  ( 1.000000000000000000, 0.000000000000000000, 0.000000000000000000 ) ) ;
#34259 = DIRECTION ( 'NONE',  ( 0.000000000000000000, 0.000000000000000000, 1.000000000000000000 ) ) ;
#34260 = ORIENTED_EDGE ( 'NONE', *, *, #26982, .F. ) ;
#34261 = ORIENTED_EDGE ( 'NONE', *, *, #19810, .F. ) ;
#34262 = CARTESIAN_POINT ( 'NONE',  ( -104.8061974404896262, 19.22934205795090534, 32.50000000000000000 ) ) ;
#34263 = VERTEX_POINT ( 'NONE', #31368 ) ;
#34264 = CARTESIAN_POINT ( 'NONE',  ( -28.00000337463118427, 69.28203230275516944, -9.999999999999998224 ) ) ;
#34265 = ORIENTED_EDGE ( 'NONE', *, *, #1403, .F. ) ;
#34266 = FACE_BOUND ( 'NONE', #6584, .T. ) ;
#34267 = ADVANCED_FACE ( 'NONE', ( #19781 ), #28022, .T. ) ;
#34268 = DIRECTION ( 'NONE',  ( -1.000000000000000000, 0.000000000000000000, 0.000000000000000000 ) ) ;
#34269 = FACE_BOUND ( 'NONE', #18209, .T. ) ;
#34270 = ORIENTED_EDGE ( 'NONE', *, *, #170, .T. ) ;
#34271 = DIRECTION ( 'NONE',  ( -0.9963767006942637616, -0.08504981077941027590, 0.000000000000000000 ) ) ;
#34272 = CARTESIAN_POINT ( 'NONE',  ( -15.00000337463126066, 77.94228634059957983, -9.999999999999998224 ) ) ;
#34273 = CARTESIAN_POINT ( 'NONE',  ( -58.88972745734203329, -33.99999999999965894, 12.49999999999999822 ) ) ;
#34274 = PLANE ( 'NONE',  #2352 ) ;
#34275 = ORIENTED_EDGE ( 'NONE', *, *, #11473, .T. ) ;
#34276 = DIRECTION ( 'NONE',  ( 1.000000000000000000, 0.000000000000000000, 0.000000000000000000 ) ) ;
#34277 = PLANE ( 'NONE',  #16647 ) ;
#34278 = DIRECTION ( 'NONE',  ( 0.000000000000000000, 0.000000000000000000, 1.000000000000000000 ) ) ;
#34279 = ORIENTED_EDGE ( 'NONE', *, *, #21261, .T. ) ;
#34280 = VERTEX_POINT ( 'NONE', #25224 ) ;
#34281 = AXIS2_PLACEMENT_3D ( 'NONE', #21208, #30025, #24780 ) ;
#34282 = EDGE_CURVE ( 'NONE', #8433, #6013, #13944, .T. ) ;
#34283 = ORIENTED_EDGE ( 'NONE', *, *, #30250, .F. ) ;
#34284 = CARTESIAN_POINT ( 'NONE',  ( 39.99999662536853151, 69.28203230275518365, -9.999999999999998224 ) ) ;
#34285 = DIRECTION ( 'NONE',  ( 0.000000000000000000, 0.000000000000000000, -1.000000000000000000 ) ) ;
#34286 = CARTESIAN_POINT ( 'NONE',  ( -47.63139720814380951, 27.50000000000055422, -10.00000000000000000 ) ) ;
#34287 = DIRECTION ( 'NONE',  ( 1.000000000000000000, 0.000000000000000000, 0.000000000000000000 ) ) ;
#34288 = CARTESIAN_POINT ( 'NONE',  ( -60.00000337463104216, 34.64101615137757051, -9.999999999999998224 ) ) ;
#34289 = DIRECTION ( 'NONE',  ( -1.000000000000000000, 0.000000000000000000, 0.000000000000000000 ) ) ;
#34290 = ORIENTED_EDGE ( 'NONE', *, *, #35574, .T. ) ;
#34291 = ORIENTED_EDGE ( 'NONE', *, *, #8918, .F. ) ;
#34292 = AXIS2_PLACEMENT_3D ( 'NONE', #10353, #26873, #13172 ) ;
#34293 = DIRECTION ( 'NONE',  ( 0.000000000000000000, 1.000000000000000000, -1.625241993126352989E-15 ) ) ;
#34294 = EDGE_CURVE ( 'NONE', #23016, #603, #17734, .T. ) ;
#34295 = CARTESIAN_POINT ( 'NONE',  ( 5.000000000000002665, -2.886751345948134873, -5.553418012614792509 ) ) ;
#34296 = DIRECTION ( 'NONE',  ( -1.000000000000000000, 0.000000000000000000, 0.000000000000000000 ) ) ;
#34297 = DIRECTION ( 'NONE',  ( 0.000000000000000000, 0.000000000000000000, 1.000000000000000000 ) ) ;
#34298 = ORIENTED_EDGE ( 'NONE', *, *, #15246, .T. ) ;
#34299 = UNCERTAINTY_MEASURE_WITH_UNIT (LENGTH_MEASURE( 1.000000000000000082E-05 ), #8062, 'distance_accuracy_value', 'NONE');
#34300 = EDGE_CURVE ( 'NONE', #25896, #12555, #14239, .T. ) ;
#34301 = FACE_BOUND ( 'NONE', #6496, .T. ) ;
#34302 = VERTEX_POINT ( 'NONE', #36474 ) ;
#34303 = CIRCLE ( 'NONE', #7350, 150.0000000000000284 ) ;
#34304 = EDGE_LOOP ( 'NONE', ( #27673, #317 ) ) ;
#34305 = CIRCLE ( 'NONE', #13334, 2.000000000000001776 ) ;
#34306 = EDGE_CURVE ( 'NONE', #33312, #10163, #1572, .T. ) ;
#34307 = CARTESIAN_POINT ( 'NONE',  ( 0.4079457818577056916, -5.537975084925947478, -5.689399939901065295 ) ) ;
#34308 = VERTEX_POINT ( 'NONE', #8686 ) ;
#34309 = FACE_OUTER_BOUND ( 'NONE', #17694, .T. ) ;
#34310 = FACE_OUTER_BOUND ( 'NONE', #20890, .T. ) ;
#34311 = EDGE_CURVE ( 'NONE', #393, #27431, #25392, .T. ) ;
#34312 = DIRECTION ( 'NONE',  ( 0.000000000000000000, 0.000000000000000000, -1.000000000000000000 ) ) ;
#34313 = EDGE_LOOP ( 'NONE', ( #12859, #1398, #29172, #17431 ) ) ;
#34314 = EDGE_LOOP ( 'NONE', ( #3838, #19661, #33617, #5282, #26044 ) ) ;
#34315 = VERTEX_POINT ( 'NONE', #34221 ) ;
#34316 = ORIENTED_EDGE ( 'NONE', *, *, #7815, .T. ) ;
#34317 = AXIS2_PLACEMENT_3D ( 'NONE', #34338, #26443, #189 ) ;
#34318 = ORIENTED_EDGE ( 'NONE', *, *, #494, .F. ) ;
#34319 = DIRECTION ( 'NONE',  ( 1.000000000000000000, 0.000000000000000000, 0.000000000000000000 ) ) ;
#34320 = DIRECTION ( 'NONE',  ( 1.000000000000000000, 0.000000000000000000, 0.000000000000000000 ) ) ;
#34321 = DIRECTION ( 'NONE',  ( -1.000000000000000000, 0.000000000000000000, 0.000000000000000000 ) ) ;
#34322 = DIRECTION ( 'NONE',  ( -0.000000000000000000, -0.000000000000000000, -1.000000000000000000 ) ) ;
#34323 = CARTESIAN_POINT ( 'NONE',  ( -80.00000337463094979, 17.32050807568878525, 12.50000000000000000 ) ) ;
#34324 = ORIENTED_EDGE ( 'NONE', *, *, #32367, .T. ) ;
#34325 = FACE_OUTER_BOUND ( 'NONE', #5662, .T. ) ;
#34326 = ADVANCED_FACE ( 'NONE', ( #11130 ), #5519, .F. ) ;
#34327 = CARTESIAN_POINT ( 'NONE',  ( -5.253368672218638125, -3.033033817057809500, -4.359491423763659945 ) ) ;
#34328 = VECTOR ( 'NONE', #23364, 1000.000000000000000 ) ;
#34329 = CARTESIAN_POINT ( 'NONE',  ( -75.00000337463099243, -25.98076211353322051, 12.50000000000000000 ) ) ;
#34330 = VERTEX_POINT ( 'NONE', #22216 ) ;
#34331 = DIRECTION ( 'NONE',  ( 0.000000000000000000, -0.4999999999999996114, 0.8660254037844388186 ) ) ;
#34332 = DIRECTION ( 'NONE',  ( 1.000000000000000000, 0.000000000000000000, 0.000000000000000000 ) ) ;
#34333 = ORIENTED_EDGE ( 'NONE', *, *, #19094, .T. ) ;
#34334 = EDGE_CURVE ( 'NONE', #18549, #34302, #28564, .T. ) ;
#34335 = EDGE_LOOP ( 'NONE', ( #11295, #2197, #21126 ) ) ;
#34336 = DIRECTION ( 'NONE',  ( 0.000000000000000000, 0.000000000000000000, 1.000000000000000000 ) ) ;
#34337 = EDGE_CURVE ( 'NONE', #6568, #25502, #35122, .T. ) ;
#34338 = CARTESIAN_POINT ( 'NONE',  ( -62.97617850287781494, -4.279621169095772615, -4.999999999999997335 ) ) ;
#34339 = CARTESIAN_POINT ( 'NONE',  ( -77.00000337463097821, 8.660254037844374864, 12.50000000000000000 ) ) ;
#34340 = DIRECTION ( 'NONE',  ( 1.000000000000000000, 0.000000000000000000, 0.000000000000000000 ) ) ;
#34341 = ORIENTED_EDGE ( 'NONE', *, *, #11427, .T. ) ;
#34342 = EDGE_LOOP ( 'NONE', ( #17326, #20080, #7665, #5612 ) ) ;
#34343 = CIRCLE ( 'NONE', #19355, 2.000000000000001776 ) ;
#34344 = DIRECTION ( 'NONE',  ( -0.000000000000000000, -0.000000000000000000, 1.000000000000000000 ) ) ;
#34345 = CARTESIAN_POINT ( 'NONE',  ( 66.99999662536839651, -43.30127018922199511, -9.999999999999998224 ) ) ;
#34346 = CARTESIAN_POINT ( 'NONE',  ( 5.000000000000002665, -2.886751345948134873, -5.553418012614792509 ) ) ;
#34347 = AXIS2_PLACEMENT_3D ( 'NONE', #6889, #26962, #10269 ) ;
#34348 = ORIENTED_EDGE ( 'NONE', *, *, #23854, .T. ) ;
#34349 = CYLINDRICAL_SURFACE ( 'NONE', #32136, 2.000000000000001776 ) ;
#34350 = ORIENTED_EDGE ( 'NONE', *, *, #18731, .T. ) ;
#34351 = ORIENTED_EDGE ( 'NONE', *, *, #17756, .F. ) ;
#34352 = CIRCLE ( 'NONE', #31936, 2.000000000000001776 ) ;
#34353 = CARTESIAN_POINT ( 'NONE',  ( 84.99999662536832545, 8.660254037844394404, 12.50000000000000000 ) ) ;
#34354 = EDGE_CURVE ( 'NONE', #31383, #31631, #33325, .T. ) ;
#34355 = AXIS2_PLACEMENT_3D ( 'NONE', #28908, #31545, #22934 ) ;
#34356 = DIRECTION ( 'NONE',  ( 0.000000000000000000, 0.000000000000000000, 1.000000000000000000 ) ) ;
#34357 = ORIENTED_EDGE ( 'NONE', *, *, #18505, .F. ) ;
#34358 = EDGE_LOOP ( 'NONE', ( #17113, #28560, #17405, #11278 ) ) ;
#34359 = CARTESIAN_POINT ( 'NONE',  ( 77.99999662536833966, 17.32050807568879236, 12.50000000000000000 ) ) ;
#34360 = VECTOR ( 'NONE', #4033, 1000.000000000000000 ) ;
#34361 = DIRECTION ( 'NONE',  ( 0.000000000000000000, 0.000000000000000000, 1.000000000000000000 ) ) ;
#34362 = DIRECTION ( 'NONE',  ( -1.000000000000000000, 0.000000000000000000, 0.000000000000000000 ) ) ;
#34363 = ORIENTED_EDGE ( 'NONE', *, *, #21996, .T. ) ;
#34364 = CARTESIAN_POINT ( 'NONE',  ( 69.99999662536839651, -17.32050807568879947, 17.49999999999999645 ) ) ;
#34365 = FACE_BOUND ( 'NONE', #34945, .T. ) ;
#34366 = CARTESIAN_POINT ( 'NONE',  ( -87.00000337463093558, 8.660254037844389075, 17.49999999999999645 ) ) ;
#34367 = DIRECTION ( 'NONE',  ( 1.000000000000000000, 0.000000000000000000, 0.000000000000000000 ) ) ;
#34368 = CARTESIAN_POINT ( 'NONE',  ( -18.00000337463123756, -69.28203230275522628, -5.000000000000000000 ) ) ;
#34369 = CARTESIAN_POINT ( 'NONE',  ( -82.00000337463094979, -2.404119930384582903E-14, -9.999999999999998224 ) ) ;
#34370 = CIRCLE ( 'NONE', #10406, 2.000000000000001776 ) ;
#34371 = ADVANCED_FACE ( 'NONE', ( #11668 ), #29303, .F. ) ;
#34372 = CARTESIAN_POINT ( 'NONE',  ( 4.999999999999999112, -2.886751345948144198, -3.984345921091770659 ) ) ;
#34373 = ORIENTED_EDGE ( 'NONE', *, *, #36493, .T. ) ;
#34374 = EDGE_CURVE ( 'NONE', #8594, #3287, #3361, .T. ) ;
#34375 = DIRECTION ( 'NONE',  ( 0.000000000000000000, 0.000000000000000000, 1.000000000000000000 ) ) ;
#34376 = CARTESIAN_POINT ( 'NONE',  ( 3.000000000000000888, 3.673940397442060854E-16, -5.674599999999998090 ) ) ;
#34377 = DIRECTION ( 'NONE',  ( 0.000000000000000000, 0.000000000000000000, 1.000000000000000000 ) ) ;
#34378 = VECTOR ( 'NONE', #35092, 1000.000000000000000 ) ;
#34379 = ORIENTED_EDGE ( 'NONE', *, *, #31242, .T. ) ;
#34380 = EDGE_CURVE ( 'NONE', #25160, #18782, #36329, .T. ) ;
#34381 = ORIENTED_EDGE ( 'NONE', *, *, #13014, .T. ) ;
#34382 = EDGE_LOOP ( 'NONE', ( #23982, #1837, #28637, #15069, #9251 ) ) ;
#34383 = AXIS2_PLACEMENT_3D ( 'NONE', #22719, #20066, #9011 ) ;
#34384 = DIRECTION ( 'NONE',  ( 0.000000000000000000, 0.000000000000000000, -1.000000000000000000 ) ) ;
#34385 = CARTESIAN_POINT ( 'NONE',  ( 74.99999662536835388, -25.98076211353319565, -9.999999999999998224 ) ) ;
#34386 = EDGE_CURVE ( 'NONE', #34851, #18020, #9435, .T. ) ;
#34387 = FACE_OUTER_BOUND ( 'NONE', #9113, .T. ) ;
#34388 = ORIENTED_EDGE ( 'NONE', *, *, #37064, .T. ) ;
#34389 = EDGE_CURVE ( 'NONE', #30855, #15669, #22533, .T. ) ;
#34390 = DIRECTION ( 'NONE',  ( 1.000000000000000000, 0.000000000000000000, 0.000000000000000000 ) ) ;
#34391 = EDGE_LOOP ( 'NONE', ( #10588, #7885, #13460, #18629, #34730 ) ) ;
#34392 = DIRECTION ( 'NONE',  ( 1.000000000000000000, 0.000000000000000000, 0.000000000000000000 ) ) ;
#34393 = ORIENTED_EDGE ( 'NONE', *, *, #32489, .T. ) ;
#34394 = DIRECTION ( 'NONE',  ( -1.000000000000000000, 0.000000000000000000, 0.000000000000000000 ) ) ;
#34395 = VERTEX_POINT ( 'NONE', #35328 ) ;
#34396 = EDGE_CURVE ( 'NONE', #26676, #13541, #34767, .T. ) ;
#34397 = EDGE_LOOP ( 'NONE', ( #7516, #29811 ) ) ;
#34398 = EDGE_CURVE ( 'NONE', #24664, #21710, #6788, .T. ) ;
#34399 = VECTOR ( 'NONE', #30771, 1000.000000000000000 ) ;
#34400 = DIRECTION ( 'NONE',  ( 0.000000000000000000, 0.000000000000000000, 1.000000000000000000 ) ) ;
#34401 = DIRECTION ( 'NONE',  ( 0.000000000000000000, 0.000000000000000000, -1.000000000000000000 ) ) ;
#34402 = EDGE_CURVE ( 'NONE', #406, #24516, #12036, .T. ) ;
#34403 = DIRECTION ( 'NONE',  ( 1.000000000000000000, 0.000000000000000000, 0.000000000000000000 ) ) ;
#34404 = ORIENTED_EDGE ( 'NONE', *, *, #31574, .F. ) ;
#34405 = DIRECTION ( 'NONE',  ( 1.000000000000000000, 0.000000000000000000, 0.000000000000000000 ) ) ;
#34406 = AXIS2_PLACEMENT_3D ( 'NONE', #23239, #3727, #34692 ) ;
#34407 = DIRECTION ( 'NONE',  ( 0.000000000000000000, 0.000000000000000000, 1.000000000000000000 ) ) ;
#34408 = CARTESIAN_POINT ( 'NONE',  ( -3.374631289687624047E-06, -69.28203230275519786, -9.999999999999998224 ) ) ;
#34409 = ORIENTED_EDGE ( 'NONE', *, *, #35963, .F. ) ;
#34410 = CIRCLE ( 'NONE', #9826, 2.000000000000001776 ) ;
#34411 = DIRECTION ( 'NONE',  ( -1.000000000000000000, -0.000000000000000000, -0.000000000000000000 ) ) ;
#34412 = DIRECTION ( 'NONE',  ( 0.000000000000000000, 0.000000000000000000, -1.000000000000000000 ) ) ;
#34413 = VERTEX_POINT ( 'NONE', #17493 ) ;
#34414 = DIRECTION ( 'NONE',  ( -0.000000000000000000, -0.000000000000000000, -1.000000000000000000 ) ) ;
#34415 = CARTESIAN_POINT ( 'NONE',  ( -12.00000337463128197, 86.60254037844397601, -9.999999999999998224 ) ) ;
#34416 = DIRECTION ( 'NONE',  ( 0.000000000000000000, 0.000000000000000000, 1.000000000000000000 ) ) ;
#34417 = CARTESIAN_POINT ( 'NONE',  ( 81.99999662536833966, -3.469446951953614189E-15, -5.000000000000000000 ) ) ;
#34418 = EDGE_CURVE ( 'NONE', #7729, #21619, #34580, .T. ) ;
#34419 = CIRCLE ( 'NONE', #3948, 25.00000000000000000 ) ;
#34420 = ORIENTED_EDGE ( 'NONE', *, *, #2539, .F. ) ;
#34421 = ADVANCED_FACE ( 'NONE', ( #23322 ), #20666, .F. ) ;
#34422 = CIRCLE ( 'NONE', #28985, 2.000000000000001776 ) ;
#34423 = DIRECTION ( 'NONE',  ( 1.000000000000000000, 0.000000000000000000, 0.000000000000000000 ) ) ;
#34424 = DIRECTION ( 'NONE',  ( -1.000000000000000000, 0.000000000000000000, 0.000000000000000000 ) ) ;
#34425 = ORIENTED_EDGE ( 'NONE', *, *, #28455, .F. ) ;
#34426 = VECTOR ( 'NONE', #13301, 1000.000000000000000 ) ;
#34427 = ORIENTED_EDGE ( 'NONE', *, *, #24459, .F. ) ;
#34428 = ORIENTED_EDGE ( 'NONE', *, *, #8215, .T. ) ;
#34429 = CARTESIAN_POINT ( 'NONE',  ( 49.99999662536846756, -69.28203230275519786, -9.999999999999998224 ) ) ;
#34430 = DIRECTION ( 'NONE',  ( 1.000000000000000000, 0.000000000000000000, 0.000000000000000000 ) ) ;
#34431 = EDGE_CURVE ( 'NONE', #4753, #31059, #10329, .T. ) ;
#34432 = CARTESIAN_POINT ( 'NONE',  ( -2.503857664561936813E-16, -5.773502691896267081, -6.000000000000000000 ) ) ;
#34433 = CIRCLE ( 'NONE', #10495, 2.000000000000001776 ) ;
#34434 = AXIS2_PLACEMENT_3D ( 'NONE', #32679, #36069, #12790 ) ;
#34435 = EDGE_LOOP ( 'NONE', ( #1914, #4378 ) ) ;
#34436 = CIRCLE ( 'NONE', #23044, 33.00000000000001421 ) ;
#34437 = DIRECTION ( 'NONE',  ( 0.000000000000000000, 0.000000000000000000, 1.000000000000000000 ) ) ;
#34438 = ORIENTED_EDGE ( 'NONE', *, *, #15087, .F. ) ;
#34439 = FACE_OUTER_BOUND ( 'NONE', #18916, .T. ) ;
#34440 = EDGE_LOOP ( 'NONE', ( #29500, #28955, #15695, #21123 ) ) ;
#34441 = DIRECTION ( 'NONE',  ( 0.000000000000000000, 0.000000000000000000, -1.000000000000000000 ) ) ;
#34442 = EDGE_CURVE ( 'NONE', #17803, #31097, #7928, .T. ) ;
#34443 = SHAPE_REPRESENTATION ( 'torque nut 04-2_iso_ISO 7043-M6-N', ( #21385 ), #11148 ) ;
#34444 = EDGE_CURVE ( 'NONE', #13283, #22239, #14510, .T. ) ;
#34445 = CARTESIAN_POINT ( 'NONE',  ( -43.00000337463111322, -77.94228634059960825, 12.50000000000000000 ) ) ;
#34446 = EDGE_CURVE ( 'NONE', #21906, #30228, #35480, .T. ) ;
#34447 = EDGE_CURVE ( 'NONE', #33059, #14671, #19039, .T. ) ;
#34448 = FACE_BOUND ( 'NONE', #11588, .T. ) ;
#34449 = AXIS2_PLACEMENT_3D ( 'NONE', #36857, #20165, #31592 ) ;
#34450 = DIRECTION ( 'NONE',  ( 1.387778780781424721E-17, -2.403703357979470486E-17, 1.000000000000000000 ) ) ;
#34451 = CIRCLE ( 'NONE', #4527, 33.00000000000001421 ) ;
#34452 = VECTOR ( 'NONE', #25304, 1000.000000000000000 ) ;
#34453 = DIRECTION ( 'NONE',  ( 0.000000000000000000, 0.000000000000000000, 1.000000000000000000 ) ) ;
#34454 = DIRECTION ( 'NONE',  ( 1.000000000000000000, 0.000000000000000000, 0.000000000000000000 ) ) ;
#34455 = DIRECTION ( 'NONE',  ( 0.000000000000000000, 0.000000000000000000, 1.000000000000000000 ) ) ;
#34456 = ORIENTED_EDGE ( 'NONE', *, *, #27757, .F. ) ;
#34457 = DIRECTION ( 'NONE',  ( 0.000000000000000000, 0.000000000000000000, 1.000000000000000000 ) ) ;
#34458 = FACE_OUTER_BOUND ( 'NONE', #23545, .T. ) ;
#34459 = CIRCLE ( 'NONE', #26066, 2.000000000000001776 ) ;
#34460 = DIRECTION ( 'NONE',  ( 0.000000000000000000, 0.000000000000000000, 1.000000000000000000 ) ) ;
#34461 = VECTOR ( 'NONE', #10965, 1000.000000000000000 ) ;
#34462 = CIRCLE ( 'NONE', #36865, 3.500000000000003109 ) ;
#34463 = VERTEX_POINT ( 'NONE', #3792 ) ;
#34464 = ORIENTED_EDGE ( 'NONE', *, *, #7847, .F. ) ;
#34465 = ORIENTED_EDGE ( 'NONE', *, *, #17072, .T. ) ;
#34466 = EDGE_CURVE ( 'NONE', #1512, #30600, #28284, .T. ) ;
#34467 = DIRECTION ( 'NONE',  ( 0.000000000000000000, 0.000000000000000000, 1.000000000000000000 ) ) ;
#34468 = VECTOR ( 'NONE', #16802, 1000.000000000000000 ) ;
#34469 = DIRECTION ( 'NONE',  ( -1.000000000000000000, 0.000000000000000000, -0.000000000000000000 ) ) ;
#34470 = FACE_OUTER_BOUND ( 'NONE', #10253, .T. ) ;
#34471 = DIRECTION ( 'NONE',  ( -1.000000000000000000, 0.000000000000000000, 0.000000000000000000 ) ) ;
#34472 = AXIS2_PLACEMENT_3D ( 'NONE', #1265, #13070, #20960 ) ;
#34473 = B_SPLINE_CURVE_WITH_KNOTS ( 'NONE', 3,
 ( #8424, #10860, #36732, #27723, #5043, #25678, #10482, #22297, #16857, #30908, #22468, #8239, #33923, #28278, #2598, #21926, #14026, #25474, #19851, #33370, #36913, #11224, #22673, #31272, #5594, #17965, #11569, #31987 ),
 .UNSPECIFIED., .F., .F.,
 ( 4, 2, 1, 2, 2, 1, 1, 2, 2, 1, 2, 2, 1, 1, 2, 2, 4 ),
 ( 0.05563282717593193150, 0.06430909872693714446, 0.07298537027794235743, 0.09033791337995278337, 0.1250429995839733577, 0.1597480857879939320, 0.1771006288900040526, 0.1857769004410091129, 0.1944531719920141732, 0.2291582581960339982, 0.2465108012980439245, 0.2551870728490489015, 0.2638633444000538786, 0.2985684306040737868, 0.3072447021550788193, 0.3159209737060837964, 0.3332735168080938615 ),
 .UNSPECIFIED. ) ;
#34474 = AXIS2_PLACEMENT_3D ( 'NONE', #8308, #19733, #22908 ) ;
#34475 = CARTESIAN_POINT ( 'NONE',  ( -5.000000000000000888, 2.119000125145918734, -3.842087316602514679 ) ) ;
#34476 = AXIS2_PLACEMENT_3D ( 'NONE', #21102, #9286, #6844 ) ;
#34477 = EDGE_LOOP ( 'NONE', ( #8244, #24898, #24383, #24463 ) ) ;
#34478 = EDGE_LOOP ( 'NONE', ( #24213, #7446, #24712, #35333 ) ) ;
#34479 = DIRECTION ( 'NONE',  ( 0.000000000000000000, 0.000000000000000000, 1.000000000000000000 ) ) ;
#34480 = DIRECTION ( 'NONE',  ( -1.000000000000000000, 0.000000000000000000, 0.000000000000000000 ) ) ;
#34481 = CARTESIAN_POINT ( 'NONE',  ( -75.00000337463097821, 8.660254037844374864, 17.49999999999999645 ) ) ;
#34482 = ORIENTED_EDGE ( 'NONE', *, *, #7847, .T. ) ;
#34483 = AXIS2_PLACEMENT_3D ( 'NONE', #882, #26398, #1263 ) ;
#34484 = DIRECTION ( 'NONE',  ( 0.000000000000000000, 0.000000000000000000, -1.000000000000000000 ) ) ;
#34485 = ORIENTED_EDGE ( 'NONE', *, *, #12686, .F. ) ;
#34486 = ORIENTED_EDGE ( 'NONE', *, *, #30500, .F. ) ;
#34487 = ADVANCED_FACE ( 'NONE', ( #25943 ), #18990, .T. ) ;
#34488 = FACE_OUTER_BOUND ( 'NONE', #22254, .T. ) ;
#34489 = ORIENTED_EDGE ( 'NONE', *, *, #35582, .T. ) ;
#34490 = AXIS2_PLACEMENT_3D ( 'NONE', #25071, #33853, #14356 ) ;
#34491 = CARTESIAN_POINT ( 'NONE',  ( 37.50000000000000000, 103.4105893997321743, -19.99999999999999645 ) ) ;
#34492 = VECTOR ( 'NONE', #13011, 1000.000000000000000 ) ;
#34493 = DIRECTION ( 'NONE',  ( -0.000000000000000000, 0.000000000000000000, -1.000000000000000000 ) ) ;
#34494 = ORIENTED_EDGE ( 'NONE', *, *, #17942, .F. ) ;
#34495 = ORIENTED_EDGE ( 'NONE', *, *, #2945, .F. ) ;
#34496 = VECTOR ( 'NONE', #29946, 1000.000000000000000 ) ;
#34497 = ORIENTED_EDGE ( 'NONE', *, *, #9145, .F. ) ;
#34498 = CIRCLE ( 'NONE', #2163, 2.000000000000001776 ) ;
#34499 = CIRCLE ( 'NONE', #36885, 2.000000000000001776 ) ;
#34500 = ORIENTED_EDGE ( 'NONE', *, *, #6074, .F. ) ;
#34501 = AXIS2_PLACEMENT_3D ( 'NONE', #31635, #17399, #20014 ) ;
#34502 = ORIENTED_EDGE ( 'NONE', *, *, #12075, .T. ) ;
#34503 = DIRECTION ( 'NONE',  ( 0.000000000000000000, -0.000000000000000000, -1.000000000000000000 ) ) ;
#34504 = CARTESIAN_POINT ( 'NONE',  ( 9.999996625368625658, 86.60254037844397601, -9.999999999999998224 ) ) ;
#34505 = FACE_OUTER_BOUND ( 'NONE', #6725, .T. ) ;
#34506 = DIRECTION ( 'NONE',  ( 0.000000000000000000, 0.000000000000000000, -1.000000000000000000 ) ) ;
#34507 = DIRECTION ( 'NONE',  ( 0.000000000000000000, 0.000000000000000000, -1.000000000000000000 ) ) ;
#34508 = ADVANCED_FACE ( 'NONE', ( #33424 ), #21615, .F. ) ;
#34509 = ORIENTED_EDGE ( 'NONE', *, *, #25421, .F. ) ;
#34510 = CARTESIAN_POINT ( 'NONE',  ( -31.46585318596190106, -86.45172111230344569, 12.49999999999999822 ) ) ;
#34511 = CARTESIAN_POINT ( 'NONE',  ( -0.8665032349992070060, -5.555903485205192283, -4.190643565754955446 ) ) ;
#34512 = CARTESIAN_POINT ( 'NONE',  ( -2.000003374631334818, 69.28203230275516944, -5.000000000000000000 ) ) ;
#34513 = ORIENTED_EDGE ( 'NONE', *, *, #12809, .T. ) ;
#34514 = CARTESIAN_POINT ( 'NONE',  ( -19.13981058454750794, 60.93295298010998806, 12.49999999999999822 ) ) ;
#34515 = EDGE_CURVE ( 'NONE', #5895, #25177, #3134, .T. ) ;
#34516 = DIRECTION ( 'NONE',  ( 0.000000000000000000, 0.000000000000000000, 1.000000000000000000 ) ) ;
#34517 = ORIENTED_EDGE ( 'NONE', *, *, #36938, .T. ) ;
#34518 = VECTOR ( 'NONE', #11309, 1000.000000000000000 ) ;
#34519 = VERTEX_POINT ( 'NONE', #16182 ) ;
#34520 = EDGE_CURVE ( 'NONE', #36052, #20938, #22303, .T. ) ;
#34521 = CYLINDRICAL_SURFACE ( 'NONE', #6871, 2.000000000000000000 ) ;
#34522 = AXIS2_PLACEMENT_3D ( 'NONE', #10521, #7721, #7345 ) ;
#34523 = DIRECTION ( 'NONE',  ( 0.000000000000000000, 0.000000000000000000, -1.000000000000000000 ) ) ;
#34524 = FACE_BOUND ( 'NONE', #16363, .T. ) ;
#34525 = LINE ( 'NONE', #14830, #33472 ) ;
#34526 = AXIS2_PLACEMENT_3D ( 'NONE', #12485, #3132, #11740 ) ;
#34527 = ORIENTED_EDGE ( 'NONE', *, *, #5523, .T. ) ;
#34528 = AXIS2_PLACEMENT_3D ( 'NONE', #19587, #2695, #28202 ) ;
#34529 = AXIS2_PLACEMENT_3D ( 'NONE', #6876, #12504, #26949 ) ;
#34530 = CIRCLE ( 'NONE', #36332, 2.000000000000001776 ) ;
#34531 = CYLINDRICAL_SURFACE ( 'NONE', #29081, 3.000000000000002665 ) ;
#34533 = VECTOR ( 'NONE', #36605, 1000.000000000000000 ) ;
#34532 = CARTESIAN_POINT ( 'NONE',  ( 59.99999662536842493, 51.96152422706639129, 12.50000000000000000 ) ) ;
#34534 = DIRECTION ( 'NONE',  ( 0.000000000000000000, -0.000000000000000000, -1.000000000000000000 ) ) ;
#34535 = CIRCLE ( 'NONE', #21953, 2.000000000000000000 ) ;
#34536 = EDGE_LOOP ( 'NONE', ( #1651, #19126 ) ) ;
#34537 = EDGE_CURVE ( 'NONE', #16351, #25578, #32658, .T. ) ;
#34538 = DIRECTION ( 'NONE',  ( 0.000000000000000000, 0.000000000000000000, 1.000000000000000000 ) ) ;
#34539 = ORIENTED_EDGE ( 'NONE', *, *, #15546, .F. ) ;
#34540 = ORIENTED_EDGE ( 'NONE', *, *, #11690, .F. ) ;
#34541 = VECTOR ( 'NONE', #22956, 1000.000000000000000 ) ;
#34542 = CYLINDRICAL_SURFACE ( 'NONE', #30164, 2.000000000000001776 ) ;
#34543 = CARTESIAN_POINT ( 'NONE',  ( 69.99999662536839651, 17.32050807568879236, 12.50000000000000000 ) ) ;
#34544 = ORIENTED_EDGE ( 'NONE', *, *, #1319, .F. ) ;
#34545 = ORIENTED_EDGE ( 'NONE', *, *, #22844, .T. ) ;
#34546 = CARTESIAN_POINT ( 'NONE',  ( 82.99999662536832545, 25.98076211353319565, -9.999999999999998224 ) ) ;
#34547 = AXIS2_PLACEMENT_3D ( 'NONE', #33199, #35308, #15600 ) ;
#34548 = EDGE_CURVE ( 'NONE', #27432, #745, #13913, .T. ) ;
#34549 = CARTESIAN_POINT ( 'NONE',  ( 67.99999662536839651, 51.96152422706640550, -5.000000000000000000 ) ) ;
#34550 = DIRECTION ( 'NONE',  ( 1.000000000000000000, 0.000000000000000000, 0.000000000000000000 ) ) ;
#34551 = CIRCLE ( 'NONE', #11771, 2.000000000000001776 ) ;
#34552 = ORIENTED_EDGE ( 'NONE', *, *, #4373, .F. ) ;
#34553 = FACE_OUTER_BOUND ( 'NONE', #21779, .T. ) ;
#34554 = CLOSED_SHELL ( 'NONE', ( #16534, #8, #27993, #36919, #8402, #5448, #24118, #22733, #29497, #2092, #12707, #25188, #18799, #16064, #4626, #11734, #10936, #18002, #18763, #29186, #12765, #35877, #2207, #21802, #18108, #27696, #5904, #30622, #6576, #21583, #17876, #32139, #13297, #31680, #35336, #33254, #5181, #27105, #24778, #26396, #3819, #10065, #8514 ) ) ;
#34555 = ADVANCED_FACE ( 'NONE', ( #1737 ), #3990, .T. ) ;
#34556 = FACE_BOUND ( 'NONE', #14389, .T. ) ;
#34557 = CARTESIAN_POINT ( 'NONE',  ( 98.21839120950853896, -66.76535579868571801, 32.50000000000000000 ) ) ;
#34558 = CARTESIAN_POINT ( 'NONE',  ( 66.99999662536842493, 43.30127018922200222, 17.49999999999999645 ) ) ;
#34559 = PLANE ( 'NONE',  #34863 ) ;
#34560 = CARTESIAN_POINT ( 'NONE',  ( -2.000003374631303732, -86.60254037844400443, -9.999999999999998224 ) ) ;
#34561 = AXIS2_PLACEMENT_3D ( 'NONE', #20683, #11511, #26499 ) ;
#34562 = CARTESIAN_POINT ( 'NONE',  ( -37.50000000000000000, 103.4105893997321886, -19.99999999999999645 ) ) ;
#34563 = ADVANCED_FACE ( 'NONE', ( #4548 ), #15794, .F. ) ;
#34564 = AXIS2_PLACEMENT_3D ( 'NONE', #25133, #7877, #14027 ) ;
#34565 = VECTOR ( 'NONE', #16877, 1000.000000000000000 ) ;
#34566 = AXIS2_PLACEMENT_3D ( 'NONE', #36082, #10379, #36457 ) ;
#34567 = DIRECTION ( 'NONE',  ( 0.000000000000000000, 0.000000000000000000, 1.000000000000000000 ) ) ;
#34568 = DIRECTION ( 'NONE',  ( 0.000000000000000000, 0.000000000000000000, 1.000000000000000000 ) ) ;
#34569 = ORIENTED_EDGE ( 'NONE', *, *, #31595, .T. ) ;
#34570 = CARTESIAN_POINT ( 'NONE',  ( -111.8061974404896262, 19.22934205795090534, 32.50000000000000000 ) ) ;
#34571 = ADVANCED_FACE ( 'NONE', ( #27605 ), #27217, .F. ) ;
#34572 = DIRECTION ( 'NONE',  ( 0.000000000000000000, 0.000000000000000000, 1.000000000000000000 ) ) ;
#34573 = DIRECTION ( 'NONE',  ( 0.000000000000000000, 0.000000000000000000, 1.000000000000000000 ) ) ;
#34574 = AXIS2_PLACEMENT_3D ( 'NONE', #27111, #16071, #4631 ) ;
#34575 = ORIENTED_EDGE ( 'NONE', *, *, #18072, .T. ) ;
#34576 = AXIS2_PLACEMENT_3D ( 'NONE', #12173, #17634, #18022 ) ;
#34577 = ORIENTED_EDGE ( 'NONE', *, *, #11316, .F. ) ;
#34578 = EDGE_LOOP ( 'NONE', ( #2625, #22106, #22090, #17990 ) ) ;
#34579 = EDGE_CURVE ( 'NONE', #24524, #14473, #15621, .T. ) ;
#34580 = LINE ( 'NONE', #26671, #36094 ) ;
#34581 = DIRECTION ( 'NONE',  ( 0.000000000000000000, 0.000000000000000000, 1.000000000000000000 ) ) ;
#34582 = CARTESIAN_POINT ( 'NONE',  ( 64.99999662536841072, 25.98076211353318854, -9.999999999999998224 ) ) ;
#34583 = VERTEX_POINT ( 'NONE', #24226 ) ;
#34584 = AXIS2_PLACEMENT_3D ( 'NONE', #15648, #12804, #4023 ) ;
#34585 = AXIS2_PLACEMENT_3D ( 'NONE', #6405, #15912, #30151 ) ;
#34586 = DIRECTION ( 'NONE',  ( 0.000000000000000000, 0.000000000000000000, 1.000000000000000000 ) ) ;
#34587 = AXIS2_PLACEMENT_3D ( 'NONE', #7225, #27461, #21650 ) ;
#34588 = ORIENTED_EDGE ( 'NONE', *, *, #35465, .T. ) ;
#34589 = CARTESIAN_POINT ( 'NONE',  ( -12.20857224668173480, -116.8572664861451642, 32.50000000000000711 ) ) ;
#34590 = ORIENTED_EDGE ( 'NONE', *, *, #36866, .F. ) ;
#34591 = DIRECTION ( 'NONE',  ( 0.000000000000000000, 0.000000000000000000, 1.000000000000000000 ) ) ;
#34592 = ORIENTED_EDGE ( 'NONE', *, *, #15395, .F. ) ;
#34593 = EDGE_LOOP ( 'NONE', ( #10883, #35599, #18356, #36682 ) ) ;
#34594 = AXIS2_PLACEMENT_3D ( 'NONE', #28110, #30909, #27566 ) ;
#34595 = CIRCLE ( 'NONE', #20816, 3.500000000000003109 ) ;
#34596 = EDGE_CURVE ( 'NONE', #6951, #24986, #31279, .T. ) ;
#34597 = CARTESIAN_POINT ( 'NONE',  ( 27.78182860042856461, 56.67878100130339902, -49.86348611802629449 ) ) ;
#34598 = CARTESIAN_POINT ( 'NONE',  ( -110.2237710830522559, 101.7384897088162745, 27.50000000000000000 ) ) ;
#34599 = ORIENTED_EDGE ( 'NONE', *, *, #16057, .F. ) ;
#34600 = DIRECTION ( 'NONE',  ( 1.000000000000000000, 0.000000000000000000, 0.000000000000000000 ) ) ;
#34601 = AXIS2_PLACEMENT_3D ( 'NONE', #6096, #20906, #11895 ) ;
#34602 = EDGE_CURVE ( 'NONE', #21975, #16037, #28862, .T. ) ;
#34603 = DIRECTION ( 'NONE',  ( -0.000000000000000000, -0.000000000000000000, -1.000000000000000000 ) ) ;
#34604 = CARTESIAN_POINT ( 'NONE',  ( 4.279621169095998212, -62.97617850287780072, 12.49999999999999822 ) ) ;
#34605 = ORIENTED_EDGE ( 'NONE', *, *, #18911, .T. ) ;
#34606 = CARTESIAN_POINT ( 'NONE',  ( 77.99999662536833966, 34.64101615137759183, 17.49999999999999645 ) ) ;
#34608 = DIRECTION ( 'NONE',  ( 0.000000000000000000, 0.000000000000000000, 1.000000000000000000 ) ) ;
#34607 = CIRCLE ( 'NONE', #458, 2.000000000000000000 ) ;
#34610 = VERTEX_POINT ( 'NONE', #4358 ) ;
#34609 = ADVANCED_FACE ( 'NONE', ( #33220 ), #36054, .F. ) ;
#34611 = CARTESIAN_POINT ( 'NONE',  ( 22.99999662536857059, 77.94228634059957983, -9.999999999999998224 ) ) ;
#34612 = AXIS2_PLACEMENT_3D ( 'NONE', #8385, #31240, #25261 ) ;
#34613 = CIRCLE ( 'NONE', #17259, 95.00000000000001421 ) ;
#34614 = DIRECTION ( 'NONE',  ( 1.000000000000000000, 0.000000000000000000, 0.000000000000000000 ) ) ;
#34615 = DIRECTION ( 'NONE',  ( 1.000000000000000000, 0.000000000000000000, 0.000000000000000000 ) ) ;
#34617 = AXIS2_PLACEMENT_3D ( 'NONE', #30343, #18732, #13278 ) ;
#34616 = DIRECTION ( 'NONE',  ( 1.000000000000000000, 0.000000000000000000, 0.000000000000000000 ) ) ;
#34618 = CARTESIAN_POINT ( 'NONE',  ( 57.99999662536844625, 34.64101615137759893, -5.000000000000000000 ) ) ;
#34619 = AXIS2_PLACEMENT_3D ( 'NONE', #31895, #32292, #3785 ) ;
#34620 = VERTEX_POINT ( 'NONE', #7540 ) ;
#34621 = DIRECTION ( 'NONE',  ( 0.000000000000000000, 0.000000000000000000, 1.000000000000000000 ) ) ;
#34622 = DIRECTION ( 'NONE',  ( 1.000000000000000000, 0.000000000000000000, 0.000000000000000000 ) ) ;
#34623 = ORIENTED_EDGE ( 'NONE', *, *, #14255, .F. ) ;
#34624 = CIRCLE ( 'NONE', #19652, 2.000000000000001776 ) ;
#34625 = ORIENTED_EDGE ( 'NONE', *, *, #16391, .T. ) ;
#34626 = ORIENTED_EDGE ( 'NONE', *, *, #22975, .T. ) ;
#34627 = ADVANCED_FACE ( 'NONE', ( #12602 ), #21981, .F. ) ;
#34628 =( NAMED_UNIT ( * ) SI_UNIT ( $, .STERADIAN. ) SOLID_ANGLE_UNIT ( ) );
#34629 = DIRECTION ( 'NONE',  ( 0.000000000000000000, 0.000000000000000000, 1.000000000000000000 ) ) ;
#34630 = CARTESIAN_POINT ( 'NONE',  ( 34.99999662536855283, 60.62177826491078747, 17.49999999999999645 ) ) ;
#34631 = AXIS2_PLACEMENT_3D ( 'NONE', #14908, #5927, #28781 ) ;
#34632 = AXIS2_PLACEMENT_3D ( 'NONE', #25750, #5320, #8486 ) ;
#34633 = CYLINDRICAL_SURFACE ( 'NONE', #32028, 2.000000000000001776 ) ;
#34634 = ORIENTED_EDGE ( 'NONE', *, *, #19844, .T. ) ;
#34635 = CARTESIAN_POINT ( 'NONE',  ( 86.99999662536832545, 8.660254037844394404, -5.000000000000000000 ) ) ;
#34636 = VERTEX_POINT ( 'NONE', #1534 ) ;
#34637 = AXIS2_PLACEMENT_3D ( 'NONE', #36098, #36475, #10947 ) ;
#34638 = AXIS2_PLACEMENT_3D ( 'NONE', #29794, #20800, #23612 ) ;
#34639 = FACE_BOUND ( 'NONE', #3657, .T. ) ;
#34640 = AXIS2_PLACEMENT_3D ( 'NONE', #14755, #11747, #23207 ) ;
#34641 = EDGE_CURVE ( 'NONE', #2865, #5973, #19910, .T. ) ;
#34642 = CIRCLE ( 'NONE', #34034, 3.000000000000002665 ) ;
#34643 = CYLINDRICAL_SURFACE ( 'NONE', #32269, 1.999999999999998224 ) ;
#34644 = DIRECTION ( 'NONE',  ( 0.000000000000000000, 0.4999999999999953926, -0.8660254037844412611 ) ) ;
#34645 = EDGE_CURVE ( 'NONE', #8370, #9761, #9982, .T. ) ;
#34646 = DIRECTION ( 'NONE',  ( 1.000000000000000000, 0.000000000000000000, 0.000000000000000000 ) ) ;
#34647 = DIRECTION ( 'NONE',  ( 0.000000000000000000, 0.000000000000000000, 1.000000000000000000 ) ) ;
#34648 = EDGE_CURVE ( 'NONE', #31778, #17896, #15715, .T. ) ;
#34649 = CARTESIAN_POINT ( 'NONE',  ( -45.00000337463111322, 77.94228634059959404, 12.50000000000000000 ) ) ;
#34650 = CIRCLE ( 'NONE', #31628, 2.000000000000000000 ) ;
#34651 = CARTESIAN_POINT ( 'NONE',  ( -2.778182860043013847, -66.86787810013035482, -49.86348611802629449 ) ) ;
#34652 = DIRECTION ( 'NONE',  ( -1.000000000000000000, 0.000000000000000000, -0.000000000000000000 ) ) ;
#34653 = ORIENTED_EDGE ( 'NONE', *, *, #25374, .T. ) ;
#34654 = CARTESIAN_POINT ( 'NONE',  ( -70.00000337463102085, -34.64101615137762025, 12.50000000000000000 ) ) ;
#34655 = EDGE_CURVE ( 'NONE', #23066, #21363, #10736, .T. ) ;
#34656 = DIRECTION ( 'NONE',  ( 0.000000000000000000, 0.000000000000000000, -1.000000000000000000 ) ) ;
#34657 = AXIS2_PLACEMENT_3D ( 'NONE', #10116, #29979, #21545 ) ;
#34658 = DIRECTION ( 'NONE',  ( 1.000000000000000000, 0.000000000000000000, 0.000000000000000000 ) ) ;
#34659 = EDGE_CURVE ( 'NONE', #18483, #6666, #30083, .T. ) ;
#34660 = ORIENTED_EDGE ( 'NONE', *, *, #10816, .F. ) ;
#34661 = ORIENTED_EDGE ( 'NONE', *, *, #5268, .T. ) ;
#34662 = VECTOR ( 'NONE', #26841, 1000.000000000000000 ) ;
#34663 = VERTEX_POINT ( 'NONE', #33613 ) ;
#34664 = CIRCLE ( 'NONE', #26890, 3.000000000000000888 ) ;
#34665 = LINE ( 'NONE', #32557, #30902 ) ;
#34666 = EDGE_CURVE ( 'NONE', #1946, #13968, #6739, .T. ) ;
#34667 = ADVANCED_FACE ( 'NONE', ( #2647 ), #32240, .F. ) ;
#34668 = DIRECTION ( 'NONE',  ( 0.000000000000000000, 0.000000000000000000, 1.000000000000000000 ) ) ;
#34669 = CONICAL_SURFACE ( 'NONE', #29235, 4.749999999999999112, 0.4572823821333981131 ) ;
#34670 = ADVANCED_FACE ( 'NONE', ( #13526 ), #7738, .F. ) ;
#34671 = EDGE_CURVE ( 'NONE', #10470, #8482, #9118, .T. ) ;
#34672 = CIRCLE ( 'NONE', #22697, 2.000000000000000000 ) ;
#34673 = DIRECTION ( 'NONE',  ( 1.000000000000000000, 0.000000000000000000, 0.000000000000000000 ) ) ;
#34674 = CARTESIAN_POINT ( 'NONE',  ( -5.000003374631307729, 77.94228634059957983, -9.999999999999998224 ) ) ;
#34675 = DIRECTION ( 'NONE',  ( 1.000000000000000000, 0.000000000000000000, 0.000000000000000000 ) ) ;
#34677 = CARTESIAN_POINT ( 'NONE',  ( -33.99999999999999289, 103.4105893997321886, 27.49999999999999645 ) ) ;
#34676 = AXIS2_PLACEMENT_3D ( 'NONE', #25486, #18984, #31283 ) ;
#34678 = EDGE_LOOP ( 'NONE', ( #638, #1120, #29978, #34660 ) ) ;
#34679 = ORIENTED_EDGE ( 'NONE', *, *, #15694, .T. ) ;
#34680 = AXIS2_PLACEMENT_3D ( 'NONE', #14852, #12383, #26292 ) ;
#34681 = DIRECTION ( 'NONE',  ( 0.000000000000000000, 0.000000000000000000, 1.000000000000000000 ) ) ;
#34682 = DIRECTION ( 'NONE',  ( 0.000000000000000000, 0.000000000000000000, -1.000000000000000000 ) ) ;
#34683 = CARTESIAN_POINT ( 'NONE',  ( 52.39915983220795681, 35.19434990244919703, -4.999999999999997335 ) ) ;
#34684 = EDGE_LOOP ( 'NONE', ( #1283, #8762, #32878, #421 ) ) ;
#34685 = DIRECTION ( 'NONE',  ( 1.000000000000000000, 0.000000000000000000, 0.000000000000000000 ) ) ;
#34686 = AXIS2_PLACEMENT_3D ( 'NONE', #30539, #13275, #21905 ) ;
#34687 = ORIENTED_EDGE ( 'NONE', *, *, #14181, .T. ) ;
#34688 = ORIENTED_EDGE ( 'NONE', *, *, #32320, .T. ) ;
#34689 = CIRCLE ( 'NONE', #22722, 2.000000000000001776 ) ;
#34690 = DIRECTION ( 'NONE',  ( -0.000000000000000000, -0.000000000000000000, 1.000000000000000000 ) ) ;
#34691 = ORIENTED_EDGE ( 'NONE', *, *, #1528, .F. ) ;
#34692 = DIRECTION ( 'NONE',  ( -1.000000000000000000, 0.000000000000000000, 0.000000000000000000 ) ) ;
#34693 = DIRECTION ( 'NONE',  ( 1.000000000000000000, 0.000000000000000000, 0.000000000000000000 ) ) ;
#34694 = ORIENTED_EDGE ( 'NONE', *, *, #22958, .T. ) ;
#34695 = VERTEX_POINT ( 'NONE', #5097 ) ;
#34696 = AXIS2_PLACEMENT_3D ( 'NONE', #23191, #28969, #20932 ) ;
#34697 = ORIENTED_EDGE ( 'NONE', *, *, #36814, .T. ) ;
#34698 = ORIENTED_EDGE ( 'NONE', *, *, #31560, .T. ) ;
#34699 = CIRCLE ( 'NONE', #13736, 2.000000000000001776 ) ;
#34700 = VERTEX_POINT ( 'NONE', #16353 ) ;
#34701 = DIRECTION ( 'NONE',  ( 1.000000000000000000, 0.000000000000000000, 0.000000000000000000 ) ) ;
#34703 = DIRECTION ( 'NONE',  ( 1.000000000000000000, 0.000000000000000000, 0.000000000000000000 ) ) ;
#34702 = CIRCLE ( 'NONE', #10746, 2.000000000000001776 ) ;
#34704 = DIRECTION ( 'NONE',  ( 0.000000000000000000, 0.000000000000000000, -1.000000000000000000 ) ) ;
#34705 = DIRECTION ( 'NONE',  ( 0.000000000000000000, 0.000000000000000000, 1.000000000000000000 ) ) ;
#34706 = DIRECTION ( 'NONE',  ( -0.000000000000000000, -0.000000000000000000, 1.000000000000000000 ) ) ;
#34707 = ORIENTED_EDGE ( 'NONE', *, *, #7365, .F. ) ;
#34708 = DIRECTION ( 'NONE',  ( -1.000000000000000000, 0.000000000000000000, 0.000000000000000000 ) ) ;
#34709 = DIRECTION ( 'NONE',  ( 1.000000000000000000, 0.000000000000000000, 0.000000000000000000 ) ) ;
#34710 = AXIS2_PLACEMENT_3D ( 'NONE', #30187, #7707, #19156 ) ;
#34711 = AXIS2_PLACEMENT_3D ( 'NONE', #36505, #30496, #16069 ) ;
#34712 = EDGE_CURVE ( 'NONE', #3789, #5373, #32483, .T. ) ;
#34713 = DIRECTION ( 'NONE',  ( 1.000000000000000000, 0.000000000000000000, 0.000000000000000000 ) ) ;
#34714 = VERTEX_POINT ( 'NONE', #31160 ) ;
#34715 = CARTESIAN_POINT ( 'NONE',  ( 46.99999662536851019, -60.62177826491080168, 12.50000000000000000 ) ) ;
#34716 = CIRCLE ( 'NONE', #9573, 33.00000000000001421 ) ;
#34717 = DIRECTION ( 'NONE',  ( 1.000000000000000000, 0.000000000000000000, 0.000000000000000000 ) ) ;
#34718 = ORIENTED_EDGE ( 'NONE', *, *, #15836, .T. ) ;
#34719 = ORIENTED_EDGE ( 'NONE', *, *, #20087, .T. ) ;
#34720 = FACE_OUTER_BOUND ( 'NONE', #33035, .T. ) ;
#34721 = CARTESIAN_POINT ( 'NONE',  ( -59.13646009116099833, 70.47608876694653190, 12.49999999999999822 ) ) ;
#34722 = DIRECTION ( 'NONE',  ( 0.000000000000000000, 0.000000000000000000, 1.000000000000000000 ) ) ;
#34723 = DIRECTION ( 'NONE',  ( 0.000000000000000000, 0.000000000000000000, 1.000000000000000000 ) ) ;
#34724 = ORIENTED_EDGE ( 'NONE', *, *, #19239, .T. ) ;
#34725 = AXIS2_PLACEMENT_3D ( 'NONE', #5158, #22394, #5704 ) ;
#34726 = CARTESIAN_POINT ( 'NONE',  ( -52.39915983220772233, -35.19434990244957362, -49.22241343995298024 ) ) ;
#34727 = CARTESIAN_POINT ( 'NONE',  ( 95.00000000000001421, 0.000000000000000000, 32.50000000000000000 ) ) ;
#34728 = DIRECTION ( 'NONE',  ( -0.000000000000000000, -0.000000000000000000, 1.000000000000000000 ) ) ;
#34729 = CIRCLE ( 'NONE', #14354, 2.000000000000001776 ) ;
#34730 = ORIENTED_EDGE ( 'NONE', *, *, #4143, .F. ) ;
#34731 = CIRCLE ( 'NONE', #28745, 2.000000000000001776 ) ;
#34732 = FACE_OUTER_BOUND ( 'NONE', #10509, .T. ) ;
#34733 = AXIS2_PLACEMENT_3D ( 'NONE', #2631, #10887, #10716 ) ;
#34734 = VERTEX_POINT ( 'NONE', #24990 ) ;
#34735 = ADVANCED_FACE ( 'NONE', ( #11281 ), #27970, .F. ) ;
#34736 = EDGE_CURVE ( 'NONE', #17798, #13025, #144, .T. ) ;
#34737 = DIRECTION ( 'NONE',  ( 0.000000000000000000, 0.000000000000000000, -1.000000000000000000 ) ) ;
#34738 = CARTESIAN_POINT ( 'NONE',  ( -70.00000337463102085, -34.64101615137762025, -5.000000000000000000 ) ) ;
#34739 = AXIS2_PLACEMENT_3D ( 'NONE', #31225, #34608, #14904 ) ;
#34740 = CARTESIAN_POINT ( 'NONE',  ( -57.00000337463109901, -60.62177826491083010, -9.999999999999998224 ) ) ;
#34741 = ORIENTED_EDGE ( 'NONE', *, *, #8853, .T. ) ;
#34742 = VERTEX_POINT ( 'NONE', #34173 ) ;
#34743 = CIRCLE ( 'NONE', #3020, 6.000000000000005329 ) ;
#34744 = CARTESIAN_POINT ( 'NONE',  ( 9.999996625368625658, 86.60254037844397601, 12.50000000000000000 ) ) ;
#34745 = DIRECTION ( 'NONE',  ( 1.000000000000000000, 0.000000000000000000, 0.000000000000000000 ) ) ;
#34746 = CARTESIAN_POINT ( 'NONE',  ( 71.99999662536839651, -17.32050807568879947, -9.999999999999998224 ) ) ;
#34747 = EDGE_CURVE ( 'NONE', #28991, #27815, #19899, .T. ) ;
#34748 = ORIENTED_EDGE ( 'NONE', *, *, #29120, .T. ) ;
#34749 = CARTESIAN_POINT ( 'NONE',  ( 44.99999662536851019, -60.62177826491080168, -9.999999999999998224 ) ) ;
#34750 = FACE_BOUND ( 'NONE', #32406, .T. ) ;
#34751 = DIRECTION ( 'NONE',  ( 0.000000000000000000, -0.000000000000000000, -1.000000000000000000 ) ) ;
#34752 = DIRECTION ( 'NONE',  ( -1.000000000000000000, 0.000000000000000000, 0.000000000000000000 ) ) ;
#34753 = DIRECTION ( 'NONE',  ( 0.000000000000000000, 0.000000000000000000, 1.000000000000000000 ) ) ;
#34754 = DIRECTION ( 'NONE',  ( 0.000000000000000000, 0.000000000000000000, 1.000000000000000000 ) ) ;
#34755 =( NAMED_UNIT ( * ) SI_UNIT ( $, .STERADIAN. ) SOLID_ANGLE_UNIT ( ) );
#34756 = AXIS2_PLACEMENT_3D ( 'NONE', #16725, #8459, #11270 ) ;
#34757 = EDGE_CURVE ( 'NONE', #25770, #5185, #21114, .T. ) ;
#34758 = CARTESIAN_POINT ( 'NONE',  ( -70.00000337463099243, -2.428612866367529932E-14, -5.000000000000000000 ) ) ;
#34759 = ORIENTED_EDGE ( 'NONE', *, *, #6003, .T. ) ;
#34760 = CARTESIAN_POINT ( 'NONE',  ( 11.99999662536865763, -86.60254037844400443, -9.999999999999998224 ) ) ;
#34761 = CARTESIAN_POINT ( 'NONE',  ( 3.000000000000000000, 2.201436576420041202, -1.271000000000003460 ) ) ;
#34762 = AXIS2_PLACEMENT_3D ( 'NONE', #32418, #6920, #6732 ) ;
#34763 = CARTESIAN_POINT ( 'NONE',  ( -8.000003374631249997, -86.60254037844400443, -5.000000000000000000 ) ) ;
#34764 = VERTEX_POINT ( 'NONE', #26074 ) ;
#34765 = ORIENTED_EDGE ( 'NONE', *, *, #36536, .F. ) ;
#34766 = ORIENTED_EDGE ( 'NONE', *, *, #20746, .F. ) ;
#34767 = LINE ( 'NONE', #9625, #27314 ) ;
#34768 = CARTESIAN_POINT ( 'NONE',  ( 0.000000000000000000, 0.000000000000000000, 0.000000000000000000 ) ) ;
#34769 = DIRECTION ( 'NONE',  ( -1.000000000000000000, 0.000000000000000000, 0.000000000000000000 ) ) ;
#34770 = VERTEX_POINT ( 'NONE', #3391 ) ;
#34771 = CARTESIAN_POINT ( 'NONE',  ( -45.00000000000000000, 0.000000000000000000, 15.00000000000000000 ) ) ;
#34772 = ORIENTED_EDGE ( 'NONE', *, *, #21568, .F. ) ;
#34773 = EDGE_CURVE ( 'NONE', #15209, #6733, #939, .T. ) ;
#34774 = CARTESIAN_POINT ( 'NONE',  ( 11.99999662536862566, 86.60254037844397601, 17.49999999999999645 ) ) ;
#34775 = ORIENTED_EDGE ( 'NONE', *, *, #1776, .T. ) ;
#34776 = CARTESIAN_POINT ( 'NONE',  ( -80.00000337463094979, 17.32050807568878525, -9.999999999999998224 ) ) ;
#34777 = ORIENTED_EDGE ( 'NONE', *, *, #33729, .F. ) ;
#34778 = ORIENTED_EDGE ( 'NONE', *, *, #27644, .T. ) ;
#34779 = DIRECTION ( 'NONE',  ( 0.000000000000000000, 0.000000000000000000, 1.000000000000000000 ) ) ;
#34780 = CARTESIAN_POINT ( 'NONE',  ( -43.00000337463111322, 60.62177826491077326, -5.000000000000000000 ) ) ;
#34782 = AXIS2_PLACEMENT_3D ( 'NONE', #10857, #30904, #16131 ) ;
#34781 = DIRECTION ( 'NONE',  ( 1.000000000000000000, 0.000000000000000000, 0.000000000000000000 ) ) ;
#34783 = ADVANCED_FACE ( 'NONE', ( #9185 ), #6382, .F. ) ;
#34784 = VERTEX_POINT ( 'NONE', #3039 ) ;
#34785 = CARTESIAN_POINT ( 'NONE',  ( -58.88972745734203329, -33.99999999999965894, -49.86561046011506448 ) ) ;
#34786 = DIRECTION ( 'NONE',  ( 1.000000000000000000, 0.000000000000000000, 0.000000000000000000 ) ) ;
#34787 = DIRECTION ( 'NONE',  ( 0.000000000000000000, 0.000000000000000000, 1.000000000000000000 ) ) ;
#34788 = EDGE_CURVE ( 'NONE', #33480, #12339, #25303, .T. ) ;
#34789 = ORIENTED_EDGE ( 'NONE', *, *, #25021, .T. ) ;
#34790 = DIRECTION ( 'NONE',  ( 0.000000000000000000, 0.000000000000000000, 1.000000000000000000 ) ) ;
#34791 = CARTESIAN_POINT ( 'NONE',  ( -68.66839587347244844, -56.74224907229008608, 12.49999999999999645 ) ) ;
#34792 = ORIENTED_EDGE ( 'NONE', *, *, #4659, .F. ) ;
#34793 = DIRECTION ( 'NONE',  ( 0.000000000000000000, 0.000000000000000000, 1.000000000000000000 ) ) ;
#34794 = DIRECTION ( 'NONE',  ( 0.000000000000000000, 0.000000000000000000, -1.000000000000000000 ) ) ;
#34795 = DIRECTION ( 'NONE',  ( 0.000000000000000000, 0.000000000000000000, 1.000000000000000000 ) ) ;
#34796 = PLANE ( 'NONE',  #18873 ) ;
#34797 = CARTESIAN_POINT ( 'NONE',  ( 44.99999662536851019, 77.94228634059959404, 17.49999999999999645 ) ) ;
#34798 = DIRECTION ( 'NONE',  ( 0.000000000000000000, 0.000000000000000000, 1.000000000000000000 ) ) ;
#34799 = ORIENTED_EDGE ( 'NONE', *, *, #32470, .T. ) ;
#34800 = DIRECTION ( 'NONE',  ( -0.000000000000000000, -0.000000000000000000, 1.000000000000000000 ) ) ;
#34801 = CARTESIAN_POINT ( 'NONE',  ( -6.216324218022825094E-15, 6.066067634115565710, -4.359491423763658169 ) ) ;
#34802 = CARTESIAN_POINT ( 'NONE',  ( 46.99999662536851019, -60.62177826491080168, -9.999999999999998224 ) ) ;
#34803 = ORIENTED_EDGE ( 'NONE', *, *, #25511, .F. ) ;
#34804 = EDGE_CURVE ( 'NONE', #18782, #5564, #22323, .T. ) ;
#34805 = ORIENTED_EDGE ( 'NONE', *, *, #3843, .T. ) ;
#34806 = EDGE_LOOP ( 'NONE', ( #21376, #7777, #6378, #11986, #7103 ) ) ;
#34807 = CIRCLE ( 'NONE', #16843, 6.000000000000005329 ) ;
#34808 = CARTESIAN_POINT ( 'NONE',  ( -6.912404044025940083E-14, -5.987311224403031318, -4.330826434870623132 ) ) ;
#34809 = CARTESIAN_POINT ( 'NONE',  ( 74.99999662536835388, -25.98076211353319565, -5.000000000000000000 ) ) ;
#34810 = DIRECTION ( 'NONE',  ( 0.000000000000000000, 0.000000000000000000, 1.000000000000000000 ) ) ;
#34811 = EDGE_CURVE ( 'NONE', #2942, #553, #14554, .T. ) ;
#34812 = CARTESIAN_POINT ( 'NONE',  ( 9.999996625368618552, 69.28203230275516944, -9.999999999999998224 ) ) ;
#34813 = ORIENTED_EDGE ( 'NONE', *, *, #16587, .T. ) ;
#34814 = EDGE_CURVE ( 'NONE', #29485, #12595, #4981, .T. ) ;
#34815 = CARTESIAN_POINT ( 'NONE',  ( -60.00000337463108480, -51.96152422706641971, -9.999999999999998224 ) ) ;
#34816 = ORIENTED_EDGE ( 'NONE', *, *, #26345, .T. ) ;
#34817 = FACE_BOUND ( 'NONE', #6362, .T. ) ;
#34818 = CYLINDRICAL_SURFACE ( 'NONE', #17353, 2.000000000000000000 ) ;
#34819 = CARTESIAN_POINT ( 'NONE',  ( 19.99999662536857770, 86.60254037844397601, -9.999999999999998224 ) ) ;
#34820 = ORIENTED_EDGE ( 'NONE', *, *, #11528, .T. ) ;
#34821 = CARTESIAN_POINT ( 'NONE',  ( -6.000000000000000000, 0.000000000000000000, 27.50000000000000000 ) ) ;
#34822 = CIRCLE ( 'NONE', #13266, 27.00000000000001776 ) ;
#34823 = CARTESIAN_POINT ( 'NONE',  ( 59.29837256189581041, 31.02796211690886707, 12.49999999999999822 ) ) ;
#34824 = EDGE_CURVE ( 'NONE', #27465, #6217, #28886, .T. ) ;
#34825 = CARTESIAN_POINT ( 'NONE',  ( -65.00000337463102085, 60.62177826491077326, -9.999999999999998224 ) ) ;
#34826 = CARTESIAN_POINT ( 'NONE',  ( -50.00000337463109190, 69.28203230275518365, 12.50000000000000000 ) ) ;
#34827 = VERTEX_POINT ( 'NONE', #8830 ) ;
#34828 = FACE_OUTER_BOUND ( 'NONE', #23251, .T. ) ;
#34829 = FACE_OUTER_BOUND ( 'NONE', #29030, .T. ) ;
#34830 = CARTESIAN_POINT ( 'NONE',  ( 61.99999662536843914, -34.64101615137759893, -9.999999999999998224 ) ) ;
#34831 = VERTEX_POINT ( 'NONE', #15190 ) ;
#34832 = ORIENTED_EDGE ( 'NONE', *, *, #10813, .T. ) ;
#34833 =( REPRESENTATION_RELATIONSHIP ('NONE','NONE', #15268, #34443 ) REPRESENTATION_RELATIONSHIP_WITH_TRANSFORMATION ( #22965 )SHAPE_REPRESENTATION_RELATIONSHIP( ) );
#34834 = ORIENTED_EDGE ( 'NONE', *, *, #21261, .F. ) ;
#34835 = FACE_OUTER_BOUND ( 'NONE', #7075, .T. ) ;
#34836 = FACE_OUTER_BOUND ( 'NONE', #14583, .T. ) ;
#34837 = ADVANCED_FACE ( 'NONE', ( #18013 ), #11814, .T. ) ;
#34838 = DIRECTION ( 'NONE',  ( -0.000000000000000000, -0.000000000000000000, 1.000000000000000000 ) ) ;
#34839 = CARTESIAN_POINT ( 'NONE',  ( -45.00000337463111322, 60.62177826491077326, -5.000000000000000000 ) ) ;
#34840 = EDGE_CURVE ( 'NONE', #7880, #3751, #34893, .T. ) ;
#34841 = CIRCLE ( 'NONE', #9690, 2.000000000000001776 ) ;
#34842 = CARTESIAN_POINT ( 'NONE',  ( -25.00000337463120914, 77.94228634059957983, -5.000000000000000000 ) ) ;
#34843 = CARTESIAN_POINT ( 'NONE',  ( 3.499999999999991562, -55.00000000000000000, -5.000000000000000000 ) ) ;
#34844 = VERTEX_POINT ( 'NONE', #20615 ) ;
#34845 = EDGE_CURVE ( 'NONE', #21657, #16356, #32510, .T. ) ;
#34846 = ORIENTED_EDGE ( 'NONE', *, *, #19894, .T. ) ;
#34847 = CARTESIAN_POINT ( 'NONE',  ( -85.00000337463092137, 25.98076211353317433, -5.000000000000000000 ) ) ;
#34848 = FACE_OUTER_BOUND ( 'NONE', #30018, .T. ) ;
#34849 = DIRECTION ( 'NONE',  ( 1.000000000000000000, 0.000000000000000000, 0.000000000000000000 ) ) ;
#34850 = EDGE_CURVE ( 'NONE', #1195, #31600, #7364, .T. ) ;
#34851 = VERTEX_POINT ( 'NONE', #6193 ) ;
#34852 = EDGE_CURVE ( 'NONE', #19680, #15168, #31875, .T. ) ;
#34853 = FACE_BOUND ( 'NONE', #11519, .T. ) ;
#34854 = EDGE_LOOP ( 'NONE', ( #15076, #24946 ) ) ;
#34855 = VERTEX_POINT ( 'NONE', #23630 ) ;
#34856 = CARTESIAN_POINT ( 'NONE',  ( 2.287832656137188447, -4.452621892014642313, -5.999999999999999112 ) ) ;
#34857 = EDGE_LOOP ( 'NONE', ( #19462, #32383, #12687, #32513, #16270 ) ) ;
#34858 = EDGE_CURVE ( 'NONE', #13344, #23066, #29509, .T. ) ;
#34859 =( NAMED_UNIT ( * ) PLANE_ANGLE_UNIT ( ) SI_UNIT ( $, .RADIAN. ) );
#34860 = ADVANCED_FACE ( 'NONE', ( #751 ), #35076, .F. ) ;
#34861 = CARTESIAN_POINT ( 'NONE',  ( -85.00000337463092137, 8.660254037844389075, 12.50000000000000000 ) ) ;
#34862 = ADVANCED_FACE ( 'NONE', ( #26623 ), #20077, .F. ) ;
#34863 = AXIS2_PLACEMENT_3D ( 'NONE', #8862, #25377, #23306 ) ;
#34864 = DIRECTION ( 'NONE',  ( -0.000000000000000000, 0.000000000000000000, -1.000000000000000000 ) ) ;
#34865 = CARTESIAN_POINT ( 'NONE',  ( -2.778182860043013847, -66.86787810013035482, 12.49999999999999822 ) ) ;
#34866 = EDGE_CURVE ( 'NONE', #22384, #24412, #8567, .T. ) ;
#34867 = VERTEX_POINT ( 'NONE', #35284 ) ;
#34868 = EDGE_CURVE ( 'NONE', #7368, #10592, #26520, .T. ) ;
#34869 = EDGE_LOOP ( 'NONE', ( #31916, #11442, #34949, #15545, #30965, #11752 ) ) ;
#34870 = ORIENTED_EDGE ( 'NONE', *, *, #31663, .T. ) ;
#34871 = VERTEX_POINT ( 'NONE', #30369 ) ;
#34872 = ORIENTED_EDGE ( 'NONE', *, *, #32549, .F. ) ;
#34873 = FACE_OUTER_BOUND ( 'NONE', #35172, .T. ) ;
#34874 = CARTESIAN_POINT ( 'NONE',  ( 0.000000000000000000, 0.000000000000000000, 0.000000000000000000 ) ) ;
#34875 = ORIENTED_EDGE ( 'NONE', *, *, #31744, .T. ) ;
#34876 = CARTESIAN_POINT ( 'NONE',  ( 23.49188653442568864, 103.5527583403323035, 27.49999400000000094 ) ) ;
#34877 = CARTESIAN_POINT ( 'NONE',  ( 106.2299706463093827, 40.32678131133052801, 32.50000000000000000 ) ) ;
#34878 = CARTESIAN_POINT ( 'NONE',  ( 84.99999662536831124, -8.660254037844397956, -5.000000000000000000 ) ) ;
#34879 = ORIENTED_EDGE ( 'NONE', *, *, #15939, .F. ) ;
#34880 = DIRECTION ( 'NONE',  ( 0.000000000000000000, 0.000000000000000000, -1.000000000000000000 ) ) ;
#34881 =( BOUNDED_CURVE ( )  B_SPLINE_CURVE ( 3, ( #32678, #12789, #24242, #10199 ),
 .UNSPECIFIED., .F., .F. ) 
 B_SPLINE_CURVE_WITH_KNOTS ( ( 4, 4 ),
 ( 1.224646799147352468E-16, 1.570796326794907438 ),
 .UNSPECIFIED. ) 
 CURVE ( )  GEOMETRIC_REPRESENTATION_ITEM ( )  RATIONAL_B_SPLINE_CURVE ( ( 1.000000000000000000, 0.8047378541243626060, 0.8047378541243626060, 1.000000000000000000 ) ) 
 REPRESENTATION_ITEM ( '' )  );
#34882 = AXIS2_PLACEMENT_3D ( 'NONE', #17469, #32449, #28885 ) ;
#34883 = VECTOR ( 'NONE', #19727, 1000.000000000000000 ) ;
#34884 = CARTESIAN_POINT ( 'NONE',  ( 69.13212189986965939, 2.778182860042805125, -49.86348611802629449 ) ) ;
#34885 = CARTESIAN_POINT ( 'NONE',  ( -80.00000337463096400, -34.64101615137762025, -5.000000000000000000 ) ) ;
#34886 = EDGE_LOOP ( 'NONE', ( #7150, #32064, #23493, #16554 ) ) ;
#34887 = CARTESIAN_POINT ( 'NONE',  ( 54.99999662536846046, -43.30127018922200222, 17.49999999999999645 ) ) ;
#34888 = DIRECTION ( 'NONE',  ( 0.000000000000000000, 0.000000000000000000, 1.000000000000000000 ) ) ;
#34889 = ORIENTED_EDGE ( 'NONE', *, *, #11484, .F. ) ;
#34890 = ORIENTED_EDGE ( 'NONE', *, *, #26567, .F. ) ;
#34891 = DIRECTION ( 'NONE',  ( 1.000000000000000000, 0.000000000000000000, 0.000000000000000000 ) ) ;
#34892 = CONICAL_SURFACE ( 'NONE', #19342, 3.050000000000000711, 0.7853981633974498333 ) ;
#34893 = LINE ( 'NONE', #20273, #5569 ) ;
#34894 = CARTESIAN_POINT ( 'NONE',  ( 7.041719095097282852E-16, 78.44802294027068967, -24.99999999999999645 ) ) ;
#34895 = CYLINDRICAL_SURFACE ( 'NONE', #19678, 2.000000000000001776 ) ;
#34896 = EDGE_LOOP ( 'NONE', ( #36519, #35558 ) ) ;
#34897 = FACE_OUTER_BOUND ( 'NONE', #28176, .T. ) ;
#34898 = CARTESIAN_POINT ( 'NONE',  ( -63.00000337463102085, 43.30127018922198801, -9.999999999999998224 ) ) ;
#34899 = DIRECTION ( 'NONE',  ( -1.000000000000000000, 0.000000000000000000, -0.000000000000000000 ) ) ;
#34900 = ORIENTED_EDGE ( 'NONE', *, *, #21551, .T. ) ;
#34901 = DIRECTION ( 'NONE',  ( -1.000000000000000000, -0.000000000000000000, -0.000000000000000000 ) ) ;
#34902 = VERTEX_POINT ( 'NONE', #7317 ) ;
#34903 = DIRECTION ( 'NONE',  ( 0.000000000000000000, 0.000000000000000000, -1.000000000000000000 ) ) ;
#34904 = EDGE_CURVE ( 'NONE', #8445, #19786, #16945, .T. ) ;
#34905 = CIRCLE ( 'NONE', #1361, 2.000000000000000000 ) ;
#34906 = CARTESIAN_POINT ( 'NONE',  ( -68.19171733629717380, 52.81598405851951838, 12.50000000000000000 ) ) ;
#34907 = EDGE_CURVE ( 'NONE', #111, #21657, #10360, .T. ) ;
#34908 = DIRECTION ( 'NONE',  ( 0.000000000000000000, 0.000000000000000000, 1.000000000000000000 ) ) ;
#34909 = EDGE_CURVE ( 'NONE', #32638, #11718, #27719, .T. ) ;
#34910 = VERTEX_POINT ( 'NONE', #13132 ) ;
#34911 = EDGE_LOOP ( 'NONE', ( #31602, #29761 ) ) ;
#34912 = DIRECTION ( 'NONE',  ( 0.000000000000000000, 0.4999999999999959477, -0.8660254037844409281 ) ) ;
#34913 = DIRECTION ( 'NONE',  ( 0.000000000000000000, 0.000000000000000000, 1.000000000000000000 ) ) ;
#34914 = DIRECTION ( 'NONE',  ( 1.000000000000000000, 0.000000000000000000, 0.000000000000000000 ) ) ;
#34915 = ORIENTED_EDGE ( 'NONE', *, *, #11731, .F. ) ;
#34916 = CARTESIAN_POINT ( 'NONE',  ( -77.00000337463097821, 8.660254037844374864, -5.000000000000000000 ) ) ;
#34917 = AXIS2_PLACEMENT_3D ( 'NONE', #12246, #18656, #35913 ) ;
#34918 = FACE_BOUND ( 'NONE', #20992, .T. ) ;
#34919 = CARTESIAN_POINT ( 'NONE',  ( -73.00000337463097821, 43.30127018922197379, -9.999999999999998224 ) ) ;
#34920 = CARTESIAN_POINT ( 'NONE',  ( 66.86787810013036903, -2.778182860042780700, -49.86348611802629449 ) ) ;
#34921 = DIRECTION ( 'NONE',  ( 0.000000000000000000, 0.000000000000000000, 1.000000000000000000 ) ) ;
#34922 = ORIENTED_EDGE ( 'NONE', *, *, #7435, .T. ) ;
#34923 = CARTESIAN_POINT ( 'NONE',  ( -6.000000000000000000, 145.0000000000000568, 32.55002500000000509 ) ) ;
#34924 = LINE ( 'NONE', #783, #24776 ) ;
#34925 = ORIENTED_EDGE ( 'NONE', *, *, #34972, .T. ) ;
#34926 = DIRECTION ( 'NONE',  ( 1.000000000000000000, 0.000000000000000000, 0.000000000000000000 ) ) ;
#34927 = DIRECTION ( 'NONE',  ( 0.000000000000000000, 0.000000000000000000, 1.000000000000000000 ) ) ;
#34928 = LINE ( 'NONE', #3435, #31747 ) ;
#34929 = EDGE_CURVE ( 'NONE', #12570, #31248, #15941, .T. ) ;
#34930 = VERTEX_POINT ( 'NONE', #15753 ) ;
#34931 = AXIS2_PLACEMENT_3D ( 'NONE', #11768, #23031, #3543 ) ;
#34932 = ORIENTED_EDGE ( 'NONE', *, *, #28914, .F. ) ;
#34933 = ORIENTED_EDGE ( 'NONE', *, *, #28978, .F. ) ;
#34934 = DIRECTION ( 'NONE',  ( 0.000000000000000000, 0.000000000000000000, 1.000000000000000000 ) ) ;
#34935 = DIRECTION ( 'NONE',  ( 0.000000000000000000, 0.000000000000000000, 1.000000000000000000 ) ) ;
#34936 = CARTESIAN_POINT ( 'NONE',  ( 96.53048327204888324, -102.5304832720499633, 32.55002500000000509 ) ) ;
#34937 = ORIENTED_EDGE ( 'NONE', *, *, #29511, .T. ) ;
#34938 = ORIENTED_EDGE ( 'NONE', *, *, #5453, .F. ) ;
#34939 = VECTOR ( 'NONE', #37048, 1000.000000000000000 ) ;
#34940 = EDGE_CURVE ( 'NONE', #30390, #16972, #15577, .T. ) ;
#34941 = CARTESIAN_POINT ( 'NONE',  ( 59.99999662536843914, -34.64101615137759893, -9.999999999999998224 ) ) ;
#34942 = CIRCLE ( 'NONE', #1399, 2.000000000000001776 ) ;
#34943 = ORIENTED_EDGE ( 'NONE', *, *, #6873, .T. ) ;
#34944 = FACE_OUTER_BOUND ( 'NONE', #6513, .T. ) ;
#34945 = EDGE_LOOP ( 'NONE', ( #33573, #1826 ) ) ;
#34946 = DIRECTION ( 'NONE',  ( 0.000000000000000000, 0.000000000000000000, 1.000000000000000000 ) ) ;
#34947 = EDGE_LOOP ( 'NONE', ( #10580, #13824, #14401, #32528 ) ) ;
#34948 = AXIS2_PLACEMENT_3D ( 'NONE', #23170, #2736, #14538 ) ;
#34949 = ORIENTED_EDGE ( 'NONE', *, *, #170, .F. ) ;
#34950 = DIRECTION ( 'NONE',  ( -0.000000000000000000, -0.000000000000000000, 1.000000000000000000 ) ) ;
#34951 = DIRECTION ( 'NONE',  ( 0.000000000000000000, 0.000000000000000000, -1.000000000000000000 ) ) ;
#34952 = DIRECTION ( 'NONE',  ( -1.000000000000000000, 0.000000000000000000, 0.000000000000000000 ) ) ;
#34953 = EDGE_CURVE ( 'NONE', #8678, #8665, #21380, .T. ) ;
#34954 = VERTEX_POINT ( 'NONE', #21008 ) ;
#34955 = EDGE_LOOP ( 'NONE', ( #11478, #33911 ) ) ;
#34956 = CYLINDRICAL_SURFACE ( 'NONE', #14898, 2.000000000000001776 ) ;
#34957 = AXIS2_PLACEMENT_3D ( 'NONE', #15057, #12413, #26484 ) ;
#34958 = CARTESIAN_POINT ( 'NONE',  ( -56.29165124598824832, 32.50000000000046896, 12.49999999999999822 ) ) ;
#34959 = CARTESIAN_POINT ( 'NONE',  ( -15.97563234535668109, 90.60231327712331506, 12.49999999999999822 ) ) ;
#34960 = AXIS2_PLACEMENT_3D ( 'NONE', #30120, #4448, #36135 ) ;
#34961 = EDGE_LOOP ( 'NONE', ( #14630, #10040 ) ) ;
#34962 = CARTESIAN_POINT ( 'NONE',  ( 46.99999662536849598, -77.94228634059960825, 17.49999999999999645 ) ) ;
#34963 = DIRECTION ( 'NONE',  ( 0.000000000000000000, 0.000000000000000000, 1.000000000000000000 ) ) ;
#34964 = ORIENTED_EDGE ( 'NONE', *, *, #18867, .T. ) ;
#34965 = LINE ( 'NONE', #32131, #18430 ) ;
#34966 = CYLINDRICAL_SURFACE ( 'NONE', #9502, 2.000000000000001776 ) ;
#34967 = DIRECTION ( 'NONE',  ( 1.000000000000000000, 0.000000000000000000, 0.000000000000000000 ) ) ;
#34968 = FACE_BOUND ( 'NONE', #5941, .T. ) ;
#34969 = VECTOR ( 'NONE', #9853, 1000.000000000000000 ) ;
#34970 = DIRECTION ( 'NONE',  ( 0.000000000000000000, 0.000000000000000000, 1.000000000000000000 ) ) ;
#34971 = VECTOR ( 'NONE', #25176, 1000.000000000000000 ) ;
#34972 = EDGE_CURVE ( 'NONE', #12226, #21994, #9140, .T. ) ;
#34973 = CARTESIAN_POINT ( 'NONE',  ( -88.00000337463090716, -1.040834085586084257E-14, -9.999999999999998224 ) ) ;
#34974 = ORIENTED_EDGE ( 'NONE', *, *, #34858, .T. ) ;
#34975 = CYLINDRICAL_SURFACE ( 'NONE', #7630, 2.000000000000001776 ) ;
#34976 = DIRECTION ( 'NONE',  ( 1.000000000000000000, 0.000000000000000000, 0.000000000000000000 ) ) ;
#34977 = DIRECTION ( 'NONE',  ( -1.000000000000000000, 0.000000000000000000, -0.000000000000000000 ) ) ;
#34978 = EDGE_CURVE ( 'NONE', #25502, #6568, #3155, .T. ) ;
#34979 = EDGE_LOOP ( 'NONE', ( #15747, #10035 ) ) ;
#34980 = VERTEX_POINT ( 'NONE', #18754 ) ;
#34981 = ORIENTED_EDGE ( 'NONE', *, *, #10090, .F. ) ;
#34982 = CARTESIAN_POINT ( 'NONE',  ( 4.390739357591696154E-15, -5.773502691896305272, -3.984345921091785758 ) ) ;
#34983 = DIRECTION ( 'NONE',  ( 0.000000000000000000, 0.000000000000000000, 1.000000000000000000 ) ) ;
#34984 = EDGE_CURVE ( 'NONE', #25888, #17256, #1138, .T. ) ;
#34985 = CARTESIAN_POINT ( 'NONE',  ( 76.99999662536835388, -25.98076211353319565, -9.999999999999998224 ) ) ;
#34986 = AXIS2_PLACEMENT_3D ( 'NONE', #31321, #28872, #28160 ) ;
#34987 = LINE ( 'NONE', #14234, #27019 ) ;
#34988 = EDGE_CURVE ( 'NONE', #25264, #26476, #16360, .T. ) ;
#34989 = DIRECTION ( 'NONE',  ( 1.000000000000000000, 0.000000000000000000, 0.000000000000000000 ) ) ;
#34990 = VERTEX_POINT ( 'NONE', #7141 ) ;
#34991 = CARTESIAN_POINT ( 'NONE',  ( 46.99999662536851019, -60.62177826491080168, -9.999999999999998224 ) ) ;
#34992 = VERTEX_POINT ( 'NONE', #1314 ) ;
#34993 = FACE_BOUND ( 'NONE', #15629, .T. ) ;
#34994 = DIRECTION ( 'NONE',  ( 0.000000000000000000, -0.000000000000000000, -1.000000000000000000 ) ) ;
#34995 = AXIS2_PLACEMENT_3D ( 'NONE', #32032, #3381, #35628 ) ;
#34996 = DIRECTION ( 'NONE',  ( 0.000000000000000000, 0.000000000000000000, 1.000000000000000000 ) ) ;
#34997 = ADVANCED_FACE ( 'NONE', ( #7496 ), #33174, .F. ) ;
#34998 = ORIENTED_EDGE ( 'NONE', *, *, #7338, .F. ) ;
#34999 = CARTESIAN_POINT ( 'NONE',  ( 44.99999662536849598, -77.94228634059960825, 17.49999999999999645 ) ) ;
#35000 = APPLICATION_PROTOCOL_DEFINITION ( 'draft international standard', 'automotive_design', 1998, #26899 ) ;
#35001 = DIRECTION ( 'NONE',  ( 0.000000000000000000, 0.000000000000000000, 1.000000000000000000 ) ) ;
#35002 = CARTESIAN_POINT ( 'NONE',  ( 3.000000000000000000, 0.000000000000000000, 0.000000000000000000 ) ) ;
#35003 = DIRECTION ( 'NONE',  ( 0.000000000000000000, 0.000000000000000000, 1.000000000000000000 ) ) ;
#35004 = EDGE_LOOP ( 'NONE', ( #20213, #25277 ) ) ;
#35005 = CARTESIAN_POINT ( 'NONE',  ( -57.00000337463107059, 43.30127018922197379, -9.999999999999998224 ) ) ;
#35006 = CIRCLE ( 'NONE', #9865, 2.000000000000001776 ) ;
#35007 = LINE ( 'NONE', #23398, #5892 ) ;
#35008 = DIRECTION ( 'NONE',  ( 1.000000000000000000, 0.000000000000000000, 0.000000000000000000 ) ) ;
#35009 = EDGE_CURVE ( 'NONE', #9788, #12832, #3938, .T. ) ;
#35010 = ORIENTED_EDGE ( 'NONE', *, *, #13573, .F. ) ;
#35011 = AXIS2_PLACEMENT_3D ( 'NONE', #4142, #3389, #26267 ) ;
#35012 = ORIENTED_EDGE ( 'NONE', *, *, #36316, .T. ) ;
#35013 = EDGE_CURVE ( 'NONE', #27668, #5018, #3765, .T. ) ;
#35014 = ORIENTED_EDGE ( 'NONE', *, *, #9858, .F. ) ;
#35015 = DIRECTION ( 'NONE',  ( 0.000000000000000000, 0.000000000000000000, 1.000000000000000000 ) ) ;
#35016 = EDGE_CURVE ( 'NONE', #29281, #35919, #15741, .T. ) ;
#35017 = CARTESIAN_POINT ( 'NONE',  ( -90.00000337463090716, -1.040834085586084257E-14, 17.49999999999999645 ) ) ;
#35018 = ORIENTED_EDGE ( 'NONE', *, *, #26011, .F. ) ;
#35019 = AXIS2_PLACEMENT_3D ( 'NONE', #22850, #34285, #8587 ) ;
#35020 = DIRECTION ( 'NONE',  ( 1.000000000000000000, 0.000000000000000000, 0.000000000000000000 ) ) ;
#35021 = DIRECTION ( 'NONE',  ( -0.000000000000000000, -0.000000000000000000, 1.000000000000000000 ) ) ;
#35022 = EDGE_CURVE ( 'NONE', #4407, #12415, #6940, .T. ) ;
#35023 = FACE_OUTER_BOUND ( 'NONE', #2998, .T. ) ;
#35024 = ORIENTED_EDGE ( 'NONE', *, *, #7129, .F. ) ;
#35025 = VERTEX_POINT ( 'NONE', #24387 ) ;
#35026 = PLANE ( 'NONE',  #18272 ) ;
#35027 = EDGE_CURVE ( 'NONE', #11389, #18782, #10943, .T. ) ;
#35028 = CARTESIAN_POINT ( 'NONE',  ( 5.253368672218635460, 3.033033817057773529, -4.359491423763652840 ) ) ;
#35029 = ORIENTED_EDGE ( 'NONE', *, *, #11879, .T. ) ;
#35030 = VECTOR ( 'NONE', #21080, 1000.000000000000000 ) ;
#35031 = DIRECTION ( 'NONE',  ( 1.000000000000000000, 0.000000000000000000, 0.000000000000000000 ) ) ;
#35032 = ORIENTED_EDGE ( 'NONE', *, *, #5477, .F. ) ;
#35033 = PLANE ( 'NONE',  #1154 ) ;
#35034 = ORIENTED_EDGE ( 'NONE', *, *, #36344, .F. ) ;
#35035 = EDGE_LOOP ( 'NONE', ( #13863, #35542, #10864 ) ) ;
#35036 = LINE ( 'NONE', #6719, #14635 ) ;
#35037 = ORIENTED_EDGE ( 'NONE', *, *, #1047, .T. ) ;
#35038 =( LENGTH_UNIT ( ) NAMED_UNIT ( * ) SI_UNIT ( .MILLI., .METRE. ) );
#35039 = AXIS2_PLACEMENT_3D ( 'NONE', #20380, #303, #31965 ) ;
#35040 = CIRCLE ( 'NONE', #29645, 2.000000000000000000 ) ;
#35041 = DIRECTION ( 'NONE',  ( 0.000000000000000000, 0.000000000000000000, 1.000000000000000000 ) ) ;
#35042 = EDGE_CURVE ( 'NONE', #23091, #33432, #33747, .T. ) ;
#35043 = CARTESIAN_POINT ( 'NONE',  ( -2.000003374631334818, 69.28203230275516944, 12.50000000000000000 ) ) ;
#35044 = PLANE ( 'NONE',  #19088 ) ;
#35045 = ORIENTED_EDGE ( 'NONE', *, *, #5078, .F. ) ;
#35046 = ORIENTED_EDGE ( 'NONE', *, *, #22881, .T. ) ;
#35047 = ORIENTED_EDGE ( 'NONE', *, *, #36264, .F. ) ;
#35048 = EDGE_CURVE ( 'NONE', #14051, #36367, #33707, .T. ) ;
#35049 = ORIENTED_EDGE ( 'NONE', *, *, #17447, .F. ) ;
#35050 = VERTEX_POINT ( 'NONE', #36187 ) ;
#35052 = CARTESIAN_POINT ( 'NONE',  ( -25.00000337463121980, -77.94228634059963667, -9.999999999999998224 ) ) ;
#35051 = AXIS2_PLACEMENT_3D ( 'NONE', #15683, #10059, #21497 ) ;
#35053 = EDGE_CURVE ( 'NONE', #10733, #35776, #34905, .T. ) ;
#35054 = DIRECTION ( 'NONE',  ( 1.000000000000000000, 0.000000000000000000, 0.000000000000000000 ) ) ;
#35055 = VERTEX_POINT ( 'NONE', #34129 ) ;
#35056 = VECTOR ( 'NONE', #32286, 1000.000000000000000 ) ;
#35057 = EDGE_CURVE ( 'NONE', #9552, #30244, #25140, .T. ) ;
#35058 = CARTESIAN_POINT ( 'NONE',  ( -60.00000337463104216, 34.64101615137757051, 17.49999999999999645 ) ) ;
#35059 = CARTESIAN_POINT ( 'NONE',  ( 79.20400555976016221, 72.31907731944103546, 32.50000000000000000 ) ) ;
#35060 = DIRECTION ( 'NONE',  ( 0.000000000000000000, 0.000000000000000000, 1.000000000000000000 ) ) ;
#35061 = CIRCLE ( 'NONE', #21890, 2.000000000000001776 ) ;
#35062 = ORIENTED_EDGE ( 'NONE', *, *, #23389, .F. ) ;
#35063 = AXIS2_PLACEMENT_3D ( 'NONE', #16275, #30867, #4657 ) ;
#35064 = DIRECTION ( 'NONE',  ( -1.000000000000000000, 0.000000000000000000, 0.000000000000000000 ) ) ;
#35065 = DIRECTION ( 'NONE',  ( 0.000000000000000000, 0.000000000000000000, 1.000000000000000000 ) ) ;
#35066 = DIRECTION ( 'NONE',  ( 1.000000000000000000, 0.000000000000000000, 0.000000000000000000 ) ) ;
#35067 = VERTEX_POINT ( 'NONE', #33575 ) ;
#35068 = DIRECTION ( 'NONE',  ( 0.000000000000000000, 0.000000000000000000, 1.000000000000000000 ) ) ;
#35069 = DIRECTION ( 'NONE',  ( 0.000000000000000000, 0.000000000000000000, 1.000000000000000000 ) ) ;
#35070 = AXIS2_PLACEMENT_3D ( 'NONE', #21499, #18864, #32937 ) ;
#35071 = ORIENTED_EDGE ( 'NONE', *, *, #17370, .F. ) ;
#35072 = VECTOR ( 'NONE', #1633, 1000.000000000000000 ) ;
#35073 = ORIENTED_EDGE ( 'NONE', *, *, #9110, .F. ) ;
#35074 = DIRECTION ( 'NONE',  ( 0.000000000000000000, -1.000000000000000000, 1.034244904716769672E-15 ) ) ;
#35075 = EDGE_CURVE ( 'NONE', #15938, #2053, #30105, .T. ) ;
#35076 = CYLINDRICAL_SURFACE ( 'NONE', #28304, 2.000000000000001776 ) ;
#35077 = DIRECTION ( 'NONE',  ( -1.000000000000000000, 0.000000000000000000, 0.000000000000000000 ) ) ;
#35078 = FACE_OUTER_BOUND ( 'NONE', #9888, .T. ) ;
#35079 = ORIENTED_EDGE ( 'NONE', *, *, #600, .F. ) ;
#35080 = FACE_BOUND ( 'NONE', #32185, .T. ) ;
#35081 = CARTESIAN_POINT ( 'NONE',  ( -33.99999999999999289, 103.4105893997321886, -19.99999999999999645 ) ) ;
#35082 = AXIS2_PLACEMENT_3D ( 'NONE', #11483, #30797, #10933 ) ;
#35083 = ORIENTED_EDGE ( 'NONE', *, *, #15853, .T. ) ;
#35084 = VECTOR ( 'NONE', #11443, 1000.000000000000000 ) ;
#35085 = LINE ( 'NONE', #29267, #27947 ) ;
#35086 = VERTEX_POINT ( 'NONE', #30915 ) ;
#35087 = AXIS2_PLACEMENT_3D ( 'NONE', #34839, #9135, #704 ) ;
#35088 = CIRCLE ( 'NONE', #8138, 2.000000000000001776 ) ;
#35089 = VECTOR ( 'NONE', #1963, 1000.000000000000000 ) ;
#35090 = CARTESIAN_POINT ( 'NONE',  ( -52.39915983220772233, -35.19434990244957362, -4.999999999999997335 ) ) ;
#35091 = AXIS2_PLACEMENT_3D ( 'NONE', #5688, #16777, #30636 ) ;
#35092 = DIRECTION ( 'NONE',  ( -0.000000000000000000, -0.000000000000000000, 1.000000000000000000 ) ) ;
#35093 = CIRCLE ( 'NONE', #6957, 2.500000000000000444 ) ;
#35094 = EDGE_CURVE ( 'NONE', #7314, #13283, #17033, .T. ) ;
#35095 = DIRECTION ( 'NONE',  ( 0.000000000000000000, 0.000000000000000000, 1.000000000000000000 ) ) ;
#35096 = ORIENTED_EDGE ( 'NONE', *, *, #22290, .F. ) ;
#35097 = ADVANCED_FACE ( 'NONE', ( #24752 ), #2606, .F. ) ;
#35098 = ORIENTED_EDGE ( 'NONE', *, *, #7277, .F. ) ;
#35099 = AXIS2_PLACEMENT_3D ( 'NONE', #1823, #10630, #4994 ) ;
#35100 = CARTESIAN_POINT ( 'NONE',  ( -75.00000337463099243, -25.98076211353322051, -9.999999999999998224 ) ) ;
#35101 = CARTESIAN_POINT ( 'NONE',  ( -106.6136999110908476, 41.75147322074028722, 32.50000000000000000 ) ) ;
#35102 = AXIS2_PLACEMENT_3D ( 'NONE', #15712, #1451, #12884 ) ;
#35103 = DIRECTION ( 'NONE',  ( 0.000000000000000000, 0.000000000000000000, 1.000000000000000000 ) ) ;
#35104 = EDGE_CURVE ( 'NONE', #19401, #630, #2576, .T. ) ;
#35105 = ORIENTED_EDGE ( 'NONE', *, *, #18611, .F. ) ;
#35106 = DIRECTION ( 'NONE',  ( 0.000000000000000000, 0.000000000000000000, 1.000000000000000000 ) ) ;
#35107 = CARTESIAN_POINT ( 'NONE',  ( 54.99999662536844625, 60.62177826491077326, -9.999999999999998224 ) ) ;
#35108 = EDGE_CURVE ( 'NONE', #7505, #34871, #2594, .T. ) ;
#35109 = LINE ( 'NONE', #29457, #20830 ) ;
#35110 = CARTESIAN_POINT ( 'NONE',  ( -4.279621169095561228, 62.97617850287782915, -4.999999999999997335 ) ) ;
#35111 = CARTESIAN_POINT ( 'NONE',  ( -2.500000000000000444, 3.061616997868383634E-16, -5.324496230895142901 ) ) ;
#35112 = VERTEX_POINT ( 'NONE', #22480 ) ;
#35113 = CARTESIAN_POINT ( 'NONE',  ( -59.13646009116099833, 70.47608876694653190, -49.22241343995295892 ) ) ;
#35114 = VECTOR ( 'NONE', #32329, 1000.000000000000000 ) ;
#35115 = DIRECTION ( 'NONE',  ( 1.000000000000000000, 0.000000000000000000, 0.000000000000000000 ) ) ;
#35116 = AXIS2_PLACEMENT_3D ( 'NONE', #15005, #12347, #17807 ) ;
#35117 = VERTEX_POINT ( 'NONE', #19315 ) ;
#35118 = DIRECTION ( 'NONE',  ( 1.000000000000000000, 0.000000000000000000, 0.000000000000000000 ) ) ;
#35119 = AXIS2_PLACEMENT_3D ( 'NONE', #19833, #28260, #11197 ) ;
#35120 = LINE ( 'NONE', #34376, #6983 ) ;
#35121 = CARTESIAN_POINT ( 'NONE',  ( -52.39915983220772233, -35.19434990244957362, 12.49999999999999822 ) ) ;
#35122 = CIRCLE ( 'NONE', #28519, 2.000000000000001776 ) ;
#35123 = ADVANCED_FACE ( 'NONE', ( #22305 ), #5252, .F. ) ;
#35124 = AXIS2_PLACEMENT_3D ( 'NONE', #15315, #15132, #26760 ) ;
#35125 = ORIENTED_EDGE ( 'NONE', *, *, #13908, .T. ) ;
#35126 = AXIS2_PLACEMENT_3D ( 'NONE', #14071, #31154, #28155 ) ;
#35127 = EDGE_CURVE ( 'NONE', #9816, #8706, #28333, .T. ) ;
#35128 = VERTEX_POINT ( 'NONE', #27732 ) ;
#35129 = VECTOR ( 'NONE', #25970, 1000.000000000000000 ) ;
#35130 = VERTEX_POINT ( 'NONE', #2046 ) ;
#35131 = EDGE_CURVE ( 'NONE', #11035, #9484, #24765, .T. ) ;
#35132 = EDGE_CURVE ( 'NONE', #5473, #32493, #24165, .T. ) ;
#35133 = CARTESIAN_POINT ( 'NONE',  ( -75.00000337463097821, 43.30127018922197379, -9.999999999999998224 ) ) ;
#35134 = CARTESIAN_POINT ( 'NONE',  ( 0.000000000000000000, 0.000000000000000000, 0.000000000000000000 ) ) ;
#35135 = CARTESIAN_POINT ( 'NONE',  ( -0.7178748134487012988, -5.359037475107207626, -1.327869168827489732 ) ) ;
#35136 = VERTEX_POINT ( 'NONE', #5439 ) ;
#35137 = ORIENTED_EDGE ( 'NONE', *, *, #5978, .F. ) ;
#35138 = EDGE_LOOP ( 'NONE', ( #22475, #8844, #5446, #14420 ) ) ;
#35139 = DIRECTION ( 'NONE',  ( 1.000000000000000000, 0.000000000000000000, 0.000000000000000000 ) ) ;
#35140 = ORIENTED_EDGE ( 'NONE', *, *, #24375, .F. ) ;
#35141 = LINE ( 'NONE', #32312, #6585 ) ;
#35142 = ORIENTED_EDGE ( 'NONE', *, *, #554, .T. ) ;
#35143 = CARTESIAN_POINT ( 'NONE',  ( -22.00000337463124112, -69.28203230275522628, -9.999999999999998224 ) ) ;
#35144 = ORIENTED_EDGE ( 'NONE', *, *, #30468, .T. ) ;
#35145 = VECTOR ( 'NONE', #27800, 1000.000000000000000 ) ;
#35146 = EDGE_LOOP ( 'NONE', ( #12054, #7545, #24042, #26560 ) ) ;
#35147 = FACE_OUTER_BOUND ( 'NONE', #14592, .T. ) ;
#35148 = DIRECTION ( 'NONE',  ( 1.000000000000000000, 0.000000000000000000, 0.000000000000000000 ) ) ;
#35149 = PLANE ( 'NONE',  #12864 ) ;
#35150 = EDGE_LOOP ( 'NONE', ( #22661, #9360, #34126, #30101 ) ) ;
#35151 = EDGE_LOOP ( 'NONE', ( #5455, #26421, #3299 ) ) ;
#35152 = COLOUR_RGB ( '', 0.31764706, 0.68627451, 0.89019608) ;
#35153 = DIRECTION ( 'NONE',  ( 0.000000000000000000, 0.000000000000000000, -1.000000000000000000 ) ) ;
#35154 = CARTESIAN_POINT ( 'NONE',  ( 5.185163620696106257, 2.993655612202505090, -4.330826434870604480 ) ) ;
#35155 = AXIS2_PLACEMENT_3D ( 'NONE', #12679, #4640, #7077 ) ;
#35156 = EDGE_CURVE ( 'NONE', #35412, #18409, #16865, .T. ) ;
#35157 = VECTOR ( 'NONE', #3034, 1000.000000000000000 ) ;
#35158 = CARTESIAN_POINT ( 'NONE',  ( -40.00000337463113453, 69.28203230275516944, -5.000000000000000000 ) ) ;
#35159 = CARTESIAN_POINT ( 'NONE',  ( 4.999996625368676284, -77.94228634059960825, -9.999999999999998224 ) ) ;
#35160 = CIRCLE ( 'NONE', #7017, 2.000000000000001776 ) ;
#35161 = ORIENTED_EDGE ( 'NONE', *, *, #24113, .F. ) ;
#35162 = CARTESIAN_POINT ( 'NONE',  ( 1.999996625368672287, 86.60254037844397601, 17.49999999999999645 ) ) ;
#35163 = FACE_OUTER_BOUND ( 'NONE', #4059, .T. ) ;
#35164 = EDGE_LOOP ( 'NONE', ( #20788, #30605 ) ) ;
#35165 = DIRECTION ( 'NONE',  ( 1.000000000000000000, 0.000000000000000000, 0.000000000000000000 ) ) ;
#35166 = DIRECTION ( 'NONE',  ( 1.000000000000000000, 0.000000000000000000, 0.000000000000000000 ) ) ;
#35167 = CARTESIAN_POINT ( 'NONE',  ( -87.00000337463093558, -8.660254037844422825, -5.000000000000000000 ) ) ;
#35168 = CARTESIAN_POINT ( 'NONE',  ( 0.000000000000000000, -55.00000000000000000, -15.00000000000000000 ) ) ;
#35169 = VECTOR ( 'NONE', #18594, 1000.000000000000000 ) ;
#35170 = DIRECTION ( 'NONE',  ( 1.000000000000000000, 0.000000000000000000, 0.000000000000000000 ) ) ;
#35171 = DIRECTION ( 'NONE',  ( 1.000000000000000000, 0.000000000000000000, 0.000000000000000000 ) ) ;
#35172 = EDGE_LOOP ( 'NONE', ( #17251, #736, #30546, #17007 ) ) ;
#35173 = CYLINDRICAL_SURFACE ( 'NONE', #24385, 150.0000000000000284 ) ;
#35174 = AXIS2_PLACEMENT_3D ( 'NONE', #13613, #33859, #2379 ) ;
#35175 = CARTESIAN_POINT ( 'NONE',  ( 4.817183509279844955, 3.279805190042301533, -4.266911319714219886 ) ) ;
#35176 = CARTESIAN_POINT ( 'NONE',  ( 62.33939050065184517, -13.89091430021398565, 12.49999999999999822 ) ) ;
#35177 = AXIS2_PLACEMENT_3D ( 'NONE', #10438, #33324, #4647 ) ;
#35178 = AXIS2_PLACEMENT_3D ( 'NONE', #4904, #10517, #30754 ) ;
#35179 = ORIENTED_EDGE ( 'NONE', *, *, #2958, .F. ) ;
#35180 = ORIENTED_EDGE ( 'NONE', *, *, #31984, .F. ) ;
#35181 = EDGE_LOOP ( 'NONE', ( #6792, #11414, #29412, #31319 ) ) ;
#35182 = AXIS2_PLACEMENT_3D ( 'NONE', #29514, #27080, #23533 ) ;
#35183 = EDGE_CURVE ( 'NONE', #14697, #18023, #31281, .T. ) ;
#35184 = CARTESIAN_POINT ( 'NONE',  ( 54.99999662536844625, -60.62177826491080168, -5.000000000000000000 ) ) ;
#35185 = CARTESIAN_POINT ( 'NONE',  ( -60.00000337463107059, -34.64101615137762025, -9.999999999999998224 ) ) ;
#35186 = CARTESIAN_POINT ( 'NONE',  ( -1.647413659512548589, 4.822367972110025214, -0.05822226285683017311 ) ) ;
#35187 = CARTESIAN_POINT ( 'NONE',  ( 67.99999662536838230, -17.32050807568879947, -5.000000000000000000 ) ) ;
#35188 = AXIS2_PLACEMENT_3D ( 'NONE', #26157, #22979, #37055 ) ;
#35189 = DIRECTION ( 'NONE',  ( 0.000000000000000000, 0.000000000000000000, 1.000000000000000000 ) ) ;
#35190 = DIRECTION ( 'NONE',  ( -0.000000000000000000, -0.000000000000000000, 1.000000000000000000 ) ) ;
#35191 = VERTEX_POINT ( 'NONE', #13302 ) ;
#35192 = DIRECTION ( 'NONE',  ( 0.000000000000000000, 0.000000000000000000, 1.000000000000000000 ) ) ;
#35193 = ORIENTED_EDGE ( 'NONE', *, *, #1192, .F. ) ;
#35194 = FACE_BOUND ( 'NONE', #27006, .T. ) ;
#35195 = VECTOR ( 'NONE', #17560, 1000.000000000000000 ) ;
#35196 = DIRECTION ( 'NONE',  ( 0.000000000000000000, 0.000000000000000000, 1.000000000000000000 ) ) ;
#35197 = AXIS2_PLACEMENT_3D ( 'NONE', #13631, #25780, #3082 ) ;
#35198 = CARTESIAN_POINT ( 'NONE',  ( -77.93337651276257816, 72.12094976675054170, 32.50001250000000397 ) ) ;
#35199 = ORIENTED_EDGE ( 'NONE', *, *, #7731, .T. ) ;
#35200 = FACE_OUTER_BOUND ( 'NONE', #20463, .T. ) ;
#35201 = CIRCLE ( 'NONE', #7062, 33.00000000000002132 ) ;
#35202 = CIRCLE ( 'NONE', #26779, 3.500000000000003109 ) ;
#35203 = EDGE_CURVE ( 'NONE', #30254, #1072, #5007, .T. ) ;
#35204 = DIRECTION ( 'NONE',  ( 0.1497583224281784364, 0.9887226329277072345, 0.000000000000000000 ) ) ;
#35205 = EDGE_CURVE ( 'NONE', #31374, #6244, #30127, .T. ) ;
#35206 = AXIS2_PLACEMENT_3D ( 'NONE', #31261, #128, #22656 ) ;
#35207 = CARTESIAN_POINT ( 'NONE',  ( 82.99999662536832545, 25.98076211353319565, 17.49999999999999645 ) ) ;
#35208 = CIRCLE ( 'NONE', #23822, 2.000000000000001776 ) ;
#35209 = CYLINDRICAL_SURFACE ( 'NONE', #14956, 3.499999999999989342 ) ;
#35210 = CARTESIAN_POINT ( 'NONE',  ( -65.00000337463106348, -60.62177826491083010, -9.999999999999998224 ) ) ;
#35211 = VERTEX_POINT ( 'NONE', #35028 ) ;
#35212 = B_SPLINE_CURVE_WITH_KNOTS ( 'NONE', 3,
 ( #17706, #34247, #20508, #31590, #5929, #13972 ),
 .UNSPECIFIED., .F., .F.,
 ( 4, 2, 4 ),
 ( 0.000000000000000000, 0.001529397995383628651, 0.003058795990767257302 ),
 .UNSPECIFIED. ) ;
#35213 = DIRECTION ( 'NONE',  ( 1.000000000000000000, 0.000000000000000000, 0.000000000000000000 ) ) ;
#35214 = CARTESIAN_POINT ( 'NONE',  ( -6.000000000000000000, 149.8799519615616305, 32.50000000000000000 ) ) ;
#35215 = CARTESIAN_POINT ( 'NONE',  ( 6.000000000000000000, -149.8799519615616305, 32.50000000000000000 ) ) ;
#35216 = VECTOR ( 'NONE', #20868, 1000.000000000000000 ) ;
#35217 = EDGE_LOOP ( 'NONE', ( #3412, #21091, #20448, #16272, #7619, #28240, #15516, #7956, #14087, #29960, #22500, #25148, #11920 ) ) ;
#35218 = CIRCLE ( 'NONE', #23210, 33.00000000000001421 ) ;
#35219 = EDGE_CURVE ( 'NONE', #17144, #19856, #23228, .T. ) ;
#35220 = ORIENTED_EDGE ( 'NONE', *, *, #34102, .F. ) ;
#35221 = ORIENTED_EDGE ( 'NONE', *, *, #35492, .F. ) ;
#35222 = CARTESIAN_POINT ( 'NONE',  ( 77.93343913441647430, -72.12058696850856165, 27.50000000000000000 ) ) ;
#35223 = CARTESIAN_POINT ( 'NONE',  ( -23.49154088336464952, -103.5526315789473699, 32.50002500000000083 ) ) ;
#35224 = CARTESIAN_POINT ( 'NONE',  ( 56.52018970185260116, -35.83991598322081273, -4.999999999999997335 ) ) ;
#35225 = AXIS2_PLACEMENT_3D ( 'NONE', #11301, #22750, #33627 ) ;
#35226 = ADVANCED_FACE ( 'NONE', ( #20404 ), #17972, .F. ) ;
#35227 = DIRECTION ( 'NONE',  ( 0.000000000000000000, 0.000000000000000000, 1.000000000000000000 ) ) ;
#35228 = DIRECTION ( 'NONE',  ( 0.000000000000000000, 0.000000000000000000, 1.000000000000000000 ) ) ;
#35229 = AXIS2_PLACEMENT_3D ( 'NONE', #15668, #4411, #12257 ) ;
#35230 = AXIS2_PLACEMENT_3D ( 'NONE', #21407, #21602, #24210 ) ;
#35231 = DIRECTION ( 'NONE',  ( 0.000000000000000000, 0.000000000000000000, 1.000000000000000000 ) ) ;
#35232 = ORIENTED_EDGE ( 'NONE', *, *, #34648, .F. ) ;
#35233 = CIRCLE ( 'NONE', #37022, 2.000000000000001776 ) ;
#35234 = ORIENTED_EDGE ( 'NONE', *, *, #18065, .F. ) ;
#35235 = DIRECTION ( 'NONE',  ( 0.000000000000000000, 0.000000000000000000, 1.000000000000000000 ) ) ;
#35236 = VECTOR ( 'NONE', #19720, 1000.000000000000000 ) ;
#35237 = DIRECTION ( 'NONE',  ( -0.8660254037844449249, -0.4999999999999888978, 0.000000000000000000 ) ) ;
#35238 = VERTEX_POINT ( 'NONE', #23415 ) ;
#35239 = CARTESIAN_POINT ( 'NONE',  ( -4.319324222803747837, -3.279739689143278181, -3.838711833383472438 ) ) ;
#35240 = VERTEX_POINT ( 'NONE', #6152 ) ;
#35241 = AXIS2_PLACEMENT_3D ( 'NONE', #30169, #21572, #32998 ) ;
#35242 = FACE_BOUND ( 'NONE', #20953, .T. ) ;
#35243 = ORIENTED_EDGE ( 'NONE', *, *, #9288, .F. ) ;
#35244 = VERTEX_POINT ( 'NONE', #2802 ) ;
#35245 = EDGE_CURVE ( 'NONE', #12872, #26254, #17549, .T. ) ;
#35246 = CARTESIAN_POINT ( 'NONE',  ( 4.242640687119251908, -4.242640687119325626, 32.50000000000000000 ) ) ;
#35247 = EDGE_LOOP ( 'NONE', ( #7920, #5424, #26650, #10105 ) ) ;
#35248 = AXIS2_PLACEMENT_3D ( 'NONE', #16462, #30887, #27893 ) ;
#35249 = SURFACE_SIDE_STYLE ('',( #32583 ) ) ;
#35250 = PRODUCT_DEFINITION_SHAPE ( 'NONE', 'NONE',  #37120 ) ;
#35251 = CARTESIAN_POINT ( 'NONE',  ( -42.97377950131527058, 96.90768712682508124, -19.99999999999999645 ) ) ;
#35252 = VECTOR ( 'NONE', #20585, 1000.000000000000000 ) ;
#35253 = CARTESIAN_POINT ( 'NONE',  ( 145.0000000000000568, -5.056524707326808249E-13, 27.50000000000000000 ) ) ;
#35254 = LINE ( 'NONE', #32410, #36481 ) ;
#35255 = ORIENTED_EDGE ( 'NONE', *, *, #27718, .T. ) ;
#35256 = ORIENTED_EDGE ( 'NONE', *, *, #31274, .F. ) ;
#35257 = ADVANCED_FACE ( 'NONE', ( #146 ), #28663, .F. ) ;
#35258 = VECTOR ( 'NONE', #15174, 1000.000000000000000 ) ;
#35259 = ORIENTED_EDGE ( 'NONE', *, *, #155, .F. ) ;
#35260 = ORIENTED_EDGE ( 'NONE', *, *, #28573, .F. ) ;
#35261 = EDGE_CURVE ( 'NONE', #10755, #2344, #12746, .T. ) ;
#35262 = AXIS2_PLACEMENT_3D ( 'NONE', #31986, #35227, #32390 ) ;
#35263 = VERTEX_POINT ( 'NONE', #34295 ) ;
#35264 = CARTESIAN_POINT ( 'NONE',  ( -65.00000337463106348, -60.62177826491083010, 12.50000000000000000 ) ) ;
#35265 = CARTESIAN_POINT ( 'NONE',  ( -30.89873480577614018, 67.49533652152319974, -5.000000000000000000 ) ) ;
#35266 = ORIENTED_EDGE ( 'NONE', *, *, #4165, .F. ) ;
#35267 = DIRECTION ( 'NONE',  ( -1.000000000000000000, 0.000000000000000000, 0.000000000000000000 ) ) ;
#35268 = CARTESIAN_POINT ( 'NONE',  ( 104.0325470118518751, 35.06873771483363100, 32.49999999999999289 ) ) ;
#35269 = CARTESIAN_POINT ( 'NONE',  ( -55.00000337463109901, -60.62177826491083010, 12.50000000000000000 ) ) ;
#35270 = AXIS2_PLACEMENT_3D ( 'NONE', #8470, #6195, #16906 ) ;
#35271 = ORIENTED_EDGE ( 'NONE', *, *, #29672, .T. ) ;
#35272 = CYLINDRICAL_SURFACE ( 'NONE', #8077, 5.750000000000002665 ) ;
#35273 = VECTOR ( 'NONE', #8323, 1000.000000000000000 ) ;
#35274 = DIRECTION ( 'NONE',  ( 0.000000000000000000, 0.000000000000000000, 1.000000000000000000 ) ) ;
#35275 = CARTESIAN_POINT ( 'NONE',  ( 7.041719095097282852E-16, 78.44802294027068967, -24.99999999999999645 ) ) ;
#35276 = VERTEX_POINT ( 'NONE', #17416 ) ;
#35277 = CARTESIAN_POINT ( 'NONE',  ( -85.00000337463092137, 8.660254037844389075, -9.999999999999998224 ) ) ;
#35278 = CARTESIAN_POINT ( 'NONE',  ( -22.00000337463124112, -69.28203230275522628, -9.999999999999998224 ) ) ;
#35279 = VERTEX_POINT ( 'NONE', #17582 ) ;
#35280 = VERTEX_POINT ( 'NONE', #3157 ) ;
#35281 = EDGE_CURVE ( 'NONE', #29968, #13826, #31655, .T. ) ;
#35282 = LINE ( 'NONE', #32250, #5085 ) ;
#35283 = AXIS2_PLACEMENT_3D ( 'NONE', #33718, #24726, #25282 ) ;
#35284 = CARTESIAN_POINT ( 'NONE',  ( -72.00000337463100664, 34.64101615137758472, -5.000000000000000000 ) ) ;
#35285 = CYLINDRICAL_SURFACE ( 'NONE', #9060, 2.000000000000001776 ) ;
#35286 = FACE_OUTER_BOUND ( 'NONE', #10392, .T. ) ;
#35287 = VERTEX_POINT ( 'NONE', #22860 ) ;
#35288 = AXIS2_PLACEMENT_3D ( 'NONE', #3265, #29324, #17695 ) ;
#35289 = ADVANCED_FACE ( 'NONE', ( #29008 ), #2994, .T. ) ;
#35290 = FACE_BOUND ( 'NONE', #34255, .T. ) ;
#35291 = DIRECTION ( 'NONE',  ( -0.000000000000000000, -0.000000000000000000, -1.000000000000000000 ) ) ;
#35292 = ORIENTED_EDGE ( 'NONE', *, *, #21431, .F. ) ;
#35293 = AXIS2_PLACEMENT_3D ( 'NONE', #34941, #14134, #19949 ) ;
#35294 = EDGE_CURVE ( 'NONE', #5247, #26842, #23551, .T. ) ;
#35295 = DIRECTION ( 'NONE',  ( 1.000000000000000000, 0.000000000000000000, 0.000000000000000000 ) ) ;
#35296 = EDGE_LOOP ( 'NONE', ( #19973, #12186 ) ) ;
#35297 = AXIS2_PLACEMENT_3D ( 'NONE', #9333, #23784, #3343 ) ;
#35298 = DIRECTION ( 'NONE',  ( 0.000000000000000000, 0.000000000000000000, 1.000000000000000000 ) ) ;
#35299 = CARTESIAN_POINT ( 'NONE',  ( -56.13646009116099123, 70.47608876694653190, -4.999999999999997335 ) ) ;
#35300 = VECTOR ( 'NONE', #23196, 1000.000000000000000 ) ;
#35301 = DIRECTION ( 'NONE',  ( 0.000000000000000000, 0.000000000000000000, 1.000000000000000000 ) ) ;
#35302 = EDGE_LOOP ( 'NONE', ( #14372, #18161, #22284, #23250 ) ) ;
#35303 = CIRCLE ( 'NONE', #23325, 1.999999999999998224 ) ;
#35304 = ORIENTED_EDGE ( 'NONE', *, *, #5477, .T. ) ;
#35305 = DIRECTION ( 'NONE',  ( -1.000000000000000000, 0.000000000000000000, 0.000000000000000000 ) ) ;
#35306 = EDGE_CURVE ( 'NONE', #10807, #11432, #12143, .T. ) ;
#35307 = ORIENTED_EDGE ( 'NONE', *, *, #1528, .T. ) ;
#35308 = DIRECTION ( 'NONE',  ( 0.000000000000000000, 0.000000000000000000, 1.000000000000000000 ) ) ;
#35309 = CIRCLE ( 'NONE', #26915, 3.500000000000003109 ) ;
#35310 = DIRECTION ( 'NONE',  ( 1.000000000000000000, 0.000000000000000000, 0.000000000000000000 ) ) ;
#35311 = AXIS2_PLACEMENT_3D ( 'NONE', #24159, #34864, #35610 ) ;
#35312 = CARTESIAN_POINT ( 'NONE',  ( -50.00000337463109190, 69.28203230275518365, -9.999999999999998224 ) ) ;
#35313 = CARTESIAN_POINT ( 'NONE',  ( 3.000000000000000000, 2.935248768560057453, -3.903127820947815962E-15 ) ) ;
#35314 = CYLINDRICAL_SURFACE ( 'NONE', #6347, 2.000000000000001776 ) ;
#35315 = ORIENTED_EDGE ( 'NONE', *, *, #29334, .F. ) ;
#35316 = FACE_OUTER_BOUND ( 'NONE', #25312, .T. ) ;
#35317 = CARTESIAN_POINT ( 'NONE',  ( 0.000000000000000000, 0.000000000000000000, 5.000000000000000000 ) ) ;
#35318 = DIRECTION ( 'NONE',  ( -0.000000000000000000, -0.000000000000000000, 1.000000000000000000 ) ) ;
#35319 = VERTEX_POINT ( 'NONE', #14233 ) ;
#35320 = DIRECTION ( 'NONE',  ( 0.000000000000000000, 0.000000000000000000, 1.000000000000000000 ) ) ;
#35321 = DIRECTION ( 'NONE',  ( -0.7650473262243665529, 0.6439740589782693148, 0.000000000000000000 ) ) ;
#35322 = CARTESIAN_POINT ( 'NONE',  ( 0.000000000000000000, 0.000000000000000000, -6.000000000000000000 ) ) ;
#35323 = AXIS2_PLACEMENT_3D ( 'NONE', #26370, #3298, #676 ) ;
#35324 = ORIENTED_EDGE ( 'NONE', *, *, #17662, .F. ) ;
#35325 = ORIENTED_EDGE ( 'NONE', *, *, #16130, .F. ) ;
#35326 = VECTOR ( 'NONE', #13042, 999.9999999999998863 ) ;
#35327 = ADVANCED_FACE ( 'NONE', ( #8598 ), #11962, .F. ) ;
#35328 = CARTESIAN_POINT ( 'NONE',  ( -13.00000337463125710, -77.94228634059960825, 12.50000000000000000 ) ) ;
#35329 = DIRECTION ( 'NONE',  ( 0.000000000000000000, 0.000000000000000000, 1.000000000000000000 ) ) ;
#35330 = EDGE_CURVE ( 'NONE', #35136, #2553, #11565, .T. ) ;
#35331 = CYLINDRICAL_SURFACE ( 'NONE', #7058, 2.000000000000000000 ) ;
#35332 = ORIENTED_EDGE ( 'NONE', *, *, #32457, .F. ) ;
#35333 = ORIENTED_EDGE ( 'NONE', *, *, #2470, .T. ) ;
#35334 = CIRCLE ( 'NONE', #3596, 6.000000000000005329 ) ;
#35335 = ORIENTED_EDGE ( 'NONE', *, *, #10615, .F. ) ;
#35336 = ADVANCED_FACE ( 'NONE', ( #34848 ), #9142, .T. ) ;
#35337 = DIRECTION ( 'NONE',  ( 1.000000000000000000, 0.000000000000000000, 0.000000000000000000 ) ) ;
#35338 = AXIS2_PLACEMENT_3D ( 'NONE', #25072, #33505, #10806 ) ;
#35339 = ORIENTED_EDGE ( 'NONE', *, *, #33702, .T. ) ;
#35340 = CARTESIAN_POINT ( 'NONE',  ( 9.904614206369521057, -117.9630559560052632, 32.49999999999999289 ) ) ;
#35342 = EDGE_CURVE ( 'NONE', #34186, #35276, #15167, .T. ) ;
#35341 = EDGE_LOOP ( 'NONE', ( #20711, #35503 ) ) ;
#35343 = CIRCLE ( 'NONE', #23335, 2.000000000000001776 ) ;
#35344 = DIRECTION ( 'NONE',  ( 0.000000000000000000, 0.000000000000000000, 1.000000000000000000 ) ) ;
#35345 = EDGE_LOOP ( 'NONE', ( #27574, #1804 ) ) ;
#35346 = ADVANCED_FACE ( 'NONE', ( #710 ), #12120, .F. ) ;
#35347 = ORIENTED_EDGE ( 'NONE', *, *, #21976, .T. ) ;
#35348 =( NAMED_UNIT ( * ) SI_UNIT ( $, .STERADIAN. ) SOLID_ANGLE_UNIT ( ) );
#35349 = CARTESIAN_POINT ( 'NONE',  ( 0.000000000000000000, 0.000000000000000000, -5.000000000000000000 ) ) ;
#35350 = DIRECTION ( 'NONE',  ( 1.000000000000000000, 0.000000000000000000, 0.000000000000000000 ) ) ;
#35351 = ORIENTED_EDGE ( 'NONE', *, *, #16523, .T. ) ;
#35352 = ORIENTED_EDGE ( 'NONE', *, *, #21621, .T. ) ;
#35353 = DIRECTION ( 'NONE',  ( 1.000000000000000000, 0.000000000000000000, 0.000000000000000000 ) ) ;
#35354 = CARTESIAN_POINT ( 'NONE',  ( 4.999999999999999112, 2.886751345948126879, -4.069522543421416394 ) ) ;
#35355 = VECTOR ( 'NONE', #18102, 1000.000000000000000 ) ;
#35356 = EDGE_CURVE ( 'NONE', #25432, #26711, #36142, .T. ) ;
#35357 = FACE_OUTER_BOUND ( 'NONE', #10363, .T. ) ;
#35358 = ADVANCED_FACE ( 'NONE', ( #9890 ), #21328, .T. ) ;
#35359 = DIRECTION ( 'NONE',  ( -0.000000000000000000, -0.000000000000000000, 1.000000000000000000 ) ) ;
#35360 = EDGE_CURVE ( 'NONE', #21285, #11174, #32533, .T. ) ;
#35361 = ORIENTED_EDGE ( 'NONE', *, *, #7290, .F. ) ;
#35362 = DIRECTION ( 'NONE',  ( 0.000000000000000000, 0.000000000000000000, 1.000000000000000000 ) ) ;
#35363 = CARTESIAN_POINT ( 'NONE',  ( -47.63139720814438505, -27.49999999999955591, -10.00000000000000178 ) ) ;
#35364 = EDGE_CURVE ( 'NONE', #18749, #7366, #36726, .T. ) ;
#35365 = ORIENTED_EDGE ( 'NONE', *, *, #22406, .F. ) ;
#35366 = CIRCLE ( 'NONE', #30549, 3.000000000000000888 ) ;
#35367 = PLANE ( 'NONE',  #2405 ) ;
#35368 = EDGE_CURVE ( 'NONE', #36249, #7111, #6786, .T. ) ;
#35369 = CARTESIAN_POINT ( 'NONE',  ( 36.99999662536855283, -60.62177826491080168, -9.999999999999998224 ) ) ;
#35370 = AXIS2_PLACEMENT_3D ( 'NONE', #3371, #359, #29238 ) ;
#35371 = DIRECTION ( 'NONE',  ( 1.000000000000000000, 0.000000000000000000, 0.000000000000000000 ) ) ;
#35372 = FACE_OUTER_BOUND ( 'NONE', #19372, .T. ) ;
#35373 = CYLINDRICAL_SURFACE ( 'NONE', #17914, 2.000000000000000000 ) ;
#35374 = CIRCLE ( 'NONE', #19193, 2.000000000000001776 ) ;
#35375 = CARTESIAN_POINT ( 'NONE',  ( 5.000000000000000000, 2.886751345948134428, -2.080000000000000071 ) ) ;
#35376 = EDGE_LOOP ( 'NONE', ( #35837, #10015 ) ) ;
#35377 = DIRECTION ( 'NONE',  ( -0.000000000000000000, -0.000000000000000000, 1.000000000000000000 ) ) ;
#35378 = AXIS2_PLACEMENT_3D ( 'NONE', #30299, #21858, #1813 ) ;
#35379 = DIRECTION ( 'NONE',  ( -1.000000000000000000, -0.000000000000000000, -0.000000000000000000 ) ) ;
#35380 = CARTESIAN_POINT ( 'NONE',  ( 54.99999662536844625, 60.62177826491077326, 12.50000000000000000 ) ) ;
#35381 = ORIENTED_EDGE ( 'NONE', *, *, #22571, .T. ) ;
#35382 = ORIENTED_EDGE ( 'NONE', *, *, #20366, .F. ) ;
#35383 = ORIENTED_EDGE ( 'NONE', *, *, #3231, .F. ) ;
#35384 = DIRECTION ( 'NONE',  ( 0.000000000000000000, 0.000000000000000000, 1.000000000000000000 ) ) ;
#35385 = DIRECTION ( 'NONE',  ( 0.000000000000000000, 0.000000000000000000, 1.000000000000000000 ) ) ;
#35386 = AXIS2_PLACEMENT_3D ( 'NONE', #26666, #981, #17668 ) ;
#35387 = DIRECTION ( 'NONE',  ( -0.000000000000000000, -0.000000000000000000, -1.000000000000000000 ) ) ;
#35388 = DIRECTION ( 'NONE',  ( 1.000000000000000000, 0.000000000000000000, 0.000000000000000000 ) ) ;
#35389 = DIRECTION ( 'NONE',  ( 1.000000000000000000, 0.000000000000000000, 0.000000000000000000 ) ) ;
#35390 = ORIENTED_EDGE ( 'NONE', *, *, #9835, .F. ) ;
#35391 = AXIS2_PLACEMENT_3D ( 'NONE', #4912, #14815, #20065 ) ;
#35392 = CARTESIAN_POINT ( 'NONE',  ( 49.99999662536846756, 69.28203230275516944, 12.50000000000000000 ) ) ;
#35393 = VERTEX_POINT ( 'NONE', #1271 ) ;
#35395 = AXIS2_PLACEMENT_3D ( 'NONE', #15919, #21725, #7481 ) ;
#35394 = FACE_BOUND ( 'NONE', #10421, .T. ) ;
#35396 = FACE_OUTER_BOUND ( 'NONE', #2195, .T. ) ;
#35397 = CARTESIAN_POINT ( 'NONE',  ( 52.99999662536846046, -43.30127018922200222, -9.999999999999998224 ) ) ;
#35398 = CARTESIAN_POINT ( 'NONE',  ( 54.99999662536844625, -60.62177826491080168, 12.50000000000000000 ) ) ;
#35399 = ORIENTED_EDGE ( 'NONE', *, *, #16332, .F. ) ;
#35400 = DIRECTION ( 'NONE',  ( 0.000000000000000000, 0.000000000000000000, 1.000000000000000000 ) ) ;
#35401 = CARTESIAN_POINT ( 'NONE',  ( -65.00000337463106348, -60.62177826491083010, 17.49999999999999645 ) ) ;
#35402 = DIRECTION ( 'NONE',  ( 0.000000000000000000, -0.000000000000000000, -1.000000000000000000 ) ) ;
#35403 = CARTESIAN_POINT ( 'NONE',  ( 49.99999662536846756, -69.28203230275519786, -5.000000000000000000 ) ) ;
#35404 = EDGE_CURVE ( 'NONE', #28909, #19957, #22349, .T. ) ;
#35405 = ORIENTED_EDGE ( 'NONE', *, *, #2676, .T. ) ;
#35406 = DIRECTION ( 'NONE',  ( 1.000000000000000000, 0.000000000000000000, 0.000000000000000000 ) ) ;
#35407 = DIRECTION ( 'NONE',  ( 0.000000000000000000, 0.000000000000000000, -1.000000000000000000 ) ) ;
#35408 = LINE ( 'NONE', #29940, #30931 ) ;
#35409 = VERTEX_POINT ( 'NONE', #18710 ) ;
#35410 = ORIENTED_EDGE ( 'NONE', *, *, #8603, .T. ) ;
#35411 = AXIS2_PLACEMENT_3D ( 'NONE', #36559, #22463, #16475 ) ;
#35412 = VERTEX_POINT ( 'NONE', #4280 ) ;
#35413 = DIRECTION ( 'NONE',  ( 1.000000000000000000, 0.000000000000000000, 0.000000000000000000 ) ) ;
#35414 = CARTESIAN_POINT ( 'NONE',  ( 57.99999662536842493, 51.96152422706639129, 17.49999999999999645 ) ) ;
#35415 = DIRECTION ( 'NONE',  ( 0.000000000000000000, 0.000000000000000000, 1.000000000000000000 ) ) ;
#35416 = DIRECTION ( 'NONE',  ( 0.000000000000000000, 0.000000000000000000, -1.000000000000000000 ) ) ;
#35417 = DIRECTION ( 'NONE',  ( 0.8660254037844344888, -0.5000000000000071054, 0.000000000000000000 ) ) ;
#35418 = DIRECTION ( 'NONE',  ( 1.000000000000000000, 0.000000000000000000, 0.000000000000000000 ) ) ;
#35419 = EDGE_CURVE ( 'NONE', #26119, #26245, #199, .T. ) ;
#35420 = ORIENTED_EDGE ( 'NONE', *, *, #37020, .F. ) ;
#35421 = EDGE_LOOP ( 'NONE', ( #19103, #21684, #7840, #28471 ) ) ;
#35422 = CARTESIAN_POINT ( 'NONE',  ( 64.99999662536839651, 60.62177826491078747, 12.50000000000000000 ) ) ;
#35423 = CARTESIAN_POINT ( 'NONE',  ( -2.000003374631303732, -86.60254037844400443, -9.999999999999998224 ) ) ;
#35424 = EDGE_LOOP ( 'NONE', ( #21531, #28282 ) ) ;
#35425 = CYLINDRICAL_SURFACE ( 'NONE', #37082, 2.000000000000001776 ) ;
#35426 = EDGE_LOOP ( 'NONE', ( #7177, #34719, #740, #10983 ) ) ;
#35427 = CARTESIAN_POINT ( 'NONE',  ( 56.99999662536846046, -43.30127018922200222, -9.999999999999998224 ) ) ;
#35428 = ORIENTED_EDGE ( 'NONE', *, *, #10600, .F. ) ;
#35429 = ORIENTED_EDGE ( 'NONE', *, *, #14933, .T. ) ;
#35430 = DIRECTION ( 'NONE',  ( 0.7071067811865536790, 0.7071067811865414665, 0.000000000000000000 ) ) ;
#35431 = ORIENTED_EDGE ( 'NONE', *, *, #23717, .T. ) ;
#35432 =( NAMED_UNIT ( * ) SI_UNIT ( $, .STERADIAN. ) SOLID_ANGLE_UNIT ( ) );
#35433 = DIRECTION ( 'NONE',  ( 1.000000000000000000, 0.000000000000000000, 0.000000000000000000 ) ) ;
#35434 = DIRECTION ( 'NONE',  ( 0.000000000000000000, 0.000000000000000000, 1.000000000000000000 ) ) ;
#35435 = DIRECTION ( 'NONE',  ( -1.000000000000000000, 0.000000000000000000, 0.000000000000000000 ) ) ;
#35436 = ADVANCED_FACE ( 'NONE', ( #3889 ), #26578, .T. ) ;
#35437 = EDGE_LOOP ( 'NONE', ( #22976, #16433, #17782, #10749 ) ) ;
#35438 = EDGE_LOOP ( 'NONE', ( #9642, #28411, #15732, #19730 ) ) ;
#35439 = ORIENTED_EDGE ( 'NONE', *, *, #19763, .T. ) ;
#35440 = SHAPE_REPRESENTATION ( 'torque nut 03_iso_ISO 7042-M6-N', ( #21385 ), #33942 ) ;
#35441 = VERTEX_POINT ( 'NONE', #24338 ) ;
#35442 = VERTEX_POINT ( 'NONE', #35423 ) ;
#35443 = CARTESIAN_POINT ( 'NONE',  ( 0.000000000000000000, 0.000000000000000000, -5.000000000000000000 ) ) ;
#35444 = AXIS2_PLACEMENT_3D ( 'NONE', #31579, #3097, #19967 ) ;
#35445 = CARTESIAN_POINT ( 'NONE',  ( 69.99999662536839651, -3.469446951953614189E-15, 12.50000000000000000 ) ) ;
#35446 = ORIENTED_EDGE ( 'NONE', *, *, #33150, .T. ) ;
#35447 = CIRCLE ( 'NONE', #28253, 2.000000000000001776 ) ;
#35448 = LINE ( 'NONE', #3919, #4715 ) ;
#35449 = CARTESIAN_POINT ( 'NONE',  ( 64.99999662536839651, -43.30127018922199511, 12.50000000000000000 ) ) ;
#35450 = DIRECTION ( 'NONE',  ( 0.000000000000000000, 0.000000000000000000, 1.000000000000000000 ) ) ;
#35451 = VERTEX_POINT ( 'NONE', #12690 ) ;
#35452 = DIRECTION ( 'NONE',  ( 0.000000000000000000, 0.000000000000000000, 1.000000000000000000 ) ) ;
#35453 = CARTESIAN_POINT ( 'NONE',  ( -5.204170427930421283E-15, 5.773502691896269745, -0.5999999999999998668 ) ) ;
#35454 = EDGE_CURVE ( 'NONE', #16972, #11035, #35561, .T. ) ;
#35455 = DIRECTION ( 'NONE',  ( 0.000000000000000000, 0.000000000000000000, 1.000000000000000000 ) ) ;
#35456 = EDGE_LOOP ( 'NONE', ( #11834, #14539, #17579, #15373, #24099 ) ) ;
#35457 = DIRECTION ( 'NONE',  ( 0.000000000000000000, 0.000000000000000000, 1.000000000000000000 ) ) ;
#35458 = DIRECTION ( 'NONE',  ( -0.000000000000000000, -0.000000000000000000, 1.000000000000000000 ) ) ;
#35459 = EDGE_CURVE ( 'NONE', #4910, #10671, #31900, .T. ) ;
#35460 = ORIENTED_EDGE ( 'NONE', *, *, #25866, .F. ) ;
#35461 = EDGE_LOOP ( 'NONE', ( #31639, #2622, #16102, #35049 ) ) ;
#35462 = DIRECTION ( 'NONE',  ( 1.000000000000000000, 0.000000000000000000, 0.000000000000000000 ) ) ;
#35463 = DIRECTION ( 'NONE',  ( 0.000000000000000000, 0.000000000000000000, -1.000000000000000000 ) ) ;
#35464 = PLANE ( 'NONE',  #19852 ) ;
#35465 = EDGE_CURVE ( 'NONE', #18462, #8511, #4397, .T. ) ;
#35466 = ORIENTED_EDGE ( 'NONE', *, *, #18603, .F. ) ;
#35467 = CARTESIAN_POINT ( 'NONE',  ( 43.19957991610432657, 47.04203867989531318, 12.49999999999999822 ) ) ;
#35468 = CARTESIAN_POINT ( 'NONE',  ( -75.00000337463097821, -8.660254037844422825, -9.999999999999998224 ) ) ;
#35469 = EDGE_CURVE ( 'NONE', #1395, #12727, #34451, .T. ) ;
#35470 = ORIENTED_EDGE ( 'NONE', *, *, #24733, .F. ) ;
#35471 = AXIS2_PLACEMENT_3D ( 'NONE', #26852, #12588, #17654 ) ;
#35472 = PLANE ( 'NONE',  #14191 ) ;
#35473 = ORIENTED_EDGE ( 'NONE', *, *, #10536, .F. ) ;
#35474 = CARTESIAN_POINT ( 'NONE',  ( 27.78182860042856461, 56.67878100130339902, 12.49999999999999822 ) ) ;
#35475 = CARTESIAN_POINT ( 'NONE',  ( 4.279621169095998212, -62.97617850287780072, -4.999999999999997335 ) ) ;
#35476 = LINE ( 'NONE', #15594, #34662 ) ;
#35477 = ORIENTED_EDGE ( 'NONE', *, *, #21533, .T. ) ;
#35478 = VERTEX_POINT ( 'NONE', #32396 ) ;
#35479 = EDGE_CURVE ( 'NONE', #28847, #31817, #15277, .T. ) ;
#35480 = CIRCLE ( 'NONE', #18716, 2.000000000000001776 ) ;
#35481 = VERTEX_POINT ( 'NONE', #15531 ) ;
#35482 = DIRECTION ( 'NONE',  ( 0.000000000000000000, 0.000000000000000000, -1.000000000000000000 ) ) ;
#35483 = DIRECTION ( 'NONE',  ( 0.000000000000000000, 0.000000000000000000, 1.000000000000000000 ) ) ;
#35484 = DIRECTION ( 'NONE',  ( 1.000000000000000000, 0.000000000000000000, 0.000000000000000000 ) ) ;
#35485 = CARTESIAN_POINT ( 'NONE',  ( 9.999996625368655856, -69.28203230275519786, -5.000000000000000000 ) ) ;
#35486 = CARTESIAN_POINT ( 'NONE',  ( -50.00000337463109190, 51.96152422706637708, -9.999999999999998224 ) ) ;
#35487 = ORIENTED_EDGE ( 'NONE', *, *, #7349, .F. ) ;
#35488 = CARTESIAN_POINT ( 'NONE',  ( -37.00000337463117717, -77.94228634059963667, -9.999999999999998224 ) ) ;
#35489 = EDGE_CURVE ( 'NONE', #9206, #12265, #27849, .T. ) ;
#35490 = DIRECTION ( 'NONE',  ( -0.000000000000000000, -0.000000000000000000, -1.000000000000000000 ) ) ;
#35491 = CIRCLE ( 'NONE', #25313, 2.000000000000001776 ) ;
#35492 = EDGE_CURVE ( 'NONE', #33065, #374, #3895, .T. ) ;
#35493 = DIRECTION ( 'NONE',  ( 1.000000000000000000, 0.000000000000000000, 0.000000000000000000 ) ) ;
#35494 = ORIENTED_EDGE ( 'NONE', *, *, #8729, .T. ) ;
#35495 = PLANE ( 'NONE',  #15441 ) ;
#35496 = DIRECTION ( 'NONE',  ( 1.000000000000000000, 0.000000000000000000, 0.000000000000000000 ) ) ;
#35497 = CYLINDRICAL_SURFACE ( 'NONE', #35386, 2.000000000000001776 ) ;
#35498 = EDGE_LOOP ( 'NONE', ( #12646, #10942, #34316, #23145 ) ) ;
#35499 = ORIENTED_EDGE ( 'NONE', *, *, #10042, .F. ) ;
#35500 = DIRECTION ( 'NONE',  ( -1.000000000000000000, 0.000000000000000000, 0.000000000000000000 ) ) ;
#35501 = CYLINDRICAL_SURFACE ( 'NONE', #14573, 2.000000000000001776 ) ;
#35502 = CYLINDRICAL_SURFACE ( 'NONE', #34023, 95.00000000000001421 ) ;
#35503 = ORIENTED_EDGE ( 'NONE', *, *, #11592, .F. ) ;
#35504 = ORIENTED_EDGE ( 'NONE', *, *, #24056, .F. ) ;
#35505 = VERTEX_POINT ( 'NONE', #1447 ) ;
#35506 = CARTESIAN_POINT ( 'NONE',  ( 74.99999662536835388, -25.98076211353319565, 12.50000000000000000 ) ) ;
#35507 = EDGE_CURVE ( 'NONE', #33684, #8634, #5700, .T. ) ;
#35508 = ORIENTED_EDGE ( 'NONE', *, *, #14570, .T. ) ;
#35509 = ORIENTED_EDGE ( 'NONE', *, *, #3107, .T. ) ;
#35510 = CARTESIAN_POINT ( 'NONE',  ( -70.00000337463099243, 51.96152422706637708, -5.000000000000000000 ) ) ;
#35511 = ORIENTED_EDGE ( 'NONE', *, *, #4185, .F. ) ;
#35512 = VERTEX_POINT ( 'NONE', #29564 ) ;
#35513 = CIRCLE ( 'NONE', #13948, 2.000000000000000000 ) ;
#35514 = CARTESIAN_POINT ( 'NONE',  ( 51.13139720814400846, -27.50000000000022737, 5.000000000000000888 ) ) ;
#35515 = ORIENTED_EDGE ( 'NONE', *, *, #9869, .F. ) ;
#35516 = CIRCLE ( 'NONE', #24728, 5.000000000000000000 ) ;
#35517 = ORIENTED_EDGE ( 'NONE', *, *, #18943, .T. ) ;
#35518 = CARTESIAN_POINT ( 'NONE',  ( 3.000000000000000000, 1.467624384280024730, -2.542000000000001592 ) ) ;
#35519 = FACE_OUTER_BOUND ( 'NONE', #10118, .T. ) ;
#35520 = CARTESIAN_POINT ( 'NONE',  ( 34.99999662536855283, 60.62177826491078747, -9.999999999999998224 ) ) ;
#35521 = DIRECTION ( 'NONE',  ( 0.000000000000000000, 0.000000000000000000, 1.000000000000000000 ) ) ;
#35522 = ADVANCED_FACE ( 'NONE', ( #15332 ), #7647, .T. ) ;
#35523 = VERTEX_POINT ( 'NONE', #2200 ) ;
#35524 = LINE ( 'NONE', #15459, #14731 ) ;
#35525 = ORIENTED_EDGE ( 'NONE', *, *, #2349, .F. ) ;
#35526 = EDGE_CURVE ( 'NONE', #11341, #23693, #33335, .T. ) ;
#35527 = CARTESIAN_POINT ( 'NONE',  ( 0.000000000000000000, 92.82302294027091705, -29.97964607176054130 ) ) ;
#35528 = LINE ( 'NONE', #18082, #13612 ) ;
#35529 = DIRECTION ( 'NONE',  ( 1.000000000000000000, 0.000000000000000000, 0.000000000000000000 ) ) ;
#35530 = DIRECTION ( 'NONE',  ( 1.000000000000000000, 0.000000000000000000, 0.000000000000000000 ) ) ;
#35531 = EDGE_CURVE ( 'NONE', #20921, #5470, #18270, .T. ) ;
#35532 = AXIS2_PLACEMENT_3D ( 'NONE', #23272, #12361, #3586 ) ;
#35533 = DIRECTION ( 'NONE',  ( 0.4999999999999922839, -0.8660254037844431485, 0.000000000000000000 ) ) ;
#35534 = ADVANCED_FACE ( 'NONE', ( #13825 ), #36877, .F. ) ;
#35535 = CARTESIAN_POINT ( 'NONE',  ( 5.000000000000000000, 1.101175676120959901, -0.7375066809288793879 ) ) ;
#35536 = EDGE_LOOP ( 'NONE', ( #23258, #26663, #25182, #23594, #120 ) ) ;
#35537 = CARTESIAN_POINT ( 'NONE',  ( 42.99999662536848888, -77.94228634059960825, 17.49999999999999645 ) ) ;
#35538 = ADVANCED_FACE ( 'NONE', ( #19271 ), #11186, .T. ) ;
#35539 = DIRECTION ( 'NONE',  ( 0.000000000000000000, 0.000000000000000000, 1.000000000000000000 ) ) ;
#35540 = CARTESIAN_POINT ( 'NONE',  ( 4.279621169095998212, -62.97617850287780072, -4.999999999999997335 ) ) ;
#35541 = ADVANCED_FACE ( 'NONE', ( #22089 ), #25269, .F. ) ;
#35542 = ORIENTED_EDGE ( 'NONE', *, *, #33989, .T. ) ;
#35543 = ORIENTED_EDGE ( 'NONE', *, *, #16860, .T. ) ;
#35544 = EDGE_LOOP ( 'NONE', ( #35876, #30848, #11183, #7648 ) ) ;
#35545 = VECTOR ( 'NONE', #14319, 1000.000000000000000 ) ;
#35546 = CARTESIAN_POINT ( 'NONE',  ( 5.253368672218635460, -3.033033817057790404, -4.359491423763655504 ) ) ;
#35547 = CARTESIAN_POINT ( 'NONE',  ( 86.99999662536832545, 25.98076211353319565, -9.999999999999998224 ) ) ;
#35548 = FACE_OUTER_BOUND ( 'NONE', #25022, .T. ) ;
#35549 = ORIENTED_EDGE ( 'NONE', *, *, #7324, .T. ) ;
#35550 = EDGE_CURVE ( 'NONE', #7036, #29469, #25479, .T. ) ;
#35551 = EDGE_CURVE ( 'NONE', #24428, #18343, #29041, .T. ) ;
#35552 = PRODUCT_DEFINITION_SHAPE ( 'NONE', 'NONE',  #37132 ) ;
#35553 = DIRECTION ( 'NONE',  ( 0.000000000000000000, 0.000000000000000000, 1.000000000000000000 ) ) ;
#35554 = EDGE_CURVE ( 'NONE', #14334, #21168, #1510, .T. ) ;
#35555 = CARTESIAN_POINT ( 'NONE',  ( 36.99999662536855283, 60.62177826491078747, -5.000000000000000000 ) ) ;
#35556 = ORIENTED_EDGE ( 'NONE', *, *, #16243, .F. ) ;
#35557 = FACE_BOUND ( 'NONE', #31259, .T. ) ;
#35558 = ORIENTED_EDGE ( 'NONE', *, *, #27046, .F. ) ;
#35559 = DIRECTION ( 'NONE',  ( 1.000000000000000000, 0.000000000000000000, 0.000000000000000000 ) ) ;
#35560 = AXIS2_PLACEMENT_3D ( 'NONE', #19538, #36230, #10535 ) ;
#35561 = CIRCLE ( 'NONE', #6171, 3.000000000000007105 ) ;
#35562 = DIRECTION ( 'NONE',  ( 0.000000000000000000, 0.000000000000000000, 1.000000000000000000 ) ) ;
#35563 = DIRECTION ( 'NONE',  ( -1.000000000000000000, 0.000000000000000000, 0.000000000000000000 ) ) ;
#35564 = CARTESIAN_POINT ( 'NONE',  ( 94.55012560584681580, 9.234378588654081454, 27.50000000000000000 ) ) ;
#35565 = ORIENTED_EDGE ( 'NONE', *, *, #25146, .T. ) ;
#35566 = FACE_OUTER_BOUND ( 'NONE', #20432, .T. ) ;
#35567 = CIRCLE ( 'NONE', #27162, 4.999999999999997335 ) ;
#35568 = CARTESIAN_POINT ( 'NONE',  ( 84.99999662536831124, -25.98076211353319565, 12.50000000000000000 ) ) ;
#35569 = ADVANCED_FACE ( 'NONE', ( #7842 ), #10993, .F. ) ;
#35570 = CIRCLE ( 'NONE', #28954, 2.000000000000001776 ) ;
#35571 = CARTESIAN_POINT ( 'NONE',  ( 77.99999662536833966, -3.224517592124143893E-15, -9.999999999999998224 ) ) ;
#35572 = DIRECTION ( 'NONE',  ( 0.000000000000000000, 0.000000000000000000, 1.000000000000000000 ) ) ;
#35573 = ORIENTED_EDGE ( 'NONE', *, *, #26626, .T. ) ;
#35574 = EDGE_CURVE ( 'NONE', #16885, #24399, #5112, .T. ) ;
#35575 = FACE_OUTER_BOUND ( 'NONE', #20015, .T. ) ;
#35576 = DIRECTION ( 'NONE',  ( 0.000000000000000000, 0.000000000000000000, 1.000000000000000000 ) ) ;
#35577 = DIRECTION ( 'NONE',  ( -0.000000000000000000, -0.000000000000000000, 1.000000000000000000 ) ) ;
#35578 = AXIS2_PLACEMENT_3D ( 'NONE', #12073, #12645, #27082 ) ;
#35579 = ORIENTED_EDGE ( 'NONE', *, *, #10917, .F. ) ;
#35580 = ORIENTED_EDGE ( 'NONE', *, *, #1412, .T. ) ;
#35581 = ORIENTED_EDGE ( 'NONE', *, *, #24114, .F. ) ;
#35582 = EDGE_CURVE ( 'NONE', #23728, #32620, #33862, .T. ) ;
#35583 = PLANE ( 'NONE',  #14179 ) ;
#35584 = CARTESIAN_POINT ( 'NONE',  ( 69.99999662536839651, 34.64101615137758472, -9.999999999999998224 ) ) ;
#35585 = AXIS2_PLACEMENT_3D ( 'NONE', #10083, #32762, #27122 ) ;
#35586 = DIRECTION ( 'NONE',  ( 1.000000000000000000, 0.000000000000000000, 0.000000000000000000 ) ) ;
#35587 = ORIENTED_EDGE ( 'NONE', *, *, #29987, .T. ) ;
#35588 = DIRECTION ( 'NONE',  ( -1.000000000000000000, 0.000000000000000000, -0.000000000000000000 ) ) ;
#35589 = DIRECTION ( 'NONE',  ( 0.000000000000000000, 0.000000000000000000, 1.000000000000000000 ) ) ;
#35590 = DIRECTION ( 'NONE',  ( 0.000000000000000000, 0.000000000000000000, 1.000000000000000000 ) ) ;
#35591 = EDGE_CURVE ( 'NONE', #2878, #26137, #12278, .T. ) ;
#35592 = ORIENTED_EDGE ( 'NONE', *, *, #5786, .T. ) ;
#35593 = AXIS2_PLACEMENT_3D ( 'NONE', #2620, #33589, #2262 ) ;
#35595 = VERTEX_POINT ( 'NONE', #31070 ) ;
#35594 = EDGE_CURVE ( 'NONE', #35608, #17798, #19446, .T. ) ;
#35596 = CARTESIAN_POINT ( 'NONE',  ( 17.99999662536861678, -86.60254037844400443, -9.999999999999998224 ) ) ;
#35597 = EDGE_CURVE ( 'NONE', #1926, #9828, #23682, .T. ) ;
#35598 = DIRECTION ( 'NONE',  ( 1.000000000000000000, 0.000000000000000000, 0.000000000000000000 ) ) ;
#35600 = ADVANCED_FACE ( 'NONE', ( #1836 ), #10445, .F. ) ;
#35599 = ORIENTED_EDGE ( 'NONE', *, *, #32567, .T. ) ;
#35601 = CARTESIAN_POINT ( 'NONE',  ( -145.0000000000001137, -5.999999999998481215, 32.55002500000000509 ) ) ;
#35602 = ORIENTED_EDGE ( 'NONE', *, *, #2482, .T. ) ;
#35603 = DIRECTION ( 'NONE',  ( 0.000000000000000000, 0.4999999999999997224, -0.8660254037844388186 ) ) ;
#35604 = CARTESIAN_POINT ( 'NONE',  ( 41.99999662536853151, -69.28203230275519786, -9.999999999999998224 ) ) ;
#35605 = ORIENTED_EDGE ( 'NONE', *, *, #7581, .T. ) ;
#35606 = ORIENTED_EDGE ( 'NONE', *, *, #25001, .F. ) ;
#35607 = CARTESIAN_POINT ( 'NONE',  ( 0.000000000000000000, 0.000000000000000000, -5.000000000000000000 ) ) ;
#35608 = VERTEX_POINT ( 'NONE', #2570 ) ;
#35609 = CARTESIAN_POINT ( 'NONE',  ( -23.49154088336464952, 103.5526315789473699, 32.50000000000000000 ) ) ;
#35610 = DIRECTION ( 'NONE',  ( -1.047444401652940007E-14, -1.000000000000000000, 0.000000000000000000 ) ) ;
#35611 = DIRECTION ( 'NONE',  ( -1.000000000000000000, 0.000000000000000000, 0.000000000000000000 ) ) ;
#35612 = ORIENTED_EDGE ( 'NONE', *, *, #14403, .T. ) ;
#35613 = ORIENTED_EDGE ( 'NONE', *, *, #32388, .F. ) ;
#35614 = EDGE_CURVE ( 'NONE', #5261, #27815, #8691, .T. ) ;
#35615 = CIRCLE ( 'NONE', #11049, 2.000000000000001776 ) ;
#35616 = AXIS2_PLACEMENT_3D ( 'NONE', #24347, #32405, #35794 ) ;
#35617 = ORIENTED_EDGE ( 'NONE', *, *, #33762, .T. ) ;
#35618 = ORIENTED_EDGE ( 'NONE', *, *, #13494, .T. ) ;
#35619 = CARTESIAN_POINT ( 'NONE',  ( -37.50000000000000000, -103.4105893997321743, 27.50000000000000000 ) ) ;
#35620 = CARTESIAN_POINT ( 'NONE',  ( -70.00000337463102085, -51.96152422706641971, -9.999999999999998224 ) ) ;
#35621 = ORIENTED_EDGE ( 'NONE', *, *, #25645, .F. ) ;
#35622 = CARTESIAN_POINT ( 'NONE',  ( -50.00000337463109190, 51.96152422706637708, -9.999999999999998224 ) ) ;
#35623 = CARTESIAN_POINT ( 'NONE',  ( 3.499999999999987566, 55.00000000000000000, -10.00000000000000178 ) ) ;
#35624 = ORIENTED_EDGE ( 'NONE', *, *, #15843, .T. ) ;
#35625 = CARTESIAN_POINT ( 'NONE',  ( -85.00000337463092137, -25.98076211353322051, -9.999999999999998224 ) ) ;
#35626 = DIRECTION ( 'NONE',  ( 0.000000000000000000, 0.000000000000000000, 1.000000000000000000 ) ) ;
#35627 = VECTOR ( 'NONE', #6506, 1000.000000000000000 ) ;
#35628 = DIRECTION ( 'NONE',  ( 1.000000000000000000, 0.000000000000000000, 0.000000000000000000 ) ) ;
#35629 = DIRECTION ( 'NONE',  ( 0.000000000000000000, 0.000000000000000000, 1.000000000000000000 ) ) ;
#35630 = DIRECTION ( 'NONE',  ( 0.000000000000000000, 0.000000000000000000, 1.000000000000000000 ) ) ;
#35631 = ORIENTED_EDGE ( 'NONE', *, *, #19302, .F. ) ;
#35632 = EDGE_LOOP ( 'NONE', ( #16121, #7964, #307, #31901, #14954, #6903 ) ) ;
#35633 = CARTESIAN_POINT ( 'NONE',  ( -55.00000337463110611, -43.30127018922202353, 12.50000000000000000 ) ) ;
#35634 = CARTESIAN_POINT ( 'NONE',  ( -30.00000337463119848, -69.28203230275522628, -5.000000000000000000 ) ) ;
#35635 = EDGE_CURVE ( 'NONE', #5095, #33663, #29632, .T. ) ;
#35636 = CARTESIAN_POINT ( 'NONE',  ( -80.69570745083950669, 15.44540918807064500, -5.000000000000000000 ) ) ;
#35637 = DIRECTION ( 'NONE',  ( 0.5000000000000039968, 0.8660254037844363761, 0.000000000000000000 ) ) ;
#35638 = ORIENTED_EDGE ( 'NONE', *, *, #17219, .F. ) ;
#35639 = AXIS2_PLACEMENT_3D ( 'NONE', #2411, #11007, #22447 ) ;
#35640 = CARTESIAN_POINT ( 'NONE',  ( 57.99999662536844625, 34.64101615137759893, -9.999999999999998224 ) ) ;
#35641 = CIRCLE ( 'NONE', #29021, 33.00000000000001421 ) ;
#35642 = CARTESIAN_POINT ( 'NONE',  ( -124.4080600076929954, 12.15049814296761888, 32.50002500000000083 ) ) ;
#35643 = VERTEX_POINT ( 'NONE', #31952 ) ;
#35644 = CARTESIAN_POINT ( 'NONE',  ( -87.83969979969870678, -14.80603122773086966, -49.86561046011506448 ) ) ;
#35645 = ORIENTED_EDGE ( 'NONE', *, *, #15370, .T. ) ;
#35646 = DIRECTION ( 'NONE',  ( -0.000000000000000000, -0.000000000000000000, 1.000000000000000000 ) ) ;
#35647 = LINE ( 'NONE', #35847, #1443 ) ;
#35648 = AXIS2_PLACEMENT_3D ( 'NONE', #1421, #10244, #29929 ) ;
#35649 = DIRECTION ( 'NONE',  ( -0.000000000000000000, -0.000000000000000000, 1.000000000000000000 ) ) ;
#35650 = ORIENTED_EDGE ( 'NONE', *, *, #9239, .T. ) ;
#35651 = VERTEX_POINT ( 'NONE', #28619 ) ;
#35652 = ADVANCED_FACE ( 'NONE', ( #2951 ), #31785, .F. ) ;
#35653 = VECTOR ( 'NONE', #34437, 1000.000000000000000 ) ;
#35654 = EDGE_LOOP ( 'NONE', ( #4638, #349 ) ) ;
#35655 = CYLINDRICAL_SURFACE ( 'NONE', #23172, 2.000000000000000000 ) ;
#35656 = DIRECTION ( 'NONE',  ( -0.000000000000000000, -0.000000000000000000, 1.000000000000000000 ) ) ;
#35657 = EDGE_CURVE ( 'NONE', #28819, #24755, #22474, .T. ) ;
#35658 = DIRECTION ( 'NONE',  ( 1.000000000000000000, 0.000000000000000000, 0.000000000000000000 ) ) ;
#35659 = CARTESIAN_POINT ( 'NONE',  ( -5.000000000000000888, -2.886751345948162406, -3.984345921091775100 ) ) ;
#35660 = AXIS2_PLACEMENT_3D ( 'NONE', #3842, #15285, #26723 ) ;
#35661 = CARTESIAN_POINT ( 'NONE',  ( -59.29837256189559724, -31.02796211690927919, -49.86561046011506448 ) ) ;
#35662 = EDGE_LOOP ( 'NONE', ( #35690, #3273 ) ) ;
#35663 = DIRECTION ( 'NONE',  ( 1.000000000000000000, 0.000000000000000000, 0.000000000000000000 ) ) ;
#35664 = VECTOR ( 'NONE', #33672, 1000.000000000000000 ) ;
#35665 = AXIS2_PLACEMENT_3D ( 'NONE', #386, #11820, #583 ) ;
#35666 = CARTESIAN_POINT ( 'NONE',  ( -73.00000337463097821, 8.660254037844374864, 12.50000000000000000 ) ) ;
#35667 = ADVANCED_FACE ( 'NONE', ( #28967 ), #6292, .F. ) ;
#35668 = DIRECTION ( 'NONE',  ( 0.000000000000000000, 0.000000000000000000, 1.000000000000000000 ) ) ;
#35669 = ORIENTED_EDGE ( 'NONE', *, *, #337, .T. ) ;
#35670 = CARTESIAN_POINT ( 'NONE',  ( 70.47608876694671665, 59.13646009116074964, -4.999999999999997335 ) ) ;
#35671 = DIRECTION ( 'NONE',  ( 0.000000000000000000, 0.000000000000000000, 1.000000000000000000 ) ) ;
#35672 = ORIENTED_EDGE ( 'NONE', *, *, #9971, .T. ) ;
#35673 = ORIENTED_EDGE ( 'NONE', *, *, #6677, .F. ) ;
#35674 = CIRCLE ( 'NONE', #6947, 27.00000000000001776 ) ;
#35675 = DIRECTION ( 'NONE',  ( 1.000000000000000000, 0.000000000000000000, 0.000000000000000000 ) ) ;
#35676 = EDGE_CURVE ( 'NONE', #33091, #15386, #14733, .T. ) ;
#35677 = CARTESIAN_POINT ( 'NONE',  ( 9.999996625368655856, -69.28203230275519786, -9.999999999999998224 ) ) ;
#35678 = AXIS2_PLACEMENT_3D ( 'NONE', #11652, #26657, #23483 ) ;
#35679 = CARTESIAN_POINT ( 'NONE',  ( -17.14523346298279449, 93.36492675454785228, 12.49999999999999822 ) ) ;
#35680 = VERTEX_POINT ( 'NONE', #34262 ) ;
#35681 = ORIENTED_EDGE ( 'NONE', *, *, #7833, .T. ) ;
#35682 = CIRCLE ( 'NONE', #26086, 2.000000000000001776 ) ;
#35683 = ORIENTED_EDGE ( 'NONE', *, *, #23866, .F. ) ;
#35684 = VECTOR ( 'NONE', #34534, 1000.000000000000000 ) ;
#35685 = CIRCLE ( 'NONE', #16515, 2.000000000000001776 ) ;
#35686 = CARTESIAN_POINT ( 'NONE',  ( 6.000000000000000000, -145.0000000000000568, 32.50000000000000000 ) ) ;
#35687 = EDGE_LOOP ( 'NONE', ( #30262, #31805, #31978, #24919 ) ) ;
#35688 = ORIENTED_EDGE ( 'NONE', *, *, #36156, .F. ) ;
#35689 = DIRECTION ( 'NONE',  ( -1.000000000000000000, 0.000000000000000000, 0.000000000000000000 ) ) ;
#35690 = ORIENTED_EDGE ( 'NONE', *, *, #15087, .T. ) ;
#35691 = ORIENTED_EDGE ( 'NONE', *, *, #22906, .T. ) ;
#35692 = EDGE_CURVE ( 'NONE', #21307, #27070, #32635, .T. ) ;
#35693 = VECTOR ( 'NONE', #4850, 1000.000000000000000 ) ;
#35694 = CYLINDRICAL_SURFACE ( 'NONE', #446, 2.000000000000001776 ) ;
#35695 = EDGE_CURVE ( 'NONE', #35086, #11321, #27263, .T. ) ;
#35696 = CYLINDRICAL_SURFACE ( 'NONE', #34434, 2.000000000000001776 ) ;
#35697 = ORIENTED_EDGE ( 'NONE', *, *, #27011, .T. ) ;
#35698 = VERTEX_POINT ( 'NONE', #11377 ) ;
#35699 = DIRECTION ( 'NONE',  ( 1.000000000000000000, 0.000000000000000000, 0.000000000000000000 ) ) ;
#35700 = DIRECTION ( 'NONE',  ( -1.000000000000000000, 0.000000000000000000, 0.000000000000000000 ) ) ;
#35701 = AXIS2_PLACEMENT_3D ( 'NONE', #2927, #2720, #22973 ) ;
#35702 = DIRECTION ( 'NONE',  ( 0.000000000000000000, 0.000000000000000000, 1.000000000000000000 ) ) ;
#35703 = DIRECTION ( 'NONE',  ( 1.000000000000000000, 0.000000000000000000, 0.000000000000000000 ) ) ;
#35704 = ORIENTED_EDGE ( 'NONE', *, *, #22776, .T. ) ;
#35705 = DIRECTION ( 'NONE',  ( 1.000000000000000000, 0.000000000000000000, 0.000000000000000000 ) ) ;
#35706 = VERTEX_POINT ( 'NONE', #11540 ) ;
#35707 = DIRECTION ( 'NONE',  ( 1.000000000000000000, 0.000000000000000000, 0.000000000000000000 ) ) ;
#35708 = ADVANCED_FACE ( 'NONE', ( #29169 ), #5563, .F. ) ;
#35709 =( GEOMETRIC_REPRESENTATION_CONTEXT ( 3 ) GLOBAL_UNCERTAINTY_ASSIGNED_CONTEXT ( ( #1318 ) ) GLOBAL_UNIT_ASSIGNED_CONTEXT ( ( #23595, #34859, #29223 ) ) REPRESENTATION_CONTEXT ( 'NONE', 'WORKASPACE' ) );
#35710 = DIRECTION ( 'NONE',  ( 1.000000000000000000, 0.000000000000000000, 0.000000000000000000 ) ) ;
#35711 = DIRECTION ( 'NONE',  ( 0.000000000000000000, 0.000000000000000000, 1.000000000000000000 ) ) ;
#35712 = AXIS2_PLACEMENT_3D ( 'NONE', #3704, #32951, #32387 ) ;
#35713 = CYLINDRICAL_SURFACE ( 'NONE', #3946, 2.000000000000001776 ) ;
#35714 = CIRCLE ( 'NONE', #1574, 2.000000000000001776 ) ;
#35715 = DIRECTION ( 'NONE',  ( -1.000000000000000000, 3.552713678800500929E-15, 0.000000000000000000 ) ) ;
#35716 = CIRCLE ( 'NONE', #32699, 4.999999999999997335 ) ;
#35717 = DIRECTION ( 'NONE',  ( 1.000000000000000000, 0.000000000000000000, 0.000000000000000000 ) ) ;
#35718 = EDGE_CURVE ( 'NONE', #9542, #10851, #14934, .T. ) ;
#35719 = DIRECTION ( 'NONE',  ( 0.000000000000000000, 0.000000000000000000, 1.000000000000000000 ) ) ;
#35720 = ORIENTED_EDGE ( 'NONE', *, *, #5057, .F. ) ;
#35721 = DIRECTION ( 'NONE',  ( -1.000000000000000000, 0.000000000000000000, 0.000000000000000000 ) ) ;
#35722 = DIRECTION ( 'NONE',  ( 0.000000000000000000, -0.000000000000000000, -1.000000000000000000 ) ) ;
#35723 = FACE_OUTER_BOUND ( 'NONE', #6137, .T. ) ;
#35724 = EDGE_LOOP ( 'NONE', ( #18719, #6012 ) ) ;
#35725 = CIRCLE ( 'NONE', #6370, 2.000000000000001776 ) ;
#35726 = VERTEX_POINT ( 'NONE', #491 ) ;
#35727 = ORIENTED_EDGE ( 'NONE', *, *, #13095, .T. ) ;
#35728 = CARTESIAN_POINT ( 'NONE',  ( 57.99999662536842493, -51.96152422706639840, -9.999999999999998224 ) ) ;
#35729 = CARTESIAN_POINT ( 'NONE',  ( -22.00000337463124112, -69.28203230275522628, 17.49999999999999645 ) ) ;
#35730 = DIRECTION ( 'NONE',  ( 1.000000000000000000, 0.000000000000000000, 0.000000000000000000 ) ) ;
#35731 = ORIENTED_EDGE ( 'NONE', *, *, #14853, .F. ) ;
#35732 = AXIS2_PLACEMENT_3D ( 'NONE', #32892, #7212, #30063 ) ;
#35733 = CARTESIAN_POINT ( 'NONE',  ( -15.00000337463126066, 77.94228634059957983, -9.999999999999998224 ) ) ;
#35734 = ADVANCED_FACE ( 'NONE', ( #8392 ), #23187, .F. ) ;
#35735 = CIRCLE ( 'NONE', #15977, 2.000000000000001776 ) ;
#35736 = DIRECTION ( 'NONE',  ( -0.000000000000000000, -0.000000000000000000, -1.000000000000000000 ) ) ;
#35737 = ORIENTED_EDGE ( 'NONE', *, *, #17143, .F. ) ;
#35738 = DIRECTION ( 'NONE',  ( -1.000000000000000000, 0.000000000000000000, 0.000000000000000000 ) ) ;
#35739 = ORIENTED_EDGE ( 'NONE', *, *, #28504, .F. ) ;
#35740 = CARTESIAN_POINT ( 'NONE',  ( 44.99999662536851019, 77.94228634059959404, 12.50000000000000000 ) ) ;
#35741 = VECTOR ( 'NONE', #21067, 1000.000000000000000 ) ;
#35742 = CIRCLE ( 'NONE', #2815, 2.000000000000001776 ) ;
#35743 = ADVANCED_FACE ( 'NONE', ( #16999 ), #34633, .F. ) ;
#35744 = CIRCLE ( 'NONE', #3401, 2.000000000000000000 ) ;
#35745 = AXIS2_PLACEMENT_3D ( 'NONE', #27300, #9868, #20744 ) ;
#35746 = LINE ( 'NONE', #36109, #2194 ) ;
#35747 = DIRECTION ( 'NONE',  ( 0.000000000000000000, 0.000000000000000000, 1.000000000000000000 ) ) ;
#35748 = EDGE_CURVE ( 'NONE', #2363, #10643, #20530, .T. ) ;
#35749 = SURFACE_STYLE_FILL_AREA ( #26929 ) ;
#35750 = ORIENTED_EDGE ( 'NONE', *, *, #31522, .T. ) ;
#35751 = DIRECTION ( 'NONE',  ( 0.000000000000000000, 0.000000000000000000, 1.000000000000000000 ) ) ;
#35752 = CIRCLE ( 'NONE', #17198, 33.00000000000001421 ) ;
#35753 = CARTESIAN_POINT ( 'NONE',  ( -68.17080498304596858, 51.15280100851584422, 12.50000000000000000 ) ) ;
#35754 = CARTESIAN_POINT ( 'NONE',  ( 10.21421739743242618, 84.61404610869705323, -5.000000000000000000 ) ) ;
#35755 = CARTESIAN_POINT ( 'NONE',  ( 64.99999662536839651, -60.62177826491080168, 17.49999999999999645 ) ) ;
#35756 = ORIENTED_EDGE ( 'NONE', *, *, #9481, .F. ) ;
#35757 = DIRECTION ( 'NONE',  ( -1.000000000000000000, 0.000000000000000000, 0.000000000000000000 ) ) ;
#35758 = CARTESIAN_POINT ( 'NONE',  ( 3.000000000000000000, -2.935248768560059229, 3.469446951953614189E-15 ) ) ;
#35759 = DIRECTION ( 'NONE',  ( 0.000000000000000000, 0.000000000000000000, 1.000000000000000000 ) ) ;
#35760 = CIRCLE ( 'NONE', #20196, 27.00000000000001776 ) ;
#35761 = ORIENTED_EDGE ( 'NONE', *, *, #14432, .F. ) ;
#35762 = EDGE_CURVE ( 'NONE', #3917, #13513, #36856, .T. ) ;
#35763 = AXIS2_PLACEMENT_3D ( 'NONE', #23925, #17917, #26354 ) ;
#35764 = VERTEX_POINT ( 'NONE', #17729 ) ;
#35765 = DIRECTION ( 'NONE',  ( 0.000000000000000000, 0.000000000000000000, -1.000000000000000000 ) ) ;
#35766 = CARTESIAN_POINT ( 'NONE',  ( -80.00000337463094979, -17.32050807568882078, -9.999999999999998224 ) ) ;
#35767 = AXIS2_PLACEMENT_3D ( 'NONE', #17815, #3581, #26439 ) ;
#35768 = CARTESIAN_POINT ( 'NONE',  ( -33.00000337463116296, 60.62177826491077326, -5.000000000000000000 ) ) ;
#35769 = AXIS2_PLACEMENT_3D ( 'NONE', #11356, #14362, #17523 ) ;
#35770 = ORIENTED_EDGE ( 'NONE', *, *, #35022, .T. ) ;
#35771 = CYLINDRICAL_SURFACE ( 'NONE', #9195, 3.499999999999991562 ) ;
#35772 = DIRECTION ( 'NONE',  ( 0.000000000000000000, 0.000000000000000000, 1.000000000000000000 ) ) ;
#35773 = DIRECTION ( 'NONE',  ( 1.000000000000000000, 0.000000000000000000, 0.000000000000000000 ) ) ;
#35774 = AXIS2_PLACEMENT_3D ( 'NONE', #21120, #13057, #35757 ) ;
#35775 = CYLINDRICAL_SURFACE ( 'NONE', #26801, 2.000000000000001776 ) ;
#35776 = VERTEX_POINT ( 'NONE', #3123 ) ;
#35777 = AXIS2_PLACEMENT_3D ( 'NONE', #24196, #27012, #15399 ) ;
#35778 = VERTEX_POINT ( 'NONE', #14185 ) ;
#35779 = DIRECTION ( 'NONE',  ( 0.000000000000000000, 0.000000000000000000, 1.000000000000000000 ) ) ;
#35780 = EDGE_CURVE ( 'NONE', #10920, #24629, #17709, .T. ) ;
#35781 = DIRECTION ( 'NONE',  ( 0.000000000000000000, 0.000000000000000000, -1.000000000000000000 ) ) ;
#35782 = ORIENTED_EDGE ( 'NONE', *, *, #23944, .F. ) ;
#35783 = EDGE_CURVE ( 'NONE', #27651, #20315, #17192, .T. ) ;
#35784 = CARTESIAN_POINT ( 'NONE',  ( -72.00000337463100664, 17.32050807568877460, -5.000000000000000000 ) ) ;
#35785 = ORIENTED_EDGE ( 'NONE', *, *, #15939, .T. ) ;
#35786 = DIRECTION ( 'NONE',  ( -1.000000000000000000, -0.000000000000000000, -0.000000000000000000 ) ) ;
#35787 = VECTOR ( 'NONE', #36163, 1000.000000000000000 ) ;
#35788 = EDGE_CURVE ( 'NONE', #35651, #29261, #12915, .T. ) ;
#35789 = AXIS2_PLACEMENT_3D ( 'NONE', #16349, #7178, #18618 ) ;
#35790 = DIRECTION ( 'NONE',  ( 1.000000000000000000, 0.000000000000000000, 0.000000000000000000 ) ) ;
#35791 = ORIENTED_EDGE ( 'NONE', *, *, #29895, .T. ) ;
#35792 = ORIENTED_EDGE ( 'NONE', *, *, #11367, .F. ) ;
#35793 = EDGE_CURVE ( 'NONE', #21238, #13993, #30875, .T. ) ;
#35794 = DIRECTION ( 'NONE',  ( -1.000000000000000000, 0.000000000000000000, -0.000000000000000000 ) ) ;
#35795 = ORIENTED_EDGE ( 'NONE', *, *, #23547, .T. ) ;
#35796 = EDGE_CURVE ( 'NONE', #6603, #182, #1543, .T. ) ;
#35798 = MECHANICAL_DESIGN_GEOMETRIC_PRESENTATION_REPRESENTATION (  '', ( #30992 ), #30898 ) ;
#35797 = SURFACE_STYLE_FILL_AREA ( #7660 ) ;
#35799 = AXIS2_PLACEMENT_3D ( 'NONE', #36097, #1956, #7231 ) ;
#35800 = CARTESIAN_POINT ( 'NONE',  ( 62.99999662536839651, -43.30127018922199511, 12.50000000000000000 ) ) ;
#35801 = CIRCLE ( 'NONE', #33386, 2.000000000000001776 ) ;
#35802 = FACE_OUTER_BOUND ( 'NONE', #19554, .T. ) ;
#35803 = DIRECTION ( 'NONE',  ( 0.000000000000000000, 0.000000000000000000, 1.000000000000000000 ) ) ;
#35804 = EDGE_LOOP ( 'NONE', ( #28518, #32487 ) ) ;
#35805 = DIRECTION ( 'NONE',  ( 0.000000000000000000, 0.000000000000000000, -1.000000000000000000 ) ) ;
#35806 = DIRECTION ( 'NONE',  ( 0.000000000000000000, 0.000000000000000000, -1.000000000000000000 ) ) ;
#35807 = CIRCLE ( 'NONE', #4080, 3.000000000000006661 ) ;
#35808 = EDGE_CURVE ( 'NONE', #10982, #17563, #32922, .T. ) ;
#35809 = VERTEX_POINT ( 'NONE', #27275 ) ;
#35810 = EDGE_CURVE ( 'NONE', #10952, #16326, #2757, .T. ) ;
#35811 = VERTEX_POINT ( 'NONE', #15288 ) ;
#35812 = VERTEX_POINT ( 'NONE', #26921 ) ;
#35813 = EDGE_CURVE ( 'NONE', #7555, #9227, #6330, .T. ) ;
#35814 = CARTESIAN_POINT ( 'NONE',  ( -70.00000337463099243, 17.32050807568877460, -5.000000000000000000 ) ) ;
#35815 = AXIS2_PLACEMENT_3D ( 'NONE', #2902, #629, #37028 ) ;
#35816 = EDGE_CURVE ( 'NONE', #27142, #7889, #956, .T. ) ;
#35817 = CARTESIAN_POINT ( 'NONE',  ( -63.00000337463104927, -43.30127018922202353, 17.49999999999999645 ) ) ;
#35818 = ORIENTED_EDGE ( 'NONE', *, *, #36270, .F. ) ;
#35819 = AXIS2_PLACEMENT_3D ( 'NONE', #7085, #35228, #32391 ) ;
#35820 = AXIS2_PLACEMENT_3D ( 'NONE', #6772, #12954, #23859 ) ;
#35821 = CARTESIAN_POINT ( 'NONE',  ( -4.999999999999999112, -2.691295138309024448, -1.881393335304213821 ) ) ;
#35822 = DIRECTION ( 'NONE',  ( 1.000000000000000000, 0.000000000000000000, 0.000000000000000000 ) ) ;
#35823 = VERTEX_POINT ( 'NONE', #18100 ) ;
#35824 = DIRECTION ( 'NONE',  ( -1.000000000000000000, 0.000000000000000000, -0.000000000000000000 ) ) ;
#35825 = CARTESIAN_POINT ( 'NONE',  ( -53.00000337463106348, 43.30127018922197379, -9.999999999999998224 ) ) ;
#35826 = CARTESIAN_POINT ( 'NONE',  ( -50.00000337463109190, 69.28203230275518365, 17.49999999999999645 ) ) ;
#35827 = CARTESIAN_POINT ( 'NONE',  ( -6.069707180676227632E-15, 5.773502691896268857, -3.984345921091771547 ) ) ;
#35828 = CARTESIAN_POINT ( 'NONE',  ( -48.00000337463112032, -51.96152422706641971, 12.50000000000000000 ) ) ;
#35829 = DIRECTION ( 'NONE',  ( 0.000000000000000000, 0.000000000000000000, -1.000000000000000000 ) ) ;
#35830 = ORIENTED_EDGE ( 'NONE', *, *, #26497, .T. ) ;
#35831 = VERTEX_POINT ( 'NONE', #12654 ) ;
#35832 = VECTOR ( 'NONE', #2434, 1000.000000000000000 ) ;
#35833 = CARTESIAN_POINT ( 'NONE',  ( -67.00000337463104927, -43.30127018922202353, 12.50000000000000000 ) ) ;
#35834 = CARTESIAN_POINT ( 'NONE',  ( 59.99999662536842493, 51.96152422706639129, 12.50000000000000000 ) ) ;
#35835 = CARTESIAN_POINT ( 'NONE',  ( 0.000000000000000000, 0.000000000000000000, 12.49999999999999822 ) ) ;
#35836 = DIRECTION ( 'NONE',  ( 0.000000000000000000, 0.000000000000000000, 1.000000000000000000 ) ) ;
#35837 = ORIENTED_EDGE ( 'NONE', *, *, #2829, .T. ) ;
#35838 = VECTOR ( 'NONE', #32795, 1000.000000000000000 ) ;
#35839 = CARTESIAN_POINT ( 'NONE',  ( 1.999996625368710257, -69.28203230275519786, -5.000000000000000000 ) ) ;
#35840 = CARTESIAN_POINT ( 'NONE',  ( 27.99999662536857414, -69.28203230275519786, 12.50000000000000000 ) ) ;
#35841 = ORIENTED_EDGE ( 'NONE', *, *, #24800, .T. ) ;
#35842 = CIRCLE ( 'NONE', #10085, 2.000000000000001776 ) ;
#35843 = CARTESIAN_POINT ( 'NONE',  ( 0.000000000000000000, 0.000000000000000000, 27.50000000000000000 ) ) ;
#35844 = ORIENTED_EDGE ( 'NONE', *, *, #9131, .T. ) ;
#35845 = AXIS2_PLACEMENT_3D ( 'NONE', #17705, #26156, #20908 ) ;
#35846 = DIRECTION ( 'NONE',  ( -0.4999999999999980016, 0.8660254037844398178, 0.000000000000000000 ) ) ;
#35847 = CARTESIAN_POINT ( 'NONE',  ( 46.99999662536849598, -77.94228634059960825, -9.999999999999998224 ) ) ;
#35848 = DIRECTION ( 'NONE',  ( -0.7071067811865487940, -0.7071067811865463515, 0.000000000000000000 ) ) ;
#35849 = ORIENTED_EDGE ( 'NONE', *, *, #35594, .T. ) ;
#35850 = ORIENTED_EDGE ( 'NONE', *, *, #26982, .T. ) ;
#35851 = CIRCLE ( 'NONE', #31129, 3.499999999999996003 ) ;
#35852 = VECTOR ( 'NONE', #8492, 1000.000000000000000 ) ;
#35853 = ORIENTED_EDGE ( 'NONE', *, *, #673, .T. ) ;
#35854 = FACE_OUTER_BOUND ( 'NONE', #34046, .T. ) ;
#35855 = ADVANCED_FACE ( 'NONE', ( #18284 ), #27093, .F. ) ;
#35856 = FACE_BOUND ( 'NONE', #30924, .T. ) ;
#35857 = DIRECTION ( 'NONE',  ( 0.000000000000000000, 0.000000000000000000, 1.000000000000000000 ) ) ;
#35858 = DIRECTION ( 'NONE',  ( 0.000000000000000000, 0.000000000000000000, 1.000000000000000000 ) ) ;
#35859 = CARTESIAN_POINT ( 'NONE',  ( 52.99999662536844625, 60.62177826491077326, -9.999999999999998224 ) ) ;
#35860 = EDGE_LOOP ( 'NONE', ( #14337, #24435, #34, #34707 ) ) ;
#35861 = CARTESIAN_POINT ( 'NONE',  ( 0.000000000000000000, 89.94802294027088863, -24.99999999999999645 ) ) ;
#35862 = DIRECTION ( 'NONE',  ( 0.000000000000000000, -0.000000000000000000, -1.000000000000000000 ) ) ;
#35863 = CIRCLE ( 'NONE', #24490, 30.00000000000001421 ) ;
#35864 = DIRECTION ( 'NONE',  ( 0.000000000000000000, 0.000000000000000000, 1.000000000000000000 ) ) ;
#35865 = ORIENTED_EDGE ( 'NONE', *, *, #2539, .T. ) ;
#35866 = DIRECTION ( 'NONE',  ( -0.000000000000000000, 0.8660254037844420383, -0.4999999999999945599 ) ) ;
#35867 = VECTOR ( 'NONE', #1011, 1000.000000000000000 ) ;
#35868 = FACE_OUTER_BOUND ( 'NONE', #8288, .T. ) ;
#35869 = ORIENTED_EDGE ( 'NONE', *, *, #9478, .T. ) ;
#35870 = ORIENTED_EDGE ( 'NONE', *, *, #14686, .F. ) ;
#35871 = DIRECTION ( 'NONE',  ( 0.000000000000000000, 0.000000000000000000, 1.000000000000000000 ) ) ;
#35872 = CARTESIAN_POINT ( 'NONE',  ( -18.00000337463124467, 69.28203230275516944, -9.999999999999998224 ) ) ;
#35873 = CARTESIAN_POINT ( 'NONE',  ( 0.000000000000000000, 0.000000000000000000, 27.50000000000000000 ) ) ;
#35874 = ORIENTED_EDGE ( 'NONE', *, *, #23643, .F. ) ;
#35875 = ORIENTED_EDGE ( 'NONE', *, *, #26535, .F. ) ;
#35876 = ORIENTED_EDGE ( 'NONE', *, *, #18119, .F. ) ;
#35877 = ADVANCED_FACE ( 'NONE', ( #29714 ), #32158, .T. ) ;
#35878 = CIRCLE ( 'NONE', #13119, 3.500000000000000888 ) ;
#35879 = EDGE_CURVE ( 'NONE', #17794, #12035, #11707, .T. ) ;
#35880 = SHAPE_REPRESENTATION ( 'Pneumatic caliper', ( #21385 ), #29775 ) ;
#35881 = DIRECTION ( 'NONE',  ( 1.000000000000000000, 0.000000000000000000, 0.000000000000000000 ) ) ;
#35882 = AXIS2_PLACEMENT_3D ( 'NONE', #30330, #4667, #1843 ) ;
#35883 = VERTEX_POINT ( 'NONE', #32720 ) ;
#35884 = ORIENTED_EDGE ( 'NONE', *, *, #34757, .F. ) ;
#35885 = FACE_BOUND ( 'NONE', #10586, .T. ) ;
#35886 = EDGE_LOOP ( 'NONE', ( #16813, #18883 ) ) ;
#35887 = ORIENTED_EDGE ( 'NONE', *, *, #12860, .T. ) ;
#35888 = ADVANCED_FACE ( 'NONE', ( #17930 ), #4049, .F. ) ;
#35889 = EDGE_CURVE ( 'NONE', #11035, #21946, #29072, .T. ) ;
#35890 = DIRECTION ( 'NONE',  ( -1.000000000000000000, 0.000000000000000000, 0.000000000000000000 ) ) ;
#35891 = VECTOR ( 'NONE', #26384, 1000.000000000000000 ) ;
#35892 = DIRECTION ( 'NONE',  ( 1.000000000000000000, 0.000000000000000000, 0.000000000000000000 ) ) ;
#35893 = ORIENTED_EDGE ( 'NONE', *, *, #24225, .F. ) ;
#35894 = ORIENTED_EDGE ( 'NONE', *, *, #13222, .T. ) ;
#35895 = CARTESIAN_POINT ( 'NONE',  ( -12.00000337463128908, 69.28203230275516944, -9.999999999999998224 ) ) ;
#35896 = AXIS2_PLACEMENT_3D ( 'NONE', #34007, #19750, #33804 ) ;
#35897 = DIRECTION ( 'NONE',  ( -0.000000000000000000, -0.000000000000000000, 1.000000000000000000 ) ) ;
#35898 = CARTESIAN_POINT ( 'NONE',  ( 0.000000000000000000, 0.000000000000000000, 15.00000000000000000 ) ) ;
#35899 = LINE ( 'NONE', #16016, #33441 ) ;
#35900 = ORIENTED_EDGE ( 'NONE', *, *, #24660, .F. ) ;
#35901 = CARTESIAN_POINT ( 'NONE',  ( 9.999996625368618552, 69.28203230275516944, -9.999999999999998224 ) ) ;
#35902 = AXIS2_PLACEMENT_3D ( 'NONE', #2351, #16402, #4962 ) ;
#35903 = ORIENTED_EDGE ( 'NONE', *, *, #4007, .F. ) ;
#35904 = EDGE_CURVE ( 'NONE', #21552, #25354, #15671, .T. ) ;
#35905 = CARTESIAN_POINT ( 'NONE',  ( -68.00000337463099243, -2.428612866367529932E-14, 12.50000000000000000 ) ) ;
#35906 = DIRECTION ( 'NONE',  ( -1.000000000000000000, 0.000000000000000000, -0.000000000000000000 ) ) ;
#35907 = CARTESIAN_POINT ( 'NONE',  ( 27.99999662536857414, -69.28203230275519786, 17.49999999999999645 ) ) ;
#35908 = CARTESIAN_POINT ( 'NONE',  ( 84.99999662536832545, 8.660254037844394404, -9.999999999999998224 ) ) ;
#35909 = AXIS2_PLACEMENT_3D ( 'NONE', #2402, #28425, #2753 ) ;
#35910 = DIRECTION ( 'NONE',  ( -1.000000000000000000, 0.000000000000000000, 0.000000000000000000 ) ) ;
#35911 = AXIS2_PLACEMENT_3D ( 'NONE', #7420, #18860, #30283 ) ;
#35912 = DIRECTION ( 'NONE',  ( 1.000000000000000000, 0.000000000000000000, 0.000000000000000000 ) ) ;
#35913 = DIRECTION ( 'NONE',  ( 1.000000000000000000, 0.000000000000000000, 0.000000000000000000 ) ) ;
#35914 = AXIS2_PLACEMENT_3D ( 'NONE', #8332, #22017, #5681 ) ;
#35915 = ORIENTED_EDGE ( 'NONE', *, *, #1129, .T. ) ;
#35916 = FACE_OUTER_BOUND ( 'NONE', #15147, .T. ) ;
#35917 = DIRECTION ( 'NONE',  ( -0.000000000000000000, -0.000000000000000000, 1.000000000000000000 ) ) ;
#35918 = CYLINDRICAL_SURFACE ( 'NONE', #27117, 2.000000000000001776 ) ;
#35919 = VERTEX_POINT ( 'NONE', #35555 ) ;
#35920 = ORIENTED_EDGE ( 'NONE', *, *, #25367, .T. ) ;
#35921 = ORIENTED_EDGE ( 'NONE', *, *, #4995, .F. ) ;
#35922 = AXIS2_PLACEMENT_3D ( 'NONE', #34826, #9120, #14953 ) ;
#35923 = EDGE_CURVE ( 'NONE', #13732, #13259, #12264, .T. ) ;
#35924 = DIRECTION ( 'NONE',  ( 1.000000000000000000, 0.000000000000000000, 0.000000000000000000 ) ) ;
#35925 = FACE_OUTER_BOUND ( 'NONE', #14501, .T. ) ;
#35926 = AXIS2_PLACEMENT_3D ( 'NONE', #304, #8574, #34454 ) ;
#35927 = ORIENTED_EDGE ( 'NONE', *, *, #15047, .T. ) ;
#35928 = EDGE_CURVE ( 'NONE', #12074, #20954, #24300, .T. ) ;
#35929 = CYLINDRICAL_SURFACE ( 'NONE', #32893, 2.000000000000001776 ) ;
#35930 = DIRECTION ( 'NONE',  ( 1.000000000000000000, 0.000000000000000000, 0.000000000000000000 ) ) ;
#35931 = ORIENTED_EDGE ( 'NONE', *, *, #4844, .T. ) ;
#35932 = CARTESIAN_POINT ( 'NONE',  ( 49.99999662536848177, -51.96152422706640550, -9.999999999999998224 ) ) ;
#35933 = EDGE_CURVE ( 'NONE', #35680, #30153, #8139, .T. ) ;
#35934 = VERTEX_POINT ( 'NONE', #29525 ) ;
#35935 = DIRECTION ( 'NONE',  ( 0.000000000000000000, 0.000000000000000000, -1.000000000000000000 ) ) ;
#35936 = AXIS2_PLACEMENT_3D ( 'NONE', #26682, #20676, #26131 ) ;
#35937 = CIRCLE ( 'NONE', #35270, 3.500000000000003109 ) ;
#35938 = EDGE_CURVE ( 'NONE', #8999, #4753, #26728, .T. ) ;
#35939 = CARTESIAN_POINT ( 'NONE',  ( 74.99999662536836809, -8.660254037844401509, 12.50000000000000000 ) ) ;
#35940 = CARTESIAN_POINT ( 'NONE',  ( -27.00000337463121625, -77.94228634059963667, -9.999999999999998224 ) ) ;
#35941 = DIRECTION ( 'NONE',  ( 0.8660254037844337116, -0.5000000000000084377, 0.000000000000000000 ) ) ;
#35942 = CIRCLE ( 'NONE', #32332, 2.000000000000001776 ) ;
#35943 = EDGE_LOOP ( 'NONE', ( #17244, #24406 ) ) ;
#35944 = CARTESIAN_POINT ( 'NONE',  ( -70.80619744049063513, -84.18124734178186941, 32.50000000000000000 ) ) ;
#35945 = VECTOR ( 'NONE', #28143, 1000.000000000000000 ) ;
#35946 = APPLICATION_PROTOCOL_DEFINITION ( 'draft international standard', 'automotive_design', 1998, #3174 ) ;
#35947 = PLANE ( 'NONE',  #5123 ) ;
#35948 = CARTESIAN_POINT ( 'NONE',  ( 4.279621169095998212, -62.97617850287780072, 12.49999999999999822 ) ) ;
#35949 = CIRCLE ( 'NONE', #4793, 2.000000000000001776 ) ;
#35950 = FACE_OUTER_BOUND ( 'NONE', #34218, .T. ) ;
#35951 = CARTESIAN_POINT ( 'NONE',  ( -32.00000337463119848, -69.28203230275522628, -5.000000000000000000 ) ) ;
#35952 = EDGE_LOOP ( 'NONE', ( #7514, #25040 ) ) ;
#35953 = DIRECTION ( 'NONE',  ( 1.000000000000000000, 0.000000000000000000, 0.000000000000000000 ) ) ;
#35954 = CIRCLE ( 'NONE', #29346, 2.000000000000001776 ) ;
#35955 = DIRECTION ( 'NONE',  ( 1.000000000000000000, 0.000000000000000000, 0.000000000000000000 ) ) ;
#35956 = DIRECTION ( 'NONE',  ( 1.000000000000000000, 0.000000000000000000, 0.000000000000000000 ) ) ;
#35957 = EDGE_CURVE ( 'NONE', #19694, #28337, #36884, .T. ) ;
#35958 = ORIENTED_EDGE ( 'NONE', *, *, #884, .T. ) ;
#35959 = VERTEX_POINT ( 'NONE', #3047 ) ;
#35960 = AXIS2_PLACEMENT_3D ( 'NONE', #22938, #34377, #28197 ) ;
#35961 = CARTESIAN_POINT ( 'NONE',  ( -19.13981058454750794, 60.93295298010998806, 12.49999999999999822 ) ) ;
#35962 = DIRECTION ( 'NONE',  ( 0.000000000000000000, 0.000000000000000000, 1.000000000000000000 ) ) ;
#35963 = EDGE_CURVE ( 'NONE', #623, #8343, #5755, .T. ) ;
#35964 = DIRECTION ( 'NONE',  ( 1.000000000000000000, 0.000000000000000000, 0.000000000000000000 ) ) ;
#35965 = ORIENTED_EDGE ( 'NONE', *, *, #14997, .T. ) ;
#35966 = EDGE_CURVE ( 'NONE', #11272, #6451, #31513, .T. ) ;
#35967 = AXIS2_PLACEMENT_3D ( 'NONE', #29646, #35490, #27410 ) ;
#35968 = CARTESIAN_POINT ( 'NONE',  ( 74.99999662536835388, -25.98076211353319565, 17.49999999999999645 ) ) ;
#35969 = CARTESIAN_POINT ( 'NONE',  ( 46.99999662536851019, 77.94228634059959404, 12.50000000000000000 ) ) ;
#35970 = CARTESIAN_POINT ( 'NONE',  ( -73.00000337463099243, -25.98076211353322051, 12.50000000000000000 ) ) ;
#35971 = AXIS2_PLACEMENT_3D ( 'NONE', #36554, #13115, #30349 ) ;
#35972 = CARTESIAN_POINT ( 'NONE',  ( -90.52737013603423577, 71.16947008734744884, 32.50000000000000000 ) ) ;
#35973 = ORIENTED_EDGE ( 'NONE', *, *, #24447, .F. ) ;
#35974 = ORIENTED_EDGE ( 'NONE', *, *, #19018, .F. ) ;
#35975 = CARTESIAN_POINT ( 'NONE',  ( 5.000000000000000000, 0.9888715124523291822, -0.07061148569344767589 ) ) ;
#35976 = DIRECTION ( 'NONE',  ( 0.000000000000000000, 0.000000000000000000, 1.000000000000000000 ) ) ;
#35977 = ORIENTED_EDGE ( 'NONE', *, *, #34602, .T. ) ;
#35978 = CARTESIAN_POINT ( 'NONE',  ( 0.000000000000000000, 0.000000000000000000, 5.000000000000000000 ) ) ;
#35979 = VERTEX_POINT ( 'NONE', #13390 ) ;
#35980 = DIRECTION ( 'NONE',  ( 1.000000000000000000, 0.000000000000000000, 0.000000000000000000 ) ) ;
#35981 = EDGE_CURVE ( 'NONE', #35025, #4037, #7963, .T. ) ;
#35982 = CARTESIAN_POINT ( 'NONE',  ( 29.99999662536856349, 69.28203230275518365, -9.999999999999998224 ) ) ;
#35983 = EDGE_LOOP ( 'NONE', ( #3784, #1380 ) ) ;
#35984 = CARTESIAN_POINT ( 'NONE',  ( -0.03111943836866844226, 6.084399642271172581, -4.366192694417985187 ) ) ;
#35985 = EDGE_LOOP ( 'NONE', ( #30988, #17372 ) ) ;
#35986 = FACE_OUTER_BOUND ( 'NONE', #10530, .T. ) ;
#35987 = DIRECTION ( 'NONE',  ( 0.000000000000000000, 0.000000000000000000, 1.000000000000000000 ) ) ;
#35988 = DIRECTION ( 'NONE',  ( -1.000000000000000000, 1.798972493605576793E-15, 0.000000000000000000 ) ) ;
#35989 = AXIS2_PLACEMENT_3D ( 'NONE', #4877, #5239, #16676 ) ;
#35990 = ORIENTED_EDGE ( 'NONE', *, *, #33639, .F. ) ;
#35991 = DIRECTION ( 'NONE',  ( 1.000000000000000000, 0.000000000000000000, 0.000000000000000000 ) ) ;
#35992 = DIRECTION ( 'NONE',  ( 0.000000000000000000, 0.000000000000000000, 1.000000000000000000 ) ) ;
#35993 = CARTESIAN_POINT ( 'NONE',  ( 37.27962116909601065, -62.97617850287780072, -49.86561046011506448 ) ) ;
#35994 = VERTEX_POINT ( 'NONE', #5852 ) ;
#35995 = EDGE_LOOP ( 'NONE', ( #24867, #16323, #30585, #6211 ) ) ;
#35996 = EDGE_CURVE ( 'NONE', #26912, #902, #16404, .T. ) ;
#35997 = ORIENTED_EDGE ( 'NONE', *, *, #19426, .T. ) ;
#35998 = PLANE ( 'NONE',  #26027 ) ;
#35999 = DIRECTION ( 'NONE',  ( 0.000000000000000000, 0.000000000000000000, 1.000000000000000000 ) ) ;
#36000 = EDGE_CURVE ( 'NONE', #7804, #2324, #27289, .T. ) ;
#36001 = ORIENTED_EDGE ( 'NONE', *, *, #28659, .T. ) ;
#36002 = CARTESIAN_POINT ( 'NONE',  ( -73.00000337463099243, -25.98076211353322051, -9.999999999999998224 ) ) ;
#36003 = FACE_OUTER_BOUND ( 'NONE', #10720, .T. ) ;
#36004 = LINE ( 'NONE', #10298, #17639 ) ;
#36005 = EDGE_CURVE ( 'NONE', #21455, #6156, #2136, .T. ) ;
#36006 = FACE_OUTER_BOUND ( 'NONE', #30056, .T. ) ;
#36007 = DIRECTION ( 'NONE',  ( 0.000000000000000000, 0.000000000000000000, 1.000000000000000000 ) ) ;
#36008 = CARTESIAN_POINT ( 'NONE',  ( 87.99999662536828282, 2.449293598294703949E-16, 12.50000000000000000 ) ) ;
#36009 = ADVANCED_FACE ( 'NONE', ( #7597 ), #16594, .F. ) ;
#36010 = CARTESIAN_POINT ( 'NONE',  ( 11.99999662536861855, 69.28203230275516944, -9.999999999999998224 ) ) ;
#36011 = EDGE_CURVE ( 'NONE', #30228, #21906, #23090, .T. ) ;
#36012 = PLANE ( 'NONE',  #32819 ) ;
#36013 = ORIENTED_EDGE ( 'NONE', *, *, #11358, .F. ) ;
#36014 = ORIENTED_EDGE ( 'NONE', *, *, #31749, .F. ) ;
#36015 = LINE ( 'NONE', #7140, #24240 ) ;
#36016 = CARTESIAN_POINT ( 'NONE',  ( 3.000000000000000000, 0.000000000000000000, 0.000000000000000000 ) ) ;
#36017 = DIRECTION ( 'NONE',  ( -1.000000000000000000, 0.000000000000000000, 0.000000000000000000 ) ) ;
#36018 = CARTESIAN_POINT ( 'NONE',  ( 84.99999662536831124, -25.98076211353319565, -9.999999999999998224 ) ) ;
#36019 = ORIENTED_EDGE ( 'NONE', *, *, #17401, .F. ) ;
#36020 = ADVANCED_FACE ( 'NONE', ( #18852 ), #33090, .F. ) ;
#36021 = LINE ( 'NONE', #9755, #15956 ) ;
#36022 = EDGE_CURVE ( 'NONE', #5071, #30149, #7412, .T. ) ;
#36023 = DIRECTION ( 'NONE',  ( 1.000000000000000000, 0.000000000000000000, 0.000000000000000000 ) ) ;
#36024 = ADVANCED_FACE ( 'NONE', ( #25229 ), #8646, .F. ) ;
#36025 = DIRECTION ( 'NONE',  ( 1.000000000000000000, 0.000000000000000000, 0.000000000000000000 ) ) ;
#36026 = ORIENTED_EDGE ( 'NONE', *, *, #33247, .T. ) ;
#36027 = EDGE_CURVE ( 'NONE', #23649, #4478, #28490, .T. ) ;
#36028 = CARTESIAN_POINT ( 'NONE',  ( 4.999996625368676284, -77.94228634059960825, -9.999999999999998224 ) ) ;
#36029 = ORIENTED_EDGE ( 'NONE', *, *, #6046, .T. ) ;
#36030 = DIRECTION ( 'NONE',  ( 0.000000000000000000, 0.000000000000000000, 1.000000000000000000 ) ) ;
#36031 = CARTESIAN_POINT ( 'NONE',  ( 124.4080600076930665, -12.15049814296675201, 32.50000000000000000 ) ) ;
#36032 = DIRECTION ( 'NONE',  ( 0.000000000000000000, 0.000000000000000000, 1.000000000000000000 ) ) ;
#36033 = EDGE_LOOP ( 'NONE', ( #25905, #5923, #12461, #22111 ) ) ;
#36034 = VERTEX_POINT ( 'NONE', #27475 ) ;
#36035 = AXIS2_PLACEMENT_3D ( 'NONE', #27175, #21936, #27733 ) ;
#36036 = LINE ( 'NONE', #18967, #2407 ) ;
#36037 = ADVANCED_FACE ( 'NONE', ( #13224 ), #24671, .F. ) ;
#36038 = ORIENTED_EDGE ( 'NONE', *, *, #34134, .T. ) ;
#36039 = DIRECTION ( 'NONE',  ( 0.000000000000000000, 0.000000000000000000, 1.000000000000000000 ) ) ;
#36040 = FACE_OUTER_BOUND ( 'NONE', #27101, .T. ) ;
#36041 = CARTESIAN_POINT ( 'NONE',  ( -55.00000337463110611, -43.30127018922202353, 17.49999999999999645 ) ) ;
#36042 = DIRECTION ( 'NONE',  ( -1.000000000000000000, 0.000000000000000000, 0.000000000000000000 ) ) ;
#36043 = LINE ( 'NONE', #24781, #30894 ) ;
#36044 = ORIENTED_EDGE ( 'NONE', *, *, #24949, .F. ) ;
#36045 = DIRECTION ( 'NONE',  ( 0.000000000000000000, 0.000000000000000000, -1.000000000000000000 ) ) ;
#36046 = DIRECTION ( 'NONE',  ( 1.000000000000000000, 0.000000000000000000, 0.000000000000000000 ) ) ;
#36047 = DIRECTION ( 'NONE',  ( 0.000000000000000000, 0.000000000000000000, -1.000000000000000000 ) ) ;
#36048 = EDGE_LOOP ( 'NONE', ( #13463, #27476, #16344 ) ) ;
#36049 = DIRECTION ( 'NONE',  ( 1.000000000000000000, 0.000000000000000000, 0.000000000000000000 ) ) ;
#36050 = CARTESIAN_POINT ( 'NONE',  ( -65.00000337463104927, -43.30127018922202353, -5.000000000000000000 ) ) ;
#36051 = VERTEX_POINT ( 'NONE', #19050 ) ;
#36052 = VERTEX_POINT ( 'NONE', #30474 ) ;
#36053 = AXIS2_PLACEMENT_3D ( 'NONE', #20896, #24077, #32326 ) ;
#36054 = CYLINDRICAL_SURFACE ( 'NONE', #34292, 2.000000000000001776 ) ;
#36055 = FACE_OUTER_BOUND ( 'NONE', #19053, .T. ) ;
#36056 = DIRECTION ( 'NONE',  ( -1.000000000000000000, 0.000000000000000000, 0.000000000000000000 ) ) ;
#36057 = ORIENTED_EDGE ( 'NONE', *, *, #28400, .T. ) ;
#36058 = ORIENTED_EDGE ( 'NONE', *, *, #10289, .T. ) ;
#36059 = EDGE_LOOP ( 'NONE', ( #26264, #27303, #33389, #24707, #33477, #2390, #23175, #31878, #11147, #22996, #14705, #15044, #3911, #1, #32844, #12291, #24502, #35232, #35255, #21620, #18271, #4751, #33532, #36514 ) ) ;
#36060 = ADVANCED_FACE ( 'NONE', ( #4800 ), #10596, .T. ) ;
#36061 = DIRECTION ( 'NONE',  ( 0.000000000000000000, 0.000000000000000000, 1.000000000000000000 ) ) ;
#36062 = EDGE_CURVE ( 'NONE', #22987, #29936, #30646, .T. ) ;
#36063 = ORIENTED_EDGE ( 'NONE', *, *, #25666, .F. ) ;
#36064 = EDGE_CURVE ( 'NONE', #16030, #24141, #24901, .T. ) ;
#36065 = DIRECTION ( 'NONE',  ( -1.000000000000000000, 0.000000000000000000, 0.000000000000000000 ) ) ;
#36066 = ORIENTED_EDGE ( 'NONE', *, *, #33728, .F. ) ;
#36067 = EDGE_LOOP ( 'NONE', ( #19987, #4562, #34192, #23666, #3083, #5138 ) ) ;
#36068 = CARTESIAN_POINT ( 'NONE',  ( 34.99999662536853862, 77.94228634059959404, 17.49999999999999645 ) ) ;
#36069 = DIRECTION ( 'NONE',  ( 0.000000000000000000, 0.000000000000000000, 1.000000000000000000 ) ) ;
#36070 = ORIENTED_EDGE ( 'NONE', *, *, #32983, .F. ) ;
#36071 = ORIENTED_EDGE ( 'NONE', *, *, #1175, .T. ) ;
#36072 = CARTESIAN_POINT ( 'NONE',  ( 44.13139720814400135, -27.50000000000022737, 5.000000000000000888 ) ) ;
#36073 = CARTESIAN_POINT ( 'NONE',  ( -20.00000337463122690, 86.60254037844397601, -9.999999999999998224 ) ) ;
#36074 = DIRECTION ( 'NONE',  ( 1.000000000000000000, 0.000000000000000000, 0.000000000000000000 ) ) ;
#36075 = CARTESIAN_POINT ( 'NONE',  ( 37.99999662536853151, 69.28203230275518365, 12.50000000000000000 ) ) ;
#36076 = EDGE_LOOP ( 'NONE', ( #3886, #26231 ) ) ;
#36077 = DIRECTION ( 'NONE',  ( 0.000000000000000000, 0.000000000000000000, 1.000000000000000000 ) ) ;
#36078 = AXIS2_PLACEMENT_3D ( 'NONE', #23106, #3229, #17481 ) ;
#36079 = VERTEX_POINT ( 'NONE', #12002 ) ;
#36080 = CARTESIAN_POINT ( 'NONE',  ( 33.99999999999986500, -58.88972745734191250, 12.49999999999999822 ) ) ;
#36081 = CARTESIAN_POINT ( 'NONE',  ( 0.000000000000000000, 0.000000000000000000, 3.400000000000000355 ) ) ;
#36082 = CARTESIAN_POINT ( 'NONE',  ( 89.99999662536828282, 0.000000000000000000, -5.000000000000000000 ) ) ;
#36083 = DIRECTION ( 'NONE',  ( -1.000000000000000000, 0.000000000000000000, 0.000000000000000000 ) ) ;
#36084 = EDGE_CURVE ( 'NONE', #11718, #32638, #13505, .T. ) ;
#36085 = DIRECTION ( 'NONE',  ( 0.000000000000000000, 0.000000000000000000, 1.000000000000000000 ) ) ;
#36086 = CARTESIAN_POINT ( 'NONE',  ( 1.999996625368672287, 86.60254037844397601, -9.999999999999998224 ) ) ;
#36087 = CARTESIAN_POINT ( 'NONE',  ( 29.99999662536856349, 69.28203230275518365, -9.999999999999998224 ) ) ;
#36088 = VERTEX_POINT ( 'NONE', #757 ) ;
#36089 = DIRECTION ( 'NONE',  ( -1.000000000000000000, 0.000000000000000000, 0.000000000000000000 ) ) ;
#36090 = DIRECTION ( 'NONE',  ( 0.000000000000000000, 0.000000000000000000, 1.000000000000000000 ) ) ;
#36091 = DIRECTION ( 'NONE',  ( 0.000000000000000000, 0.000000000000000000, -1.000000000000000000 ) ) ;
#36092 = ORIENTED_EDGE ( 'NONE', *, *, #34655, .F. ) ;
#36093 =( BOUNDED_SURFACE ( )  B_SPLINE_SURFACE ( 3, 2, ( 
 ( #30971, #1917, #13341 ),
 ( #24991, #19351, #21783 ),
 ( #10905, #5098, #5302 ),
 ( #33615, #24799, #25186 ),
 ( #16541, #30217, #4920 ),
 ( #27971, #2293, #36611 ) ),
 .UNSPECIFIED., .F., .F., .F. ) 
 B_SPLINE_SURFACE_WITH_KNOTS ( ( 4, 2, 4 ),
 ( 3, 3 ),
 ( 0.002450104044831694170, 0.005591829551853678623, 0.008733555058875663510 ),
 ( 0.000000000000000000, 1.000000000000000000 ),
 .UNSPECIFIED. ) 
 GEOMETRIC_REPRESENTATION_ITEM ( )  RATIONAL_B_SPLINE_SURFACE ( (
 ( 1.000000000000000000, 0.8047731410850409439, 1.000000000000000000),
 ( 1.000000000000000000, 0.8125552299156232339, 1.000000000000000000),
 ( 1.000000000000000000, 0.8191520442889870246, 1.000000000000000000),
 ( 1.000000000000000000, 0.8191520442889870246, 1.000000000000000000),
 ( 1.000000000000000000, 0.8125552299156219016, 1.000000000000000000),
 ( 1.000000000000000000, 0.8047731410850398337, 1.000000000000000000) ) ) 
 REPRESENTATION_ITEM ( '' )  SURFACE ( )  );
#36094 = VECTOR ( 'NONE', #23494, 1000.000000000000000 ) ;
#36095 = ORIENTED_EDGE ( 'NONE', *, *, #20590, .F. ) ;
#36096 = VERTEX_POINT ( 'NONE', #23460 ) ;
#36097 = CARTESIAN_POINT ( 'NONE',  ( -45.00000337463112743, -60.62177826491080168, -9.999999999999998224 ) ) ;
#36098 = CARTESIAN_POINT ( 'NONE',  ( -3.374631303565411855E-06, -86.60254037844400443, 12.50000000000000000 ) ) ;
#36099 = ORIENTED_EDGE ( 'NONE', *, *, #33285, .F. ) ;
#36100 = DIRECTION ( 'NONE',  ( 0.000000000000000000, 0.000000000000000000, 1.000000000000000000 ) ) ;
#36101 = AXIS2_PLACEMENT_3D ( 'NONE', #20802, #26054, #6566 ) ;
#36102 = DIRECTION ( 'NONE',  ( 0.000000000000000000, 0.000000000000000000, 1.000000000000000000 ) ) ;
#36103 = EDGE_LOOP ( 'NONE', ( #16717, #22720 ) ) ;
#36104 = ADVANCED_FACE ( 'NONE', ( #29440, #6586, #18018, #17828, #23636, #20446, #26629, #35080, #18188, #6200, #25899, #35290, #28880, #17627 ), #14835, .T. ) ;
#36105 = AXIS2_PLACEMENT_3D ( 'NONE', #24659, #36091, #10388 ) ;
#36106 = FACE_BOUND ( 'NONE', #17687, .T. ) ;
#36107 = VERTEX_POINT ( 'NONE', #17459 ) ;
#36108 = DIRECTION ( 'NONE',  ( 0.000000000000000000, 0.000000000000000000, 1.000000000000000000 ) ) ;
#36109 = CARTESIAN_POINT ( 'NONE',  ( 0.000000000000000000, -1.467624384280027172, 2.542000000000001592 ) ) ;
#36110 = DIRECTION ( 'NONE',  ( 0.000000000000000000, 0.000000000000000000, 1.000000000000000000 ) ) ;
#36111 = CYLINDRICAL_SURFACE ( 'NONE', #3798, 2.000000000000001776 ) ;
#36112 = EDGE_LOOP ( 'NONE', ( #19529, #13140, #33796, #9334 ) ) ;
#36113 = CARTESIAN_POINT ( 'NONE',  ( -85.00000337463092137, -8.660254037844422825, -9.999999999999998224 ) ) ;
#36114 = DIRECTION ( 'NONE',  ( -1.000000000000000000, 0.000000000000000000, 0.000000000000000000 ) ) ;
#36115 = CYLINDRICAL_SURFACE ( 'NONE', #22434, 30.00000000000000000 ) ;
#36116 = AXIS2_PLACEMENT_3D ( 'NONE', #7693, #28286, #2247 ) ;
#36117 = EDGE_LOOP ( 'NONE', ( #8768, #14973 ) ) ;
#36118 = DIRECTION ( 'NONE',  ( 0.000000000000000000, 1.224646799147351482E-16, 1.000000000000000000 ) ) ;
#36119 = DIRECTION ( 'NONE',  ( 1.000000000000000000, 0.000000000000000000, 0.000000000000000000 ) ) ;
#36120 = ORIENTED_EDGE ( 'NONE', *, *, #27169, .T. ) ;
#36121 = DIRECTION ( 'NONE',  ( 1.000000000000000000, 0.000000000000000000, 0.000000000000000000 ) ) ;
#36122 = DIRECTION ( 'NONE',  ( 0.000000000000000000, 0.000000000000000000, 1.000000000000000000 ) ) ;
#36123 = PLANE ( 'NONE',  #8777 ) ;
#36124 = EDGE_CURVE ( 'NONE', #8997, #15428, #35714, .T. ) ;
#36125 = VERTEX_POINT ( 'NONE', #15195 ) ;
#36126 = AXIS2_PLACEMENT_3D ( 'NONE', #15271, #10025, #1223 ) ;
#36127 = VERTEX_POINT ( 'NONE', #29062 ) ;
#36128 = EDGE_CURVE ( 'NONE', #15570, #2260, #3203, .T. ) ;
#36129 = CARTESIAN_POINT ( 'NONE',  ( 3.750000000000001776, 0.000000000000000000, 3.400000000000000355 ) ) ;
#36130 = CARTESIAN_POINT ( 'NONE',  ( -42.00000337463114164, -69.28203230275519786, 17.49999999999999645 ) ) ;
#36131 = CARTESIAN_POINT ( 'NONE',  ( 106.7731239591682026, -98.28784258493070070, 32.50000000000000000 ) ) ;
#36133 = EDGE_CURVE ( 'NONE', #29875, #12814, #26079, .T. ) ;
#36132 = ORIENTED_EDGE ( 'NONE', *, *, #30860, .F. ) ;
#36134 = ORIENTED_EDGE ( 'NONE', *, *, #19432, .T. ) ;
#36135 = DIRECTION ( 'NONE',  ( -1.000000000000000000, -1.798972493605577187E-15, 0.000000000000000000 ) ) ;
#36136 = CARTESIAN_POINT ( 'NONE',  ( -2.991272306860052410, 4.046490820311134939, -0.5592653008974223239 ) ) ;
#36137 = CARTESIAN_POINT ( 'NONE',  ( -60.00000337463107059, -34.64101615137762025, -5.000000000000000000 ) ) ;
#36138 = CIRCLE ( 'NONE', #6167, 4.999999999999997335 ) ;
#36139 = CARTESIAN_POINT ( 'NONE',  ( -104.5389608366994167, 58.87775083094626183, 32.49999999999999289 ) ) ;
#36140 = ORIENTED_EDGE ( 'NONE', *, *, #8299, .T. ) ;
#36141 = ORIENTED_EDGE ( 'NONE', *, *, #12809, .F. ) ;
#36142 = CIRCLE ( 'NONE', #13372, 2.000000000000001776 ) ;
#36143 = CARTESIAN_POINT ( 'NONE',  ( 4.999999999999997335, 0.000000000000000000, 0.000000000000000000 ) ) ;
#36144 = DIRECTION ( 'NONE',  ( 1.000000000000000000, 0.000000000000000000, 0.000000000000000000 ) ) ;
#36145 = ORIENTED_EDGE ( 'NONE', *, *, #11886, .T. ) ;
#36146 = EDGE_CURVE ( 'NONE', #23895, #26782, #8837, .T. ) ;
#36147 = CARTESIAN_POINT ( 'NONE',  ( 86.99999662536831124, -8.660254037844397956, 12.50000000000000000 ) ) ;
#36148 = VERTEX_POINT ( 'NONE', #20279 ) ;
#36149 = DIRECTION ( 'NONE',  ( 1.000000000000000000, 0.000000000000000000, 0.000000000000000000 ) ) ;
#36150 = LINE ( 'NONE', #36346, #22121 ) ;
#36151 = ORIENTED_EDGE ( 'NONE', *, *, #22724, .T. ) ;
#36152 = CIRCLE ( 'NONE', #19981, 2.000000000000000000 ) ;
#36153 = CARTESIAN_POINT ( 'NONE',  ( 5.284804376168104945, 3.015249596956811384, -4.366192694417979858 ) ) ;
#36154 = VERTEX_POINT ( 'NONE', #34727 ) ;
#36155 = FILL_AREA_STYLE_COLOUR ( '', #32089 ) ;
#36156 = EDGE_CURVE ( 'NONE', #34191, #16233, #25595, .T. ) ;
#36157 = FACE_OUTER_BOUND ( 'NONE', #32672, .T. ) ;
#36158 = LINE ( 'NONE', #7854, #25754 ) ;
#36159 = CARTESIAN_POINT ( 'NONE',  ( 19.99999662536861678, -86.60254037844400443, -5.000000000000000000 ) ) ;
#36160 = ADVANCED_FACE ( 'NONE', ( #26275 ), #21014, .F. ) ;
#36161 = VERTEX_POINT ( 'NONE', #6755 ) ;
#36162 = CARTESIAN_POINT ( 'NONE',  ( 76.99999662536836809, 8.660254037844394404, -5.000000000000000000 ) ) ;
#36163 = DIRECTION ( 'NONE',  ( 0.000000000000000000, 0.000000000000000000, 1.000000000000000000 ) ) ;
#36164 = CARTESIAN_POINT ( 'NONE',  ( 4.999996625368645198, 77.94228634059957983, -9.999999999999998224 ) ) ;
#36165 = ORIENTED_EDGE ( 'NONE', *, *, #35597, .F. ) ;
#36166 = ADVANCED_FACE ( 'NONE', ( #31704 ), #14467, .T. ) ;
#36167 = ORIENTED_EDGE ( 'NONE', *, *, #2186, .T. ) ;
#36168 = AXIS2_PLACEMENT_3D ( 'NONE', #37068, #28413, #16990 ) ;
#36169 = ORIENTED_EDGE ( 'NONE', *, *, #36604, .T. ) ;
#36170 = DIRECTION ( 'NONE',  ( 0.000000000000000000, 0.000000000000000000, 1.000000000000000000 ) ) ;
#36171 = VERTEX_POINT ( 'NONE', #15389 ) ;
#36172 = EDGE_CURVE ( 'NONE', #3095, #18828, #36021, .T. ) ;
#36173 = CARTESIAN_POINT ( 'NONE',  ( -59.29837256189559724, -31.02796211690927919, 12.49999999999999822 ) ) ;
#36174 = CARTESIAN_POINT ( 'NONE',  ( 67.99999662536838230, 17.32050807568879236, -5.000000000000000000 ) ) ;
#36175 = VECTOR ( 'NONE', #20290, 1000.000000000000000 ) ;
#36176 = CARTESIAN_POINT ( 'NONE',  ( 0.000000000000000000, -1.467624384280032501, -2.541999999999998483 ) ) ;
#36177 = ADVANCED_FACE ( 'NONE', ( #7322 ), #33180, .F. ) ;
#36178 = VECTOR ( 'NONE', #14274, 1000.000000000000000 ) ;
#36179 = DIRECTION ( 'NONE',  ( -0.000000000000000000, -0.000000000000000000, 1.000000000000000000 ) ) ;
#36180 = DIRECTION ( 'NONE',  ( 0.000000000000000000, 0.000000000000000000, -1.000000000000000000 ) ) ;
#36181 = LINE ( 'NONE', #1868, #6606 ) ;
#36182 = DIRECTION ( 'NONE',  ( -1.000000000000000000, -0.000000000000000000, -0.000000000000000000 ) ) ;
#36183 = CARTESIAN_POINT ( 'NONE',  ( -68.00000337463102085, -34.64101615137762025, -9.999999999999998224 ) ) ;
#36184 = ORIENTED_EDGE ( 'NONE', *, *, #7859, .F. ) ;
#36185 = ORIENTED_EDGE ( 'NONE', *, *, #16870, .F. ) ;
#36186 = CARTESIAN_POINT ( 'NONE',  ( -3.374631327851540519E-06, 86.60254037844397601, -9.999999999999998224 ) ) ;
#36187 = CARTESIAN_POINT ( 'NONE',  ( 3.000000000000000000, 1.467624384280024730, -2.542000000000001592 ) ) ;
#36188 = CARTESIAN_POINT ( 'NONE',  ( -53.00000337463110611, -43.30127018922202353, 17.49999999999999645 ) ) ;
#36189 = LINE ( 'NONE', #21937, #15502 ) ;
#36190 = ORIENTED_EDGE ( 'NONE', *, *, #6901, .T. ) ;
#36191 = CYLINDRICAL_SURFACE ( 'NONE', #28488, 2.000000000000001776 ) ;
#36192 = AXIS2_PLACEMENT_3D ( 'NONE', #25818, #20524, #23373 ) ;
#36193 = EDGE_CURVE ( 'NONE', #26406, #9668, #19545, .T. ) ;
#36194 = DIRECTION ( 'NONE',  ( 0.000000000000000000, 0.000000000000000000, -1.000000000000000000 ) ) ;
#36195 = ORIENTED_EDGE ( 'NONE', *, *, #2, .T. ) ;
#36196 = DIRECTION ( 'NONE',  ( -0.000000000000000000, 0.8660254037844391517, 0.4999999999999990563 ) ) ;
#36197 = EDGE_LOOP ( 'NONE', ( #26978, #18903, #26856, #33116 ) ) ;
#36198 = LINE ( 'NONE', #10320, #33512 ) ;
#36199 = AXIS2_PLACEMENT_3D ( 'NONE', #35475, #14643, #18025 ) ;
#36200 = EDGE_CURVE ( 'NONE', #11967, #7273, #15758, .T. ) ;
#36201 = CARTESIAN_POINT ( 'NONE',  ( 72.77422209630368855, 61.06482292022033675, -5.000000000000000000 ) ) ;
#36202 = VECTOR ( 'NONE', #19135, 1000.000000000000000 ) ;
#36203 = CARTESIAN_POINT ( 'NONE',  ( -72.00000337463102085, -34.64101615137762025, -5.000000000000000000 ) ) ;
#36204 = EDGE_CURVE ( 'NONE', #35706, #7403, #24929, .T. ) ;
#36205 = ORIENTED_EDGE ( 'NONE', *, *, #31123, .T. ) ;
#36206 = EDGE_LOOP ( 'NONE', ( #17047, #27934, #27828, #14342 ) ) ;
#36207 = EDGE_CURVE ( 'NONE', #9828, #1926, #30320, .T. ) ;
#36208 = ORIENTED_EDGE ( 'NONE', *, *, #3807, .T. ) ;
#36210 = DIRECTION ( 'NONE',  ( 1.000000000000000000, 0.000000000000000000, 0.000000000000000000 ) ) ;
#36209 = VECTOR ( 'NONE', #14064, 1000.000000000000000 ) ;
#36211 = DIRECTION ( 'NONE',  ( 0.000000000000000000, 0.000000000000000000, -1.000000000000000000 ) ) ;
#36212 = CIRCLE ( 'NONE', #30198, 2.000000000000001776 ) ;
#36213 = DIRECTION ( 'NONE',  ( 0.000000000000000000, 0.000000000000000000, 1.000000000000000000 ) ) ;
#36214 = CARTESIAN_POINT ( 'NONE',  ( 56.99999662536846046, -43.30127018922200222, -5.000000000000000000 ) ) ;
#36215 = DIRECTION ( 'NONE',  ( 0.000000000000000000, 0.000000000000000000, 1.000000000000000000 ) ) ;
#36216 = VERTEX_POINT ( 'NONE', #27179 ) ;
#36217 = CARTESIAN_POINT ( 'NONE',  ( -106.7731239591695669, -98.28784258492920856, 32.55002500000000509 ) ) ;
#36218 = AXIS2_PLACEMENT_3D ( 'NONE', #20076, #34336, #36778 ) ;
#36219 = DIRECTION ( 'NONE',  ( 0.000000000000000000, 0.000000000000000000, -1.000000000000000000 ) ) ;
#36220 = EDGE_CURVE ( 'NONE', #5553, #21436, #5169, .T. ) ;
#36221 = ORIENTED_EDGE ( 'NONE', *, *, #19233, .T. ) ;
#36222 = DIRECTION ( 'NONE',  ( 1.000000000000000000, 0.000000000000000000, 0.000000000000000000 ) ) ;
#36223 = DIRECTION ( 'NONE',  ( 1.000000000000000000, 0.000000000000000000, 0.000000000000000000 ) ) ;
#36224 = AXIS2_PLACEMENT_3D ( 'NONE', #29973, #12530, #9905 ) ;
#36225 = VERTEX_POINT ( 'NONE', #24393 ) ;
#36226 = AXIS2_PLACEMENT_3D ( 'NONE', #5611, #34690, #11777 ) ;
#36227 = VECTOR ( 'NONE', #10986, 1000.000000000000000 ) ;
#36228 = ORIENTED_EDGE ( 'NONE', *, *, #10098, .T. ) ;
#36229 = CARTESIAN_POINT ( 'NONE',  ( 0.000000000000000000, 0.000000000000000000, -5.000000000000000000 ) ) ;
#36230 = DIRECTION ( 'NONE',  ( 0.000000000000000000, 0.000000000000000000, 1.000000000000000000 ) ) ;
#36231 = DIRECTION ( 'NONE',  ( 0.000000000000000000, 0.000000000000000000, 1.000000000000000000 ) ) ;
#36232 = VERTEX_POINT ( 'NONE', #35839 ) ;
#36233 = EDGE_LOOP ( 'NONE', ( #36657, #2873 ) ) ;
#36234 = ORIENTED_EDGE ( 'NONE', *, *, #7039, .F. ) ;
#36235 = CARTESIAN_POINT ( 'NONE',  ( -20.00000337463122690, 86.60254037844397601, -9.999999999999998224 ) ) ;
#36236 = EDGE_CURVE ( 'NONE', #14671, #8160, #3954, .T. ) ;
#36237 = VECTOR ( 'NONE', #28860, 1000.000000000000000 ) ;
#36238 = ORIENTED_EDGE ( 'NONE', *, *, #15861, .T. ) ;
#36239 = EDGE_CURVE ( 'NONE', #31490, #29904, #984, .T. ) ;
#36240 = VECTOR ( 'NONE', #19425, 1000.000000000000000 ) ;
#36241 = FACE_BOUND ( 'NONE', #4117, .T. ) ;
#36242 = VERTEX_POINT ( 'NONE', #10147 ) ;
#36243 = ORIENTED_EDGE ( 'NONE', *, *, #6993, .F. ) ;
#36244 = EDGE_CURVE ( 'NONE', #14173, #6793, #8165, .T. ) ;
#36245 = AXIS2_PLACEMENT_3D ( 'NONE', #32572, #17415, #3887 ) ;
#36246 = FACE_OUTER_BOUND ( 'NONE', #22698, .T. ) ;
#36247 = FACE_OUTER_BOUND ( 'NONE', #20587, .T. ) ;
#36248 = VERTEX_POINT ( 'NONE', #27380 ) ;
#36249 = VERTEX_POINT ( 'NONE', #7501 ) ;
#36250 = ADVANCED_FACE ( 'NONE', ( #33007 ), #30374, .T. ) ;
#36251 = DIRECTION ( 'NONE',  ( 0.000000000000000000, 0.000000000000000000, 1.000000000000000000 ) ) ;
#36252 = CYLINDRICAL_SURFACE ( 'NONE', #2787, 2.000000000000001776 ) ;
#36253 = EDGE_CURVE ( 'NONE', #34519, #13060, #33916, .T. ) ;
#36254 = CIRCLE ( 'NONE', #12863, 2.000000000000001776 ) ;
#36255 = DIRECTION ( 'NONE',  ( 1.000000000000000000, 0.000000000000000000, 0.000000000000000000 ) ) ;
#36256 = CIRCLE ( 'NONE', #36836, 2.000000000000001776 ) ;
#36257 = CARTESIAN_POINT ( 'NONE',  ( 59.99999662536843914, -34.64101615137759893, -9.999999999999998224 ) ) ;
#36258 = VERTEX_POINT ( 'NONE', #32621 ) ;
#36259 = LINE ( 'NONE', #30243, #11723 ) ;
#36260 = FACE_BOUND ( 'NONE', #3762, .T. ) ;
#36261 = CARTESIAN_POINT ( 'NONE',  ( 71.99999662536839651, 17.32050807568879236, 12.50000000000000000 ) ) ;
#36262 = LINE ( 'NONE', #7388, #5815 ) ;
#36263 = CARTESIAN_POINT ( 'NONE',  ( -83.00000337463092137, 25.98076211353317433, -9.999999999999998224 ) ) ;
#36264 = EDGE_CURVE ( 'NONE', #33803, #28072, #29102, .T. ) ;
#36265 = DIRECTION ( 'NONE',  ( 1.000000000000000000, 0.000000000000000000, 0.000000000000000000 ) ) ;
#36266 = EDGE_CURVE ( 'NONE', #30829, #9726, #12334, .T. ) ;
#36267 = CYLINDRICAL_SURFACE ( 'NONE', #25768, 2.000000000000001776 ) ;
#36268 = ADVANCED_FACE ( 'NONE', ( #4079 ), #318, .F. ) ;
#36269 = CIRCLE ( 'NONE', #13496, 2.541999999999999815 ) ;
#36270 = EDGE_CURVE ( 'NONE', #34308, #20758, #33328, .T. ) ;
#36271 = DIRECTION ( 'NONE',  ( 1.000000000000000000, 0.000000000000000000, 0.000000000000000000 ) ) ;
#36272 = VERTEX_POINT ( 'NONE', #23770 ) ;
#36274 = AXIS2_PLACEMENT_3D ( 'NONE', #34923, #9217, #20649 ) ;
#36273 = DIRECTION ( 'NONE',  ( 1.000000000000000000, 0.000000000000000000, 0.000000000000000000 ) ) ;
#36275 = LINE ( 'NONE', #24658, #958 ) ;
#36276 = DIRECTION ( 'NONE',  ( 0.000000000000000000, 0.000000000000000000, -1.000000000000000000 ) ) ;
#36277 = CIRCLE ( 'NONE', #13504, 2.000000000000000000 ) ;
#36278 = AXIS2_PLACEMENT_3D ( 'NONE', #22039, #7792, #19234 ) ;
#36279 = VERTEX_POINT ( 'NONE', #21129 ) ;
#36280 = AXIS2_PLACEMENT_3D ( 'NONE', #33333, #10443, #13077 ) ;
#36281 = ORIENTED_EDGE ( 'NONE', *, *, #659, .T. ) ;
#36282 = VERTEX_POINT ( 'NONE', #6875 ) ;
#36283 = DIRECTION ( 'NONE',  ( 0.000000000000000000, 0.000000000000000000, 1.000000000000000000 ) ) ;
#36284 = DIRECTION ( 'NONE',  ( -3.554796214472773777E-16, -1.000000000000000000, 0.000000000000000000 ) ) ;
#36285 = EDGE_LOOP ( 'NONE', ( #4516, #36066, #12139, #12858, #33929 ) ) ;
#36286 = VECTOR ( 'NONE', #4996, 1000.000000000000000 ) ;
#36287 = CARTESIAN_POINT ( 'NONE',  ( -25.00000337463121980, -77.94228634059963667, -5.000000000000000000 ) ) ;
#36288 = CARTESIAN_POINT ( 'NONE',  ( 37.50000000000000000, 103.4105893997321743, -19.99999999999999645 ) ) ;
#36289 = EDGE_LOOP ( 'NONE', ( #1202, #10790 ) ) ;
#36290 = LINE ( 'NONE', #7599, #15582 ) ;
#36291 = ORIENTED_EDGE ( 'NONE', *, *, #19520, .F. ) ;
#36292 = FACE_BOUND ( 'NONE', #28426, .T. ) ;
#36293 = AXIS2_PLACEMENT_3D ( 'NONE', #7569, #36077, #1566 ) ;
#36294 = CARTESIAN_POINT ( 'NONE',  ( -0.4079457818577069683, 5.537975084925943037, -5.689399939901069736 ) ) ;
#36295 = DIRECTION ( 'NONE',  ( 1.000000000000000000, 0.000000000000000000, 0.000000000000000000 ) ) ;
#36296 = VECTOR ( 'NONE', #610, 1000.000000000000000 ) ;
#36297 = CARTESIAN_POINT ( 'NONE',  ( -2.000003374631289521, -69.28203230275519786, -9.999999999999998224 ) ) ;
#36298 = CIRCLE ( 'NONE', #27284, 25.00000000000000000 ) ;
#36299 = ORIENTED_EDGE ( 'NONE', *, *, #26374, .F. ) ;
#36300 = DIRECTION ( 'NONE',  ( 1.000000000000000000, 0.000000000000000000, 0.000000000000000000 ) ) ;
#36301 = AXIS2_PLACEMENT_3D ( 'NONE', #6945, #4150, #9943 ) ;
#36302 = VECTOR ( 'NONE', #13020, 1000.000000000000114 ) ;
#36303 = DIRECTION ( 'NONE',  ( -0.000000000000000000, -0.000000000000000000, 1.000000000000000000 ) ) ;
#36304 = LINE ( 'NONE', #16417, #8069 ) ;
#36305 = AXIS2_PLACEMENT_3D ( 'NONE', #6406, #26462, #23654 ) ;
#36306 = ORIENTED_EDGE ( 'NONE', *, *, #12116, .F. ) ;
#36307 = DIRECTION ( 'NONE',  ( 0.000000000000000000, 0.000000000000000000, -1.000000000000000000 ) ) ;
#36308 = DIRECTION ( 'NONE',  ( 1.000000000000000000, 0.000000000000000000, 0.000000000000000000 ) ) ;
#36309 = ORIENTED_EDGE ( 'NONE', *, *, #21590, .T. ) ;
#36310 = LINE ( 'NONE', #33678, #31607 ) ;
#36311 = PLANE ( 'NONE',  #20862 ) ;
#36312 = DIRECTION ( 'NONE',  ( 0.000000000000000000, 0.000000000000000000, -1.000000000000000000 ) ) ;
#36313 =( BOUNDED_SURFACE ( )  B_SPLINE_SURFACE ( 3, 2, ( 
 ( #26580, #893, #12314 ),
 ( #35239, #20970, #32398 ),
 ( #15334, #33337, #4660 ),
 ( #7453, #18712, #16448 ),
 ( #13083, #22092, #27329 ),
 ( #7844, #32966, #24540 ) ),
 .UNSPECIFIED., .F., .F., .T. ) 
 B_SPLINE_SURFACE_WITH_KNOTS ( ( 4, 2, 4 ),
 ( 3, 3 ),
 ( 0.002450104044831698507, 0.005591829551853683827, 0.008733555058875668714 ),
 ( 0.000000000000000000, 1.000000000000000000 ),
 .UNSPECIFIED. ) 
 GEOMETRIC_REPRESENTATION_ITEM ( )  RATIONAL_B_SPLINE_SURFACE ( (
 ( 1.000000000000000000, 0.8047731410850408329, 1.000000000000000000),
 ( 1.000000000000000000, 0.8125552299152700719, 1.000000000000000000),
 ( 1.000000000000000000, 0.8191520442894577592, 1.000000000000000000),
 ( 1.000000000000000000, 0.8191520442885167341, 1.000000000000000000),
 ( 1.000000000000000000, 0.8125552299159767289, 1.000000000000000000),
 ( 1.000000000000000000, 0.8047731410850399447, 1.000000000000000000) ) ) 
 REPRESENTATION_ITEM ( '' )  SURFACE ( )  );
#36314 = AXIS2_PLACEMENT_3D ( 'NONE', #8750, #34441, #31075 ) ;
#36315 = EDGE_LOOP ( 'NONE', ( #31015, #33377 ) ) ;
#36316 = EDGE_CURVE ( 'NONE', #29025, #13349, #34665, .T. ) ;
#36317 = VERTEX_POINT ( 'NONE', #35222 ) ;
#36318 = DIRECTION ( 'NONE',  ( 0.000000000000000000, 0.000000000000000000, 1.000000000000000000 ) ) ;
#36319 = DIRECTION ( 'NONE',  ( 1.000000000000000000, 0.000000000000000000, 0.000000000000000000 ) ) ;
#36320 = CIRCLE ( 'NONE', #26724, 2.000000000000001776 ) ;
#36321 = CARTESIAN_POINT ( 'NONE',  ( -68.00000337463099243, 34.64101615137758472, -9.999999999999998224 ) ) ;
#36322 = ORIENTED_EDGE ( 'NONE', *, *, #32059, .F. ) ;
#36323 = VERTEX_POINT ( 'NONE', #29744 ) ;
#36324 = VECTOR ( 'NONE', #21770, 1000.000000000000114 ) ;
#36325 = LINE ( 'NONE', #27863, #33782 ) ;
#36326 = CARTESIAN_POINT ( 'NONE',  ( -65.00000337463106348, -60.62177826491083010, -5.000000000000000000 ) ) ;
#36327 = PRODUCT_DEFINITION_FORMATION_WITH_SPECIFIED_SOURCE ( 'ANY', '', #11249, .NOT_KNOWN. ) ;
#36328 = FACE_OUTER_BOUND ( 'NONE', #574, .T. ) ;
#36329 = CIRCLE ( 'NONE', #2191, 2.000000000000001776 ) ;
#36330 = AXIS2_PLACEMENT_3D ( 'NONE', #25755, #17645, #36997 ) ;
#36331 = CARTESIAN_POINT ( 'NONE',  ( -98.00091034470435147, 66.93791212686957692, 32.50000000000000711 ) ) ;
#36332 = AXIS2_PLACEMENT_3D ( 'NONE', #35939, #29924, #4618 ) ;
#36333 = ORIENTED_EDGE ( 'NONE', *, *, #3445, .F. ) ;
#36334 = AXIS2_PLACEMENT_3D ( 'NONE', #8091, #34169, #30767 ) ;
#36335 = EDGE_LOOP ( 'NONE', ( #6293, #14669 ) ) ;
#36336 = DIRECTION ( 'NONE',  ( 0.000000000000000000, 0.000000000000000000, 1.000000000000000000 ) ) ;
#36337 = CIRCLE ( 'NONE', #13570, 2.000000000000001776 ) ;
#36338 = DIRECTION ( 'NONE',  ( 0.000000000000000000, 0.000000000000000000, 1.000000000000000000 ) ) ;
#36339 = ORIENTED_EDGE ( 'NONE', *, *, #6085, .F. ) ;
#36340 = CARTESIAN_POINT ( 'NONE',  ( -60.00000337463104216, 34.64101615137757051, -9.999999999999998224 ) ) ;
#36341 = ORIENTED_EDGE ( 'NONE', *, *, #16973, .T. ) ;
#36342 = DIRECTION ( 'NONE',  ( 0.000000000000000000, 0.000000000000000000, 1.000000000000000000 ) ) ;
#36343 = EDGE_CURVE ( 'NONE', #29568, #31223, #20123, .T. ) ;
#36344 = EDGE_CURVE ( 'NONE', #27555, #1358, #29693, .T. ) ;
#36345 = CIRCLE ( 'NONE', #27919, 2.445500000000000007 ) ;
#36346 = CARTESIAN_POINT ( 'NONE',  ( 3.000000000000000000, 1.467624384280024730, -2.542000000000001592 ) ) ;
#36347 = CARTESIAN_POINT ( 'NONE',  ( 21.99999662536857770, 86.60254037844397601, -9.999999999999998224 ) ) ;
#36348 = EDGE_LOOP ( 'NONE', ( #8636, #34373, #20132, #34517, #19662, #19784, #13176, #9016 ) ) ;
#36349 = CARTESIAN_POINT ( 'NONE',  ( 59.99999662536843914, -34.64101615137759893, -9.999999999999998224 ) ) ;
#36350 = EDGE_CURVE ( 'NONE', #36323, #31828, #34498, .T. ) ;
#36351 = AXIS2_PLACEMENT_3D ( 'NONE', #10297, #24369, #21729 ) ;
#36352 = CARTESIAN_POINT ( 'NONE',  ( -30.00000337463118427, 69.28203230275516944, -5.000000000000000000 ) ) ;
#36353 = CARTESIAN_POINT ( 'NONE',  ( -75.00000337463097821, 43.30127018922197379, 17.49999999999999645 ) ) ;
#36354 = EDGE_LOOP ( 'NONE', ( #18569, #36888 ) ) ;
#36355 = CARTESIAN_POINT ( 'NONE',  ( 47.99999662536846756, -69.28203230275519786, -9.999999999999998224 ) ) ;
#36356 = DIRECTION ( 'NONE',  ( 1.000000000000000000, 0.000000000000000000, 0.000000000000000000 ) ) ;
#36357 = DIRECTION ( 'NONE',  ( 0.000000000000000000, 0.000000000000000000, 1.000000000000000000 ) ) ;
#36358 = VERTEX_POINT ( 'NONE', #31807 ) ;
#36359 = VECTOR ( 'NONE', #24498, 1000.000000000000000 ) ;
#36360 = CIRCLE ( 'NONE', #33980, 2.000000000000001776 ) ;
#36361 = ORIENTED_EDGE ( 'NONE', *, *, #15153, .T. ) ;
#36362 = AXIS2_PLACEMENT_3D ( 'NONE', #36137, #24705, #21695 ) ;
#36363 = AXIS2_PLACEMENT_3D ( 'NONE', #18470, #9264, #34967 ) ;
#36364 = EDGE_LOOP ( 'NONE', ( #35841, #28172, #17043, #14996 ) ) ;
#36365 = EDGE_CURVE ( 'NONE', #34263, #32378, #6141, .T. ) ;
#36366 = CARTESIAN_POINT ( 'NONE',  ( 74.99999662536835388, -43.30127018922199511, -9.999999999999998224 ) ) ;
#36367 = VERTEX_POINT ( 'NONE', #3327 ) ;
#36368 = CARTESIAN_POINT ( 'NONE',  ( -5.000000000000000000, -2.886751345948134428, -2.080000000000000071 ) ) ;
#36369 = CARTESIAN_POINT ( 'NONE',  ( -85.00000337463092137, 8.660254037844389075, 12.50000000000000000 ) ) ;
#36370 = CIRCLE ( 'NONE', #1610, 2.000000000000001776 ) ;
#36371 = DIRECTION ( 'NONE',  ( 1.000000000000000000, 0.000000000000000000, 0.000000000000000000 ) ) ;
#36372 = CARTESIAN_POINT ( 'NONE',  ( -44.13139720814380240, 27.50000000000055422, -15.00000000000000000 ) ) ;
#36373 = CARTESIAN_POINT ( 'NONE',  ( -19.31922176934808633, 76.99660315353983719, 18.49999999999999645 ) ) ;
#36374 = CARTESIAN_POINT ( 'NONE',  ( 40.99999999999999289, -103.4105893997321743, 27.50000000000000000 ) ) ;
#36375 = CARTESIAN_POINT ( 'NONE',  ( 31.99999662536857770, -69.28203230275519786, -9.999999999999998224 ) ) ;
#36376 = CARTESIAN_POINT ( 'NONE',  ( -10.00000337463127842, -69.28203230275519786, 17.49999999999999645 ) ) ;
#36377 = EDGE_LOOP ( 'NONE', ( #20633, #2103 ) ) ;
#36378 = AXIS2_PLACEMENT_3D ( 'NONE', #24609, #27590, #6769 ) ;
#36379 = ORIENTED_EDGE ( 'NONE', *, *, #34402, .F. ) ;
#36380 = DIRECTION ( 'NONE',  ( 0.000000000000000000, 0.000000000000000000, 1.000000000000000000 ) ) ;
#36381 = ADVANCED_FACE ( 'NONE', ( #14763 ), #18327, .F. ) ;
#36382 = DIRECTION ( 'NONE',  ( -0.000000000000000000, -0.000000000000000000, -1.000000000000000000 ) ) ;
#36383 = CYLINDRICAL_SURFACE ( 'NONE', #14442, 2.000000000000001776 ) ;
#36384 = CARTESIAN_POINT ( 'NONE',  ( 37.50000000000000000, 103.4105893997321743, 27.49999999999999645 ) ) ;
#36385 = ORIENTED_EDGE ( 'NONE', *, *, #16650, .F. ) ;
#36386 = AXIS2_PLACEMENT_3D ( 'NONE', #23340, #9247, #6255 ) ;
#36387 = VECTOR ( 'NONE', #3536, 1000.000000000000000 ) ;
#36388 = CARTESIAN_POINT ( 'NONE',  ( 72.99999662536835388, -25.98076211353319565, -9.999999999999998224 ) ) ;
#36389 = VECTOR ( 'NONE', #28218, 1000.000000000000000 ) ;
#36390 = CARTESIAN_POINT ( 'NONE',  ( 69.99999662536839651, 34.64101615137758472, 17.49999999999999645 ) ) ;
#36391 = ORIENTED_EDGE ( 'NONE', *, *, #2176, .F. ) ;
#36392 = EDGE_CURVE ( 'NONE', #6626, #7555, #26563, .T. ) ;
#36393 = DIRECTION ( 'NONE',  ( 0.000000000000000000, 0.000000000000000000, 1.000000000000000000 ) ) ;
#36394 = ORIENTED_EDGE ( 'NONE', *, *, #11654, .F. ) ;
#36395 = AXIS2_PLACEMENT_3D ( 'NONE', #30302, #26940, #33307 ) ;
#36396 = DIRECTION ( 'NONE',  ( 1.000000000000000000, 0.000000000000000000, 0.000000000000000000 ) ) ;
#36397 = CARTESIAN_POINT ( 'NONE',  ( 84.99999662536831124, -25.98076211353319565, 17.49999999999999645 ) ) ;
#36398 = DIRECTION ( 'NONE',  ( -1.000000000000000000, 0.000000000000000000, 0.000000000000000000 ) ) ;
#36399 = EDGE_CURVE ( 'NONE', #30228, #26119, #522, .T. ) ;
#36400 = CIRCLE ( 'NONE', #4057, 2.000000000000000000 ) ;
#36401 = DIRECTION ( 'NONE',  ( -1.000000000000000000, 0.000000000000000000, 0.000000000000000000 ) ) ;
#36402 = VERTEX_POINT ( 'NONE', #9316 ) ;
#36403 = ORIENTED_EDGE ( 'NONE', *, *, #22280, .T. ) ;
#36404 = CIRCLE ( 'NONE', #23812, 33.00000000000001421 ) ;
#36405 = VECTOR ( 'NONE', #33598, 1000.000000000000000 ) ;
#36406 = AXIS2_PLACEMENT_3D ( 'NONE', #19919, #28894, #3223 ) ;
#36407 = VECTOR ( 'NONE', #26477, 1000.000000000000000 ) ;
#36408 = ORIENTED_EDGE ( 'NONE', *, *, #13435, .F. ) ;
#36409 = DIRECTION ( 'NONE',  ( 0.000000000000000000, 0.000000000000000000, 1.000000000000000000 ) ) ;
#36410 = CARTESIAN_POINT ( 'NONE',  ( -83.47442710120355969, 31.09745072740822991, -49.86348611802629449 ) ) ;
#36411 = CARTESIAN_POINT ( 'NONE',  ( 4.390739357591696154E-15, -5.773502691896305272, -3.984345921091785758 ) ) ;
#36412 = DIRECTION ( 'NONE',  ( 1.000000000000000000, 0.000000000000000000, 0.000000000000000000 ) ) ;
#36413 = ORIENTED_EDGE ( 'NONE', *, *, #34071, .F. ) ;
#36414 = DIRECTION ( 'NONE',  ( -0.7071067811865486830, 8.659560562354947649E-17, 0.7071067811865464625 ) ) ;
#36415 = CIRCLE ( 'NONE', #16687, 2.999999999999999556 ) ;
#36416 = ADVANCED_FACE ( 'NONE', ( #34835 ), #6699, .F. ) ;
#36417 = CARTESIAN_POINT ( 'NONE',  ( -5.000003374631269537, -77.94228634059960825, -9.999999999999998224 ) ) ;
#36418 = DIRECTION ( 'NONE',  ( 0.000000000000000000, 0.000000000000000000, 1.000000000000000000 ) ) ;
#36419 = ORIENTED_EDGE ( 'NONE', *, *, #11721, .T. ) ;
#36420 = FACE_OUTER_BOUND ( 'NONE', #28840, .T. ) ;
#36421 = CARTESIAN_POINT ( 'NONE',  ( 78.38501592334911550, 33.46125459406803060, -5.000000000000000000 ) ) ;
#36422 = AXIS2_PLACEMENT_3D ( 'NONE', #2378, #17171, #22240 ) ;
#36423 = ORIENTED_EDGE ( 'NONE', *, *, #1074, .F. ) ;
#36424 = EDGE_CURVE ( 'NONE', #27540, #11751, #20727, .T. ) ;
#36425 = ORIENTED_EDGE ( 'NONE', *, *, #31654, .T. ) ;
#36426 = CARTESIAN_POINT ( 'NONE',  ( 19.99999662536861678, -86.60254037844400443, -9.999999999999998224 ) ) ;
#36427 = VECTOR ( 'NONE', #8112, 1000.000000000000000 ) ;
#36428 = EDGE_CURVE ( 'NONE', #9125, #4, #32386, .T. ) ;
#36429 = DIRECTION ( 'NONE',  ( 1.000000000000000000, 0.000000000000000000, 0.000000000000000000 ) ) ;
#36430 = DIRECTION ( 'NONE',  ( 0.000000000000000000, -0.000000000000000000, 1.000000000000000000 ) ) ;
#36431 = CARTESIAN_POINT ( 'NONE',  ( -3.101151694651716806, -3.983051926191232717, -0.6020238742160465284 ) ) ;
#36432 = VERTEX_POINT ( 'NONE', #29551 ) ;
#36433 = ORIENTED_EDGE ( 'NONE', *, *, #5491, .T. ) ;
#36434 = AXIS2_PLACEMENT_3D ( 'NONE', #25329, #21962, #36764 ) ;
#36435 = CIRCLE ( 'NONE', #21433, 2.000000000000001776 ) ;
#36436 = CYLINDRICAL_SURFACE ( 'NONE', #20672, 2.000000000000001776 ) ;
#36437 = VERTEX_POINT ( 'NONE', #20751 ) ;
#36438 = DIRECTION ( 'NONE',  ( 1.000000000000000000, 0.000000000000000000, -0.000000000000000000 ) ) ;
#36439 = ORIENTED_EDGE ( 'NONE', *, *, #29809, .T. ) ;
#36440 = ORIENTED_EDGE ( 'NONE', *, *, #8002, .F. ) ;
#36441 = DIRECTION ( 'NONE',  ( 0.000000000000000000, 0.000000000000000000, 1.000000000000000000 ) ) ;
#36442 = EDGE_CURVE ( 'NONE', #14753, #12497, #3874, .T. ) ;
#36443 = CARTESIAN_POINT ( 'NONE',  ( 0.000000000000000000, 0.000000000000000000, 12.49999999999999822 ) ) ;
#36444 = ORIENTED_EDGE ( 'NONE', *, *, #2045, .T. ) ;
#36445 = ORIENTED_EDGE ( 'NONE', *, *, #11688, .F. ) ;
#36446 = DIRECTION ( 'NONE',  ( 1.000000000000000000, 0.000000000000000000, 0.000000000000000000 ) ) ;
#36447 = AXIS2_PLACEMENT_3D ( 'NONE', #8852, #8661, #2667 ) ;
#36448 = CYLINDRICAL_SURFACE ( 'NONE', #27315, 2.000000000000001776 ) ;
#36449 = CARTESIAN_POINT ( 'NONE',  ( 46.99999662536849598, -77.94228634059960825, -5.000000000000000000 ) ) ;
#36450 = CARTESIAN_POINT ( 'NONE',  ( -85.00000337463092137, 25.98076211353317433, 12.50000000000000000 ) ) ;
#36451 = ORIENTED_EDGE ( 'NONE', *, *, #4497, .F. ) ;
#36452 = CYLINDRICAL_SURFACE ( 'NONE', #6377, 2.000000000000001776 ) ;
#36453 = VECTOR ( 'NONE', #28484, 1000.000000000000000 ) ;
#36454 = FACE_BOUND ( 'NONE', #37100, .T. ) ;
#36455 = CIRCLE ( 'NONE', #30479, 5.750000000000002665 ) ;
#36456 = CARTESIAN_POINT ( 'NONE',  ( 82.99999662536831124, -8.660254037844397956, 12.50000000000000000 ) ) ;
#36457 = DIRECTION ( 'NONE',  ( -1.000000000000000000, 0.000000000000000000, 0.000000000000000000 ) ) ;
#36458 = LINE ( 'NONE', #15823, #36846 ) ;
#36459 = CARTESIAN_POINT ( 'NONE',  ( 5.248988766908545323, -2.532174945215652340, -4.266961984436639099 ) ) ;
#36460 = EDGE_CURVE ( 'NONE', #20259, #15438, #11153, .T. ) ;
#36461 = LINE ( 'NONE', #28008, #27553 ) ;
#36462 = AXIS2_PLACEMENT_3D ( 'NONE', #5593, #17409, #12111 ) ;
#36463 = DIRECTION ( 'NONE',  ( 1.000000000000000000, 0.000000000000000000, 0.000000000000000000 ) ) ;
#36464 = VERTEX_POINT ( 'NONE', #23963 ) ;
#36465 = EDGE_CURVE ( 'NONE', #31031, #16370, #36906, .T. ) ;
#36466 = DIRECTION ( 'NONE',  ( 0.000000000000000000, 0.000000000000000000, 1.000000000000000000 ) ) ;
#36467 = DIRECTION ( 'NONE',  ( 0.000000000000000000, 0.000000000000000000, 1.000000000000000000 ) ) ;
#36468 = DIRECTION ( 'NONE',  ( 0.000000000000000000, 0.000000000000000000, 1.000000000000000000 ) ) ;
#36469 = ORIENTED_EDGE ( 'NONE', *, *, #32842, .T. ) ;
#36470 = EDGE_CURVE ( 'NONE', #12555, #9993, #15878, .T. ) ;
#36471 = AXIS2_PLACEMENT_3D ( 'NONE', #26099, #11839, #966 ) ;
#36472 = VERTEX_POINT ( 'NONE', #29945 ) ;
#36473 = EDGE_LOOP ( 'NONE', ( #13737, #23808, #31525 ) ) ;
#36474 = CARTESIAN_POINT ( 'NONE',  ( 12.99999662536859901, 77.94228634059957983, 17.49999999999999645 ) ) ;
#36475 = DIRECTION ( 'NONE',  ( 0.000000000000000000, 0.000000000000000000, 1.000000000000000000 ) ) ;
#36476 = EDGE_CURVE ( 'NONE', #24345, #16958, #26762, .T. ) ;
#36477 = EDGE_LOOP ( 'NONE', ( #22998, #26944, #1783 ) ) ;
#36478 = ADVANCED_FACE ( 'NONE', ( #18878 ), #21869, .F. ) ;
#36479 = PRODUCT_DEFINITION_SHAPE ( 'NONE', 'NONE',  #37126 ) ;
#36480 = DIRECTION ( 'NONE',  ( 0.000000000000000000, 0.000000000000000000, 1.000000000000000000 ) ) ;
#36481 = VECTOR ( 'NONE', #1288, 1000.000000000000000 ) ;
#36482 = CARTESIAN_POINT ( 'NONE',  ( -47.00000337463111322, -77.94228634059960825, -9.999999999999998224 ) ) ;
#36483 = VERTEX_POINT ( 'NONE', #30309 ) ;
#36484 = CARTESIAN_POINT ( 'NONE',  ( 110.2237710830529664, -101.7384897088154929, 32.50000000000000000 ) ) ;
#36485 = VERTEX_POINT ( 'NONE', #27506 ) ;
#36486 = CIRCLE ( 'NONE', #18522, 2.000000000000001776 ) ;
#36487 = CARTESIAN_POINT ( 'NONE',  ( -67.00000337463104927, -43.30127018922202353, -9.999999999999998224 ) ) ;
#36488 = EDGE_CURVE ( 'NONE', #8851, #36088, #3397, .T. ) ;
#36489 = EDGE_CURVE ( 'NONE', #18239, #16233, #13416, .T. ) ;
#36490 = DIRECTION ( 'NONE',  ( 0.000000000000000000, 0.000000000000000000, 1.000000000000000000 ) ) ;
#36491 = CARTESIAN_POINT ( 'NONE',  ( 3.499999647538293512, -4.028415724610473703, -4.085927688751840314 ) ) ;
#36492 = ADVANCED_FACE ( 'NONE', ( #16079 ), #30116, .T. ) ;
#36493 = EDGE_CURVE ( 'NONE', #26110, #9484, #22073, .T. ) ;
#36494 = AXIS2_PLACEMENT_3D ( 'NONE', #436, #6442, #5902 ) ;
#36495 =( REPRESENTATION_RELATIONSHIP ('NONE','NONE', #15268, #33474 ) REPRESENTATION_RELATIONSHIP_WITH_TRANSFORMATION ( #1248 )SHAPE_REPRESENTATION_RELATIONSHIP( ) );
#36496 = ADVANCED_FACE ( 'NONE', ( #21311 ), #35583, .F. ) ;
#36497 = VERTEX_POINT ( 'NONE', #10076 ) ;
#36498 = CYLINDRICAL_SURFACE ( 'NONE', #18293, 2.000000000000001776 ) ;
#36499 = CIRCLE ( 'NONE', #552, 2.000000000000001776 ) ;
#36500 = DIRECTION ( 'NONE',  ( 0.000000000000000000, 0.000000000000000000, -1.000000000000000000 ) ) ;
#36501 = CARTESIAN_POINT ( 'NONE',  ( -10.00000337463127842, -69.28203230275519786, -9.999999999999998224 ) ) ;
#36502 = AXIS2_PLACEMENT_3D ( 'NONE', #14038, #11421, #28290 ) ;
#36503 = ORIENTED_EDGE ( 'NONE', *, *, #35676, .T. ) ;
#36504 = DIRECTION ( 'NONE',  ( 1.000000000000000000, 0.000000000000000000, 0.000000000000000000 ) ) ;
#36505 = CARTESIAN_POINT ( 'NONE',  ( 49.99999662536846756, 51.96152422706637708, -9.999999999999998224 ) ) ;
#36506 = ORIENTED_EDGE ( 'NONE', *, *, #36604, .F. ) ;
#36507 = AXIS2_PLACEMENT_3D ( 'NONE', #23530, #15654, #13013 ) ;
#36508 = FACE_OUTER_BOUND ( 'NONE', #27998, .T. ) ;
#36509 = DIRECTION ( 'NONE',  ( 0.000000000000000000, 0.000000000000000000, 1.000000000000000000 ) ) ;
#36510 = DIRECTION ( 'NONE',  ( 0.8660254037844344888, -0.5000000000000069944, 0.000000000000000000 ) ) ;
#36511 = CIRCLE ( 'NONE', #2382, 2.000000000000001776 ) ;
#36512 = VERTEX_POINT ( 'NONE', #36129 ) ;
#36513 = AXIS2_PLACEMENT_3D ( 'NONE', #7983, #7814, #10618 ) ;
#36514 = ORIENTED_EDGE ( 'NONE', *, *, #33002, .F. ) ;
#36515 = AXIS2_PLACEMENT_3D ( 'NONE', #32976, #30147, #19116 ) ;
#36516 = CARTESIAN_POINT ( 'NONE',  ( 0.000000000000000000, 0.000000000000000000, -5.000000000000000000 ) ) ;
#36517 = DIRECTION ( 'NONE',  ( 1.000000000000000000, 0.000000000000000000, 0.000000000000000000 ) ) ;
#36518 = CARTESIAN_POINT ( 'NONE',  ( -89.27079897466127534, 32.49191361593859995, -5.000000000000000000 ) ) ;
#36519 = ORIENTED_EDGE ( 'NONE', *, *, #37103, .F. ) ;
#36520 = EDGE_LOOP ( 'NONE', ( #1487, #12157, #34777 ) ) ;
#36521 = PLANE ( 'NONE',  #24794 ) ;
#36522 = DIRECTION ( 'NONE',  ( -0.000000000000000000, -0.000000000000000000, 1.000000000000000000 ) ) ;
#36523 = CARTESIAN_POINT ( 'NONE',  ( -2.448772250512182280E-15, 99.94802294027086020, 27.49999999999999645 ) ) ;
#36524 = AXIS2_PLACEMENT_3D ( 'NONE', #30094, #16406, #18854 ) ;
#36525 = ORIENTED_EDGE ( 'NONE', *, *, #14456, .T. ) ;
#36526 = VERTEX_POINT ( 'NONE', #10629 ) ;
#36527 = CARTESIAN_POINT ( 'NONE',  ( 84.99999662536831124, -25.98076211353319565, -9.999999999999998224 ) ) ;
#36528 = CIRCLE ( 'NONE', #8966, 3.000000000000002665 ) ;
#36529 = CARTESIAN_POINT ( 'NONE',  ( 29.99999662536856349, 69.28203230275518365, -5.000000000000000000 ) ) ;
#36530 = ORIENTED_EDGE ( 'NONE', *, *, #17633, .F. ) ;
#36531 = AXIS2_PLACEMENT_3D ( 'NONE', #15610, #6972, #33208 ) ;
#36532 = DIRECTION ( 'NONE',  ( 0.000000000000000000, 0.000000000000000000, 1.000000000000000000 ) ) ;
#36533 = EDGE_LOOP ( 'NONE', ( #18996, #22432, #2356, #4155 ) ) ;
#36535 = AXIS2_PLACEMENT_3D ( 'NONE', #13203, #24648, #15647 ) ;
#36534 = DIRECTION ( 'NONE',  ( 1.000000000000000000, 0.000000000000000000, 0.000000000000000000 ) ) ;
#36536 = EDGE_CURVE ( 'NONE', #4653, #22919, #6981, .T. ) ;
#36537 = DIRECTION ( 'NONE',  ( 0.000000000000000000, 0.000000000000000000, -1.000000000000000000 ) ) ;
#36538 = AXIS2_PLACEMENT_3D ( 'NONE', #15261, #26698, #12061 ) ;
#36539 = EDGE_CURVE ( 'NONE', #21337, #31907, #27118, .T. ) ;
#36540 = AXIS2_PLACEMENT_3D ( 'NONE', #9510, #17556, #29541 ) ;
#36541 = CARTESIAN_POINT ( 'NONE',  ( -17.00000337463125533, -77.94228634059960825, -9.999999999999998224 ) ) ;
#36542 = ORIENTED_EDGE ( 'NONE', *, *, #10615, .T. ) ;
#36543 = CARTESIAN_POINT ( 'NONE',  ( -108.3061974404900951, -19.22934205794868490, -26.00000000000000000 ) ) ;
#36544 = DIRECTION ( 'NONE',  ( 0.000000000000000000, 0.000000000000000000, -1.000000000000000000 ) ) ;
#36545 = DIRECTION ( 'NONE',  ( 0.000000000000000000, 0.000000000000000000, 1.000000000000000000 ) ) ;
#36546 = DIRECTION ( 'NONE',  ( 0.000000000000000000, 0.000000000000000000, -1.000000000000000000 ) ) ;
#36547 = ORIENTED_EDGE ( 'NONE', *, *, #33235, .T. ) ;
#36548 = DIRECTION ( 'NONE',  ( 0.000000000000000000, 0.000000000000000000, 1.000000000000000000 ) ) ;
#36549 = DIRECTION ( 'NONE',  ( 1.000000000000000000, 0.000000000000000000, 0.000000000000000000 ) ) ;
#36550 = LINE ( 'NONE', #7861, #24932 ) ;
#36551 = AXIS2_PLACEMENT_3D ( 'NONE', #31209, #7966, #25591 ) ;
#36552 = ORIENTED_EDGE ( 'NONE', *, *, #14752, .F. ) ;
#36553 = ORIENTED_EDGE ( 'NONE', *, *, #12974, .T. ) ;
#36554 = CARTESIAN_POINT ( 'NONE',  ( 0.000000000000000000, 0.000000000000000000, -5.000000000000000000 ) ) ;
#36555 = ORIENTED_EDGE ( 'NONE', *, *, #17941, .F. ) ;
#36556 = CARTESIAN_POINT ( 'NONE',  ( -65.00000337463104927, -25.98076211353322051, -9.999999999999998224 ) ) ;
#36557 = DIRECTION ( 'NONE',  ( -0.000000000000000000, -0.000000000000000000, -1.000000000000000000 ) ) ;
#36558 = EDGE_CURVE ( 'NONE', #32142, #1362, #33314, .T. ) ;
#36559 = CARTESIAN_POINT ( 'NONE',  ( -35.19434990244938888, 52.39915983220783602, 12.49999999999999822 ) ) ;
#36560 = CIRCLE ( 'NONE', #9597, 27.00000000000001421 ) ;
#36561 = CARTESIAN_POINT ( 'NONE',  ( 41.00000000000000000, 103.4105893997321743, -19.99999999999999645 ) ) ;
#36562 = CARTESIAN_POINT ( 'NONE',  ( 49.99999662536846756, -69.28203230275519786, -9.999999999999998224 ) ) ;
#36563 = CARTESIAN_POINT ( 'NONE',  ( 5.999999999999999112, 3.980102097228899218E-16, 3.250000000000001332 ) ) ;
#36564 = CARTESIAN_POINT ( 'NONE',  ( -5.321755965770424296E-15, 5.914763229585211946, -4.281769937709103857 ) ) ;
#36565 = DIRECTION ( 'NONE',  ( 0.000000000000000000, 0.000000000000000000, 1.000000000000000000 ) ) ;
#36566 = ORIENTED_EDGE ( 'NONE', *, *, #7335, .F. ) ;
#36567 = VERTEX_POINT ( 'NONE', #1627 ) ;
#36568 = ADVANCED_FACE ( 'NONE', ( #7632 ), #13063, .F. ) ;
#36569 = LINE ( 'NONE', #28662, #26649 ) ;
#36570 = CARTESIAN_POINT ( 'NONE',  ( -57.00000337463107059, 60.62177826491078747, -9.999999999999998224 ) ) ;
#36571 = DIRECTION ( 'NONE',  ( 1.000000000000000000, -0.000000000000000000, 0.000000000000000000 ) ) ;
#36572 = CIRCLE ( 'NONE', #26364, 2.000000000000001776 ) ;
#36573 = CARTESIAN_POINT ( 'NONE',  ( 46.74665512060159500, 61.59603906214631763, 12.50000000000000000 ) ) ;
#36574 = ORIENTED_EDGE ( 'NONE', *, *, #25000, .F. ) ;
#36575 = UNCERTAINTY_MEASURE_WITH_UNIT (LENGTH_MEASURE( 1.000000000000000082E-05 ), #26051, 'distance_accuracy_value', 'NONE');
#36576 = DIRECTION ( 'NONE',  ( -1.000000000000000000, 0.000000000000000000, 0.000000000000000000 ) ) ;
#36577 = ORIENTED_EDGE ( 'NONE', *, *, #31258, .T. ) ;
#36578 = VERTEX_POINT ( 'NONE', #7263 ) ;
#36579 = TOROIDAL_SURFACE ( 'NONE', #35391, 3.250000000000001332, 0.2500000000000000000 ) ;
#36580 = ADVANCED_FACE ( 'NONE', ( #4830 ), #24316, .T. ) ;
#36581 = DIRECTION ( 'NONE',  ( 1.000000000000000000, 0.000000000000000000, 0.000000000000000000 ) ) ;
#36582 = ORIENTED_EDGE ( 'NONE', *, *, #31871, .T. ) ;
#36583 = DIRECTION ( 'NONE',  ( -0.000000000000000000, -0.000000000000000000, 1.000000000000000000 ) ) ;
#36584 = DIRECTION ( 'NONE',  ( 0.000000000000000000, 0.000000000000000000, -1.000000000000000000 ) ) ;
#36585 = DIRECTION ( 'NONE',  ( 0.000000000000000000, 0.000000000000000000, -1.000000000000000000 ) ) ;
#36586 = ORIENTED_EDGE ( 'NONE', *, *, #6260, .T. ) ;
#36587 = ORIENTED_EDGE ( 'NONE', *, *, #14222, .F. ) ;
#36588 = ORIENTED_EDGE ( 'NONE', *, *, #15111, .T. ) ;
#36589 = ORIENTED_EDGE ( 'NONE', *, *, #16986, .T. ) ;
#36590 = DIRECTION ( 'NONE',  ( 0.000000000000000000, 0.000000000000000000, -1.000000000000000000 ) ) ;
#36591 = EDGE_CURVE ( 'NONE', #691, #6247, #33518, .T. ) ;
#36592 = CARTESIAN_POINT ( 'NONE',  ( 6.000000000000000000, -145.0000000000000568, 27.50000000000000000 ) ) ;
#36593 = LINE ( 'NONE', #24973, #464 ) ;
#36594 = CARTESIAN_POINT ( 'NONE',  ( 24.99999662536859546, -77.94228634059960825, 12.50000000000000000 ) ) ;
#36595 = DIRECTION ( 'NONE',  ( 0.000000000000000000, 0.000000000000000000, 1.000000000000000000 ) ) ;
#36596 = EDGE_CURVE ( 'NONE', #2284, #3385, #14765, .T. ) ;
#36597 = ORIENTED_EDGE ( 'NONE', *, *, #20734, .T. ) ;
#36598 = CARTESIAN_POINT ( 'NONE',  ( 0.000000000000000000, 0.000000000000000000, 12.49999999999999822 ) ) ;
#36599 = DIRECTION ( 'NONE',  ( -1.000000000000000000, 0.000000000000000000, 0.000000000000000000 ) ) ;
#36600 = AXIS2_PLACEMENT_3D ( 'NONE', #4490, #26814, #32809 ) ;
#36601 = FACE_OUTER_BOUND ( 'NONE', #29192, .T. ) ;
#36602 = VERTEX_POINT ( 'NONE', #22618 ) ;
#36603 = DIRECTION ( 'NONE',  ( -0.000000000000000000, -0.000000000000000000, 1.000000000000000000 ) ) ;
#36604 = EDGE_CURVE ( 'NONE', #24335, #13777, #37062, .T. ) ;
#36605 = DIRECTION ( 'NONE',  ( 0.7071067811865435759, -0.7071067811865514585, 0.000000000000000000 ) ) ;
#36606 = ORIENTED_EDGE ( 'NONE', *, *, #30519, .T. ) ;
#36607 = ORIENTED_EDGE ( 'NONE', *, *, #7147, .F. ) ;
#36608 = ADVANCED_FACE ( 'NONE', ( #25626 ), #8379, .F. ) ;
#36609 = DIRECTION ( 'NONE',  ( -1.000000000000000000, 0.000000000000000000, 0.000000000000000000 ) ) ;
#36610 = CARTESIAN_POINT ( 'NONE',  ( -3.401922400366804045, 3.809401878282542064, -3.971474537231016733 ) ) ;
#36611 = CARTESIAN_POINT ( 'NONE',  ( -0.2117491801717885924, -5.895756138069174312, -4.027903350935069682 ) ) ;
#36612 = CARTESIAN_POINT ( 'NONE',  ( -1.642566673137934696, -4.825166380998203053, -0.07080520455423977566 ) ) ;
#36613 = ORIENTED_EDGE ( 'NONE', *, *, #475, .F. ) ;
#36614 = EDGE_LOOP ( 'NONE', ( #19384, #32847, #13170, #11079 ) ) ;
#36615 = DIRECTION ( 'NONE',  ( 1.000000000000000000, 0.000000000000000000, 0.000000000000000000 ) ) ;
#36616 = ORIENTED_EDGE ( 'NONE', *, *, #23047, .T. ) ;
#36617 = ADVANCED_FACE ( 'NONE', ( #19625 ), #16429, .F. ) ;
#36618 = CIRCLE ( 'NONE', #6686, 2.000000000000001776 ) ;
#36619 = DIRECTION ( 'NONE',  ( 0.000000000000000000, 0.000000000000000000, 1.000000000000000000 ) ) ;
#36620 = ORIENTED_EDGE ( 'NONE', *, *, #11316, .T. ) ;
#36621 = EDGE_LOOP ( 'NONE', ( #69, #597 ) ) ;
#36622 = EDGE_CURVE ( 'NONE', #27142, #4841, #22814, .T. ) ;
#36623 = LINE ( 'NONE', #16753, #29812 ) ;
#36624 = FACE_OUTER_BOUND ( 'NONE', #30647, .T. ) ;
#36625 = ORIENTED_EDGE ( 'NONE', *, *, #4999, .T. ) ;
#36626 = VERTEX_POINT ( 'NONE', #27854 ) ;
#36627 = CARTESIAN_POINT ( 'NONE',  ( 3.499999999999991562, 55.00000000000000000, -5.000000000000000000 ) ) ;
#36628 = DIRECTION ( 'NONE',  ( 0.000000000000000000, 0.000000000000000000, 1.000000000000000000 ) ) ;
#36629 = EDGE_CURVE ( 'NONE', #1500, #575, #2179, .T. ) ;
#36630 = DIRECTION ( 'NONE',  ( 0.000000000000000000, 0.000000000000000000, 1.000000000000000000 ) ) ;
#36631 = CYLINDRICAL_SURFACE ( 'NONE', #10713, 2.000000000000001776 ) ;
#36632 = EDGE_LOOP ( 'NONE', ( #5204, #25079, #6706, #13579, #7094 ) ) ;
#36633 = DIRECTION ( 'NONE',  ( 0.000000000000000000, 0.000000000000000000, 1.000000000000000000 ) ) ;
#36634 = EDGE_CURVE ( 'NONE', #25705, #8997, #29134, .T. ) ;
#36635 = FACE_BOUND ( 'NONE', #11137, .T. ) ;
#36636 = CARTESIAN_POINT ( 'NONE',  ( 9.999996625368625658, 86.60254037844397601, -5.000000000000000000 ) ) ;
#36637 = DIRECTION ( 'NONE',  ( 0.000000000000000000, 0.000000000000000000, -1.000000000000000000 ) ) ;
#36638 = CARTESIAN_POINT ( 'NONE',  ( 3.000000000000000000, -2.935248768560059229, 3.469446951953614189E-15 ) ) ;
#36639 = CYLINDRICAL_SURFACE ( 'NONE', #36852, 2.000000000000001776 ) ;
#36640 = CARTESIAN_POINT ( 'NONE',  ( -50.00000337463109190, 51.96152422706637708, -9.999999999999998224 ) ) ;
#36641 = AXIS2_PLACEMENT_3D ( 'NONE', #35520, #35702, #9646 ) ;
#36642 = DIRECTION ( 'NONE',  ( 0.000000000000000000, 0.000000000000000000, 1.000000000000000000 ) ) ;
#36643 = ORIENTED_EDGE ( 'NONE', *, *, #26774, .T. ) ;
#36644 = DIRECTION ( 'NONE',  ( -1.000000000000000000, 0.000000000000000000, 0.000000000000000000 ) ) ;
#36645 = EDGE_CURVE ( 'NONE', #14671, #16872, #20617, .T. ) ;
#36646 = CARTESIAN_POINT ( 'NONE',  ( 14.99999662536859901, 77.94228634059957983, -9.999999999999998224 ) ) ;
#36647 = CARTESIAN_POINT ( 'NONE',  ( 0.3000000000000016542, 0.000000000000000000, 0.000000000000000000 ) ) ;
#36648 = VERTEX_POINT ( 'NONE', #5738 ) ;
#36649 = ORIENTED_EDGE ( 'NONE', *, *, #15831, .F. ) ;
#36650 = ORIENTED_EDGE ( 'NONE', *, *, #14639, .F. ) ;
#36651 = EDGE_CURVE ( 'NONE', #35050, #12167, #31056, .T. ) ;
#36652 = DIRECTION ( 'NONE',  ( -0.5000000000000094369, -0.8660254037844332675, 0.000000000000000000 ) ) ;
#36653 = CYLINDRICAL_SURFACE ( 'NONE', #1083, 2.000000000000001776 ) ;
#36654 = EDGE_LOOP ( 'NONE', ( #21050, #19148 ) ) ;
#36655 = CARTESIAN_POINT ( 'NONE',  ( -68.66839587347244844, -56.74224907229007187, -49.22241343995298024 ) ) ;
#36656 = DIRECTION ( 'NONE',  ( 0.000000000000000000, 0.000000000000000000, 1.000000000000000000 ) ) ;
#36657 = ORIENTED_EDGE ( 'NONE', *, *, #2088, .T. ) ;
#36658 = CARTESIAN_POINT ( 'NONE',  ( 86.99999662536831124, -25.98076211353319565, 17.49999999999999645 ) ) ;
#36659 = ORIENTED_EDGE ( 'NONE', *, *, #19497, .F. ) ;
#36660 = DIRECTION ( 'NONE',  ( 1.000000000000000000, 0.000000000000000000, 0.000000000000000000 ) ) ;
#36661 = ADVANCED_FACE ( 'NONE', ( #8727 ), #22984, .T. ) ;
#36662 = DIRECTION ( 'NONE',  ( 0.4999999999999919509, -0.8660254037844432595, 0.000000000000000000 ) ) ;
#36663 = CARTESIAN_POINT ( 'NONE',  ( 66.00000000000000000, 0.000000000000000000, 0.000000000000000000 ) ) ;
#36664 = EDGE_LOOP ( 'NONE', ( #4425, #37065, #31833, #10644 ) ) ;
#36665 = DIRECTION ( 'NONE',  ( 1.000000000000000000, 1.792547591842699744E-15, 0.000000000000000000 ) ) ;
#36666 = EDGE_CURVE ( 'NONE', #36697, #15333, #15985, .T. ) ;
#36667 = CARTESIAN_POINT ( 'NONE',  ( -78.00000337463094979, -17.32050807568882078, 12.50000000000000000 ) ) ;
#36668 = DIRECTION ( 'NONE',  ( -1.000000000000000000, 0.000000000000000000, 0.000000000000000000 ) ) ;
#36669 = VERTEX_POINT ( 'NONE', #7992 ) ;
#36670 = DIRECTION ( 'NONE',  ( 0.000000000000000000, 0.000000000000000000, -1.000000000000000000 ) ) ;
#36671 = DIRECTION ( 'NONE',  ( 1.000000000000000000, 0.000000000000000000, 0.000000000000000000 ) ) ;
#36673 = ORIENTED_EDGE ( 'NONE', *, *, #3928, .T. ) ;
#36672 = ADVANCED_FACE ( 'NONE', ( #19430 ), #28407, .T. ) ;
#36674 = DIRECTION ( 'NONE',  ( -1.000000000000000000, 0.000000000000000000, 0.000000000000000000 ) ) ;
#36675 = ADVANCED_FACE ( 'NONE', ( #30849 ), #36683, .F. ) ;
#36676 = CARTESIAN_POINT ( 'NONE',  ( 34.99999662536853862, 77.94228634059959404, 12.50000000000000000 ) ) ;
#36677 = CARTESIAN_POINT ( 'NONE',  ( -3.374631303565411855E-06, -86.60254037844400443, 17.49999999999999645 ) ) ;
#36678 = DIRECTION ( 'NONE',  ( -1.000000000000000000, -0.000000000000000000, -0.000000000000000000 ) ) ;
#36679 = CIRCLE ( 'NONE', #22130, 33.00000000000001421 ) ;
#36680 = AXIS2_PLACEMENT_3D ( 'NONE', #36977, #30602, #33785 ) ;
#36681 = EDGE_LOOP ( 'NONE', ( #25625, #17134, #14536, #6578, #36616 ) ) ;
#36682 = ORIENTED_EDGE ( 'NONE', *, *, #18911, .F. ) ;
#36683 = CYLINDRICAL_SURFACE ( 'NONE', #25566, 2.000000000000001776 ) ;
#36684 = DIRECTION ( 'NONE',  ( 1.000000000000000000, 0.000000000000000000, 0.000000000000000000 ) ) ;
#36685 = ORIENTED_EDGE ( 'NONE', *, *, #17656, .F. ) ;
#36686 = ORIENTED_EDGE ( 'NONE', *, *, #26583, .F. ) ;
#36687 = ADVANCED_FACE ( 'NONE', ( #25255 ), #22419, .F. ) ;
#36688 = AXIS2_PLACEMENT_3D ( 'NONE', #14268, #3183, #8624 ) ;
#36689 = CARTESIAN_POINT ( 'NONE',  ( 0.000000000000000000, 0.000000000000000000, -15.00000000000000000 ) ) ;
#36690 = CARTESIAN_POINT ( 'NONE',  ( -2.381231458764688558, 4.398698068175660225, -0.5078976954042897507 ) ) ;
#36691 = LINE ( 'NONE', #11538, #33966 ) ;
#36692 = ORIENTED_EDGE ( 'NONE', *, *, #17611, .T. ) ;
#36693 = ORIENTED_EDGE ( 'NONE', *, *, #28199, .F. ) ;
#36694 = PRODUCT ( 'torque nut 03_iso_ISO 7042-M6-N', 'torque nut 03_iso_ISO 7042-M6-N', '', ( #17553 ) ) ;
#36695 = DIRECTION ( 'NONE',  ( 1.000000000000000000, 0.000000000000000000, 0.000000000000000000 ) ) ;
#36696 = DIRECTION ( 'NONE',  ( -1.000000000000000000, 0.000000000000000000, 0.000000000000000000 ) ) ;
#36697 = VERTEX_POINT ( 'NONE', #8182 ) ;
#36698 = CARTESIAN_POINT ( 'NONE',  ( -18.00000337463123756, -86.60254037844400443, -9.999999999999998224 ) ) ;
#36699 = EDGE_LOOP ( 'NONE', ( #32979, #18103, #20104, #18718, #2450, #24068 ) ) ;
#36700 = FACE_BOUND ( 'NONE', #36832, .T. ) ;
#36701 = VECTOR ( 'NONE', #19683, 1000.000000000000000 ) ;
#36702 = EDGE_CURVE ( 'NONE', #4841, #2089, #17760, .T. ) ;
#36703 = CARTESIAN_POINT ( 'NONE',  ( -57.00000337463107059, 60.62177826491078747, -9.999999999999998224 ) ) ;
#36704 = ADVANCED_FACE ( 'NONE', ( #14168 ), #4422, .F. ) ;
#36705 = ORIENTED_EDGE ( 'NONE', *, *, #19830, .F. ) ;
#36706 = DIRECTION ( 'NONE',  ( 0.000000000000000000, 0.000000000000000000, 1.000000000000000000 ) ) ;
#36707 = DIRECTION ( 'NONE',  ( 1.000000000000000000, 0.000000000000000000, 0.000000000000000000 ) ) ;
#36708 = AXIS2_PLACEMENT_3D ( 'NONE', #7678, #10125, #21558 ) ;
#36709 = DIRECTION ( 'NONE',  ( -1.000000000000000000, 0.000000000000000000, 0.000000000000000000 ) ) ;
#36710 = LINE ( 'NONE', #33350, #1137 ) ;
#36711 = ORIENTED_EDGE ( 'NONE', *, *, #30212, .F. ) ;
#36712 = CIRCLE ( 'NONE', #12733, 27.00000000000001421 ) ;
#36713 = CARTESIAN_POINT ( 'NONE',  ( 21.99999662536859191, 69.28203230275516944, 17.49999999999999645 ) ) ;
#36714 = EDGE_CURVE ( 'NONE', #29900, #9542, #35742, .T. ) ;
#36715 = FACE_OUTER_BOUND ( 'NONE', #35985, .T. ) ;
#36716 = CARTESIAN_POINT ( 'NONE',  ( -58.00000337463108480, -51.96152422706641971, -9.999999999999998224 ) ) ;
#36717 = ORIENTED_EDGE ( 'NONE', *, *, #18094, .F. ) ;
#36718 = ORIENTED_EDGE ( 'NONE', *, *, #31134, .T. ) ;
#36719 = CARTESIAN_POINT ( 'NONE',  ( 101.4249800177813086, -31.43204461043964315, 27.50000000000000000 ) ) ;
#36720 = VERTEX_POINT ( 'NONE', #18676 ) ;
#36721 = CARTESIAN_POINT ( 'NONE',  ( -33.99999999999945288, 58.88972745734214698, -49.86561046011506448 ) ) ;
#36722 = AXIS2_PLACEMENT_3D ( 'NONE', #34222, #14130, #20482 ) ;
#36723 = DIRECTION ( 'NONE',  ( 1.000000000000000000, 0.000000000000000000, 0.000000000000000000 ) ) ;
#36724 = ADVANCED_FACE ( 'NONE', ( #27098 ), #32731, .F. ) ;
#36725 = ADVANCED_FACE ( 'NONE', ( #35396 ), #33096, .F. ) ;
#36726 = CIRCLE ( 'NONE', #2004, 3.000000000000005773 ) ;
#36727 = CARTESIAN_POINT ( 'NONE',  ( 1.642566673137904498, 4.825166380998184401, -0.07080520455421732140 ) ) ;
#36728 = EDGE_CURVE ( 'NONE', #20625, #13035, #7243, .T. ) ;
#36729 = EDGE_CURVE ( 'NONE', #12147, #8890, #29722, .T. ) ;
#36730 = CARTESIAN_POINT ( 'NONE',  ( -3.500000000000000888, -55.00000000000000000, 5.000000000000000888 ) ) ;
#36731 = CARTESIAN_POINT ( 'NONE',  ( -35.00000337463116296, 60.62177826491077326, -9.999999999999998224 ) ) ;
#36732 = CARTESIAN_POINT ( 'NONE',  ( -78.83864671358962539, -72.26719042872781529, 32.49999999999999289 ) ) ;
#36733 = CARTESIAN_POINT ( 'NONE',  ( 94.40806000769313755, 12.15049814296589226, 32.50002500000000083 ) ) ;
#36734 = CARTESIAN_POINT ( 'NONE',  ( 0.000000000000000000, 0.000000000000000000, 27.50000000000000000 ) ) ;
#36735 = VERTEX_POINT ( 'NONE', #29725 ) ;
#36736 = ORIENTED_EDGE ( 'NONE', *, *, #30490, .T. ) ;
#36737 = DIRECTION ( 'NONE',  ( 0.000000000000000000, 0.000000000000000000, 1.000000000000000000 ) ) ;
#36738 = CIRCLE ( 'NONE', #28927, 2.000000000000001776 ) ;
#36739 = DIRECTION ( 'NONE',  ( 0.000000000000000000, 0.000000000000000000, 1.000000000000000000 ) ) ;
#36740 = FACE_OUTER_BOUND ( 'NONE', #8451, .T. ) ;
#36741 = DIRECTION ( 'NONE',  ( -0.000000000000000000, -0.000000000000000000, 1.000000000000000000 ) ) ;
#36742 = EDGE_LOOP ( 'NONE', ( #18160, #8806, #34778, #18558 ) ) ;
#36743 = CARTESIAN_POINT ( 'NONE',  ( -30.00000337463118427, 69.28203230275516944, -9.999999999999998224 ) ) ;
#36744 = ORIENTED_EDGE ( 'NONE', *, *, #24988, .T. ) ;
#36745 = ORIENTED_EDGE ( 'NONE', *, *, #36207, .F. ) ;
#36746 =( REPRESENTATION_RELATIONSHIP ('NONE','NONE', #15268, #26771 ) REPRESENTATION_RELATIONSHIP_WITH_TRANSFORMATION ( #16062 )SHAPE_REPRESENTATION_RELATIONSHIP( ) );
#36747 = DIRECTION ( 'NONE',  ( 0.000000000000000000, 0.000000000000000000, 1.000000000000000000 ) ) ;
#36748 = CIRCLE ( 'NONE', #20557, 3.499999999999996003 ) ;
#36749 = VERTEX_POINT ( 'NONE', #19056 ) ;
#36750 = EDGE_CURVE ( 'NONE', #34871, #30085, #13566, .T. ) ;
#36751 = CARTESIAN_POINT ( 'NONE',  ( 3.000000000000000000, 1.467624384280029615, 2.541999999999997151 ) ) ;
#36752 = CONICAL_SURFACE ( 'NONE', #32561, 5.000000000000000888, 1.047197551196596299 ) ;
#36753 = CARTESIAN_POINT ( 'NONE',  ( 0.000000000000000000, 0.000000000000000000, -5.000000000000000000 ) ) ;
#36754 = DIRECTION ( 'NONE',  ( 0.000000000000000000, 0.000000000000000000, 1.000000000000000000 ) ) ;
#36755 = VERTEX_POINT ( 'NONE', #15857 ) ;
#36756 = ORIENTED_EDGE ( 'NONE', *, *, #3906, .F. ) ;
#36757 = ORIENTED_EDGE ( 'NONE', *, *, #13155, .F. ) ;
#36758 = PRESENTATION_LAYER_ASSIGNMENT (  '', '', ( #26574 ) ) ;
#36759 = EDGE_LOOP ( 'NONE', ( #15916, #14622, #22576, #35221 ) ) ;
#36760 = ORIENTED_EDGE ( 'NONE', *, *, #19294, .F. ) ;
#36761 = DIRECTION ( 'NONE',  ( -1.000000000000000000, 3.491481338843133750E-15, 0.000000000000000000 ) ) ;
#36762 = COLOUR_RGB ( '', 0.72549020, 0.75294118, 0.79215686) ;
#36763 = DIRECTION ( 'NONE',  ( 1.000000000000000000, 0.000000000000000000, 0.000000000000000000 ) ) ;
#36764 = DIRECTION ( 'NONE',  ( 1.000000000000000000, 0.000000000000000000, 0.000000000000000000 ) ) ;
#36765 = DIRECTION ( 'NONE',  ( 1.000000000000000000, 0.000000000000000000, 0.000000000000000000 ) ) ;
#36766 = DIRECTION ( 'NONE',  ( -0.000000000000000000, -0.000000000000000000, 1.000000000000000000 ) ) ;
#36767 = ORIENTED_EDGE ( 'NONE', *, *, #28255, .F. ) ;
#36768 = CARTESIAN_POINT ( 'NONE',  ( -65.00000337463102085, 43.30127018922198801, -9.999999999999998224 ) ) ;
#36769 = CARTESIAN_POINT ( 'NONE',  ( 0.000000000000000000, 55.00000000000000000, -10.00000000000000000 ) ) ;
#36770 = EDGE_CURVE ( 'NONE', #34463, #12103, #35746, .T. ) ;
#36771 = DIRECTION ( 'NONE',  ( 0.000000000000000000, 0.000000000000000000, 1.000000000000000000 ) ) ;
#36772 = ORIENTED_EDGE ( 'NONE', *, *, #15397, .F. ) ;
#36773 = DIRECTION ( 'NONE',  ( 1.000000000000000000, 0.000000000000000000, 0.000000000000000000 ) ) ;
#36774 = CARTESIAN_POINT ( 'NONE',  ( 58.88972745734226066, 33.99999999999924682, 12.49999999999999822 ) ) ;
#36775 = ORIENTED_EDGE ( 'NONE', *, *, #14156, .F. ) ;
#36776 = CIRCLE ( 'NONE', #20581, 2.000000000000001776 ) ;
#36777 = ORIENTED_EDGE ( 'NONE', *, *, #4143, .T. ) ;
#36778 = DIRECTION ( 'NONE',  ( 1.000000000000000000, 0.000000000000000000, 0.000000000000000000 ) ) ;
#36779 = CARTESIAN_POINT ( 'NONE',  ( -1.721886139904403201, 5.052888355616344640, -4.057689166958363458 ) ) ;
#36780 = DIRECTION ( 'NONE',  ( 1.000000000000000000, 0.000000000000000000, 0.000000000000000000 ) ) ;
#36781 = CARTESIAN_POINT ( 'NONE',  ( -106.2329258812508641, -40.32806679316945520, 32.50000000000000000 ) ) ;
#36782 = VERTEX_POINT ( 'NONE', #21288 ) ;
#36783 = VERTEX_POINT ( 'NONE', #4249 ) ;
#36784 = VECTOR ( 'NONE', #16156, 1000.000000000000000 ) ;
#36785 = DIRECTION ( 'NONE',  ( 0.000000000000000000, 0.000000000000000000, -1.000000000000000000 ) ) ;
#36786 = CIRCLE ( 'NONE', #11630, 2.000000000000001776 ) ;
#36787 = ORIENTED_EDGE ( 'NONE', *, *, #36488, .F. ) ;
#36788 = CARTESIAN_POINT ( 'NONE',  ( 66.99999662536841072, 25.98076211353318854, 17.49999999999999645 ) ) ;
#36789 = ORIENTED_EDGE ( 'NONE', *, *, #2294, .T. ) ;
#36790 = EDGE_CURVE ( 'NONE', #27821, #29329, #5812, .T. ) ;
#36791 = DIRECTION ( 'NONE',  ( 1.000000000000000000, 9.251858538542971828E-16, 0.000000000000000000 ) ) ;
#36792 = LINE ( 'NONE', #22544, #28025 ) ;
#36793 = CYLINDRICAL_SURFACE ( 'NONE', #7673, 2.000000000000001776 ) ;
#36794 = ORIENTED_EDGE ( 'NONE', *, *, #6827, .T. ) ;
#36795 = AXIS2_PLACEMENT_3D ( 'NONE', #35814, #10121, #7298 ) ;
#36796 = ORIENTED_EDGE ( 'NONE', *, *, #19829, .T. ) ;
#36797 = DIRECTION ( 'NONE',  ( 0.000000000000000000, 0.000000000000000000, 1.000000000000000000 ) ) ;
#36798 = LINE ( 'NONE', #5121, #15955 ) ;
#36799 = DIRECTION ( 'NONE',  ( 1.000000000000000000, 0.000000000000000000, 0.000000000000000000 ) ) ;
#36800 = FACE_OUTER_BOUND ( 'NONE', #4161, .T. ) ;
#36801 = AXIS2_PLACEMENT_3D ( 'NONE', #32820, #36380, #21740 ) ;
#36802 = EDGE_CURVE ( 'NONE', #33338, #5117, #10054, .T. ) ;
#36803 = EDGE_LOOP ( 'NONE', ( #28334, #24234, #9377, #29537 ) ) ;
#36804 = DIRECTION ( 'NONE',  ( 0.000000000000000000, 0.000000000000000000, 1.000000000000000000 ) ) ;
#36805 = FACE_BOUND ( 'NONE', #31752, .T. ) ;
#36806 = CARTESIAN_POINT ( 'NONE',  ( 3.000000000000000000, -2.935248768560059229, 3.469446951953614189E-15 ) ) ;
#36807 = PLANE ( 'NONE',  #31265 ) ;
#36808 = CARTESIAN_POINT ( 'NONE',  ( 0.000000000000000000, 0.000000000000000000, 15.00000000000000000 ) ) ;
#36809 = DIRECTION ( 'NONE',  ( 1.000000000000000000, 0.000000000000000000, 0.000000000000000000 ) ) ;
#36810 = AXIS2_PLACEMENT_3D ( 'NONE', #17009, #22836, #31255 ) ;
#36811 = VECTOR ( 'NONE', #17250, 1000.000000000000000 ) ;
#36812 = PLANE ( 'NONE',  #29927 ) ;
#36813 = CIRCLE ( 'NONE', #28998, 30.00000000000000000 ) ;
#36814 = EDGE_CURVE ( 'NONE', #19982, #21384, #24289, .T. ) ;
#36815 = CARTESIAN_POINT ( 'NONE',  ( -5.000000000000000000, -2.886751345948133540, -6.000000000000000000 ) ) ;
#36816 = ORIENTED_EDGE ( 'NONE', *, *, #13468, .F. ) ;
#36817 = DIRECTION ( 'NONE',  ( -1.000000000000000000, 0.000000000000000000, 0.000000000000000000 ) ) ;
#36818 = DIRECTION ( 'NONE',  ( -0.7650473262243666639, 0.6439740589782693148, 0.000000000000000000 ) ) ;
#36819 = CARTESIAN_POINT ( 'NONE',  ( 86.45172111230354517, -31.46585318596159553, -49.86348611802629449 ) ) ;
#36820 = ORIENTED_EDGE ( 'NONE', *, *, #121, .T. ) ;
#36821 = ORIENTED_EDGE ( 'NONE', *, *, #7392, .F. ) ;
#36822 = ORIENTED_EDGE ( 'NONE', *, *, #18620, .F. ) ;
#36823 = CIRCLE ( 'NONE', #9269, 2.000000000000001776 ) ;
#36824 = DIRECTION ( 'NONE',  ( 0.000000000000000000, 0.000000000000000000, 1.000000000000000000 ) ) ;
#36825 = DIRECTION ( 'NONE',  ( 1.000000000000000000, 0.000000000000000000, 0.000000000000000000 ) ) ;
#36826 = EDGE_LOOP ( 'NONE', ( #14581, #5778, #7863, #12711 ) ) ;
#36827 = CIRCLE ( 'NONE', #29634, 3.500000000000000888 ) ;
#36828 = CARTESIAN_POINT ( 'NONE',  ( 74.99999662536836809, -8.660254037844401509, -5.000000000000000000 ) ) ;
#36829 = ORIENTED_EDGE ( 'NONE', *, *, #21980, .F. ) ;
#36830 = EDGE_CURVE ( 'NONE', #29836, #5293, #34530, .T. ) ;
#36831 = DIRECTION ( 'NONE',  ( 0.000000000000000000, 0.000000000000000000, 1.000000000000000000 ) ) ;
#36832 = EDGE_LOOP ( 'NONE', ( #2513, #25917 ) ) ;
#36833 = DIRECTION ( 'NONE',  ( -1.000000000000000000, 0.000000000000000000, 0.000000000000000000 ) ) ;
#36834 = AXIS2_PLACEMENT_3D ( 'NONE', #7853, #36707, #36544 ) ;
#36835 = ORIENTED_EDGE ( 'NONE', *, *, #35219, .T. ) ;
#36836 = AXIS2_PLACEMENT_3D ( 'NONE', #3263, #449, #7007 ) ;
#36837 = LINE ( 'NONE', #11144, #29166 ) ;
#36838 = CARTESIAN_POINT ( 'NONE',  ( -80.00000337463094979, 17.32050807568878525, -5.000000000000000000 ) ) ;
#36839 = EDGE_CURVE ( 'NONE', #32311, #34910, #27936, .T. ) ;
#36840 = ORIENTED_EDGE ( 'NONE', *, *, #16537, .F. ) ;
#36841 = DIRECTION ( 'NONE',  ( 0.000000000000000000, 0.000000000000000000, 1.000000000000000000 ) ) ;
#36842 = ITEM_DEFINED_TRANSFORMATION ( 'NONE', 'NONE', #382,  #21385 ) ;
#36843 = CARTESIAN_POINT ( 'NONE',  ( 74.99999662536836809, 25.98076211353319565, 17.49999999999999645 ) ) ;
#36844 = DIRECTION ( 'NONE',  ( 0.000000000000000000, 0.000000000000000000, 1.000000000000000000 ) ) ;
#36845 = EDGE_CURVE ( 'NONE', #34930, #16912, #32728, .T. ) ;
#36846 = VECTOR ( 'NONE', #32898, 1000.000000000000000 ) ;
#36847 = ORIENTED_EDGE ( 'NONE', *, *, #29216, .T. ) ;
#36848 = CYLINDRICAL_SURFACE ( 'NONE', #21569, 1.999999999999998224 ) ;
#36849 = CARTESIAN_POINT ( 'NONE',  ( -12.00000337463125000, -86.60254037844400443, 17.49999999999999645 ) ) ;
#36850 = ORIENTED_EDGE ( 'NONE', *, *, #24767, .T. ) ;
#36851 = FACE_OUTER_BOUND ( 'NONE', #29581, .T. ) ;
#36852 = AXIS2_PLACEMENT_3D ( 'NONE', #19929, #31005, #36809 ) ;
#36853 = DIRECTION ( 'NONE',  ( 0.000000000000000000, 0.000000000000000000, -1.000000000000000000 ) ) ;
#36854 = CARTESIAN_POINT ( 'NONE',  ( 51.99999662536847467, 69.28203230275516944, 17.49999999999999645 ) ) ;
#36855 = AXIS2_PLACEMENT_3D ( 'NONE', #31705, #585, #17090 ) ;
#36856 = CIRCLE ( 'NONE', #21298, 3.000000000000002665 ) ;
#36857 = CARTESIAN_POINT ( 'NONE',  ( 56.67878100130369035, -27.78182860042797131, 12.49999999999999822 ) ) ;
#36858 = AXIS2_PLACEMENT_3D ( 'NONE', #10831, #5562, #22261 ) ;
#36859 = EDGE_LOOP ( 'NONE', ( #32207, #33428, #37101, #36013 ) ) ;
#36860 = EDGE_LOOP ( 'NONE', ( #19515, #26999 ) ) ;
#36861 = CARTESIAN_POINT ( 'NONE',  ( -78.00000337463096400, -34.64101615137762025, -9.999999999999998224 ) ) ;
#36862 = CYLINDRICAL_SURFACE ( 'NONE', #5019, 2.000000000000000000 ) ;
#36863 = B_SPLINE_CURVE_WITH_KNOTS ( 'NONE', 3,
 ( #2481, #1918, #25348, #30774, #36781, #21617, #33047, #13175, #1739, #5100, #27972, #33223 ),
 .UNSPECIFIED., .F., .F.,
 ( 4, 1, 2, 2, 1, 2, 4 ),
 ( 0.3332735168080938615, 0.3610471732601487904, 0.3749340014861762826, 0.3888208297122037749, 0.4165944861642589259, 0.4304813143902864181, 0.4443681426163139103 ),
 .UNSPECIFIED. ) ;
#36864 = CIRCLE ( 'NONE', #20680, 0.2999999999999999334 ) ;
#36865 = AXIS2_PLACEMENT_3D ( 'NONE', #17292, #26078, #31329 ) ;
#36866 = EDGE_CURVE ( 'NONE', #27114, #2420, #15678, .T. ) ;
#36867 = ORIENTED_EDGE ( 'NONE', *, *, #32768, .F. ) ;
#36868 = VERTEX_POINT ( 'NONE', #1799 ) ;
#36869 = CARTESIAN_POINT ( 'NONE',  ( -48.00000337463112032, -51.96152422706641971, -5.000000000000000000 ) ) ;
#36870 = DIRECTION ( 'NONE',  ( -0.1391731009600657432, 0.000000000000000000, -0.9902680687415703620 ) ) ;
#36871 = DIRECTION ( 'NONE',  ( -1.000000000000000000, 0.000000000000000000, 0.000000000000000000 ) ) ;
#36872 = ORIENTED_EDGE ( 'NONE', *, *, #18175, .T. ) ;
#36873 = EDGE_CURVE ( 'NONE', #8103, #6603, #1042, .T. ) ;
#36874 = ORIENTED_EDGE ( 'NONE', *, *, #7466, .F. ) ;
#36875 = CARTESIAN_POINT ( 'NONE',  ( 74.99999662536835388, -43.30127018922199511, -9.999999999999998224 ) ) ;
#36876 = AXIS2_PLACEMENT_3D ( 'NONE', #8330, #16933, #28358 ) ;
#36877 = CYLINDRICAL_SURFACE ( 'NONE', #30261, 2.000000000000001776 ) ;
#36878 = VERTEX_POINT ( 'NONE', #24676 ) ;
#36879 = ADVANCED_FACE ( 'NONE', ( #32929 ), #2846, .T. ) ;
#36880 = CARTESIAN_POINT ( 'NONE',  ( -3.374631334790434423E-06, 69.28203230275516944, -9.999999999999998224 ) ) ;
#36881 = ORIENTED_EDGE ( 'NONE', *, *, #20477, .F. ) ;
#36882 = FACE_BOUND ( 'NONE', #21540, .T. ) ;
#36883 = AXIS2_PLACEMENT_3D ( 'NONE', #35642, #18395, #12569 ) ;
#36884 = CIRCLE ( 'NONE', #30294, 20.00000000000001066 ) ;
#36885 = AXIS2_PLACEMENT_3D ( 'NONE', #32515, #13213, #7032 ) ;
#36886 = CARTESIAN_POINT ( 'NONE',  ( 0.000000000000000000, 0.000000000000000000, 27.50000000000000000 ) ) ;
#36887 = CIRCLE ( 'NONE', #22512, 2.000000000000001776 ) ;
#36888 = ORIENTED_EDGE ( 'NONE', *, *, #29935, .T. ) ;
#36889 = DIRECTION ( 'NONE',  ( -0.3123845849830156340, -0.9499557205812222405, 0.000000000000000000 ) ) ;
#36890 = AXIS2_PLACEMENT_3D ( 'NONE', #2359, #11141, #4971 ) ;
#36891 = FACE_OUTER_BOUND ( 'NONE', #26817, .T. ) ;
#36892 = EDGE_CURVE ( 'NONE', #21874, #725, #32155, .T. ) ;
#36893 = DIRECTION ( 'NONE',  ( 0.000000000000000000, 0.000000000000000000, 1.000000000000000000 ) ) ;
#36894 = FACE_OUTER_BOUND ( 'NONE', #22924, .T. ) ;
#36895 = ORIENTED_EDGE ( 'NONE', *, *, #32837, .T. ) ;
#36896 = DIRECTION ( 'NONE',  ( 1.000000000000000000, 0.000000000000000000, 0.000000000000000000 ) ) ;
#36897 = CARTESIAN_POINT ( 'NONE',  ( -68.00000337463099243, 51.96152422706637708, -9.999999999999998224 ) ) ;
#36898 = LINE ( 'NONE', #16294, #33300 ) ;
#36899 = AXIS2_PLACEMENT_3D ( 'NONE', #8713, #8539, #20157 ) ;
#36900 = ORIENTED_EDGE ( 'NONE', *, *, #3188, .F. ) ;
#36901 = ORIENTED_EDGE ( 'NONE', *, *, #15591, .F. ) ;
#36902 = ORIENTED_EDGE ( 'NONE', *, *, #7055, .F. ) ;
#36903 = FACE_OUTER_BOUND ( 'NONE', #22504, .T. ) ;
#36904 = FACE_OUTER_BOUND ( 'NONE', #30775, .T. ) ;
#36905 = VECTOR ( 'NONE', #19206, 1000.000000000000000 ) ;
#36906 = CIRCLE ( 'NONE', #4586, 5.000000000000000000 ) ;
#36907 = AXIS2_PLACEMENT_3D ( 'NONE', #1529, #21042, #15788 ) ;
#36908 = CARTESIAN_POINT ( 'NONE',  ( 61.99999662536845335, 34.64101615137759893, -9.999999999999998224 ) ) ;
#36909 = CIRCLE ( 'NONE', #25509, 2.000000000000001776 ) ;
#36910 = EDGE_CURVE ( 'NONE', #3771, #12599, #22794, .T. ) ;
#36911 = CARTESIAN_POINT ( 'NONE',  ( -4.185558440016324155, -3.356969399843958257, -0.2680587191991318785 ) ) ;
#36912 = DIRECTION ( 'NONE',  ( -0.000000000000000000, -0.000000000000000000, -1.000000000000000000 ) ) ;
#36913 = CARTESIAN_POINT ( 'NONE',  ( -105.5599775193885392, -56.84101280297493020, 32.50000000000000711 ) ) ;
#36914 = ADVANCED_FACE ( 'NONE', ( #8156 ), #7970, .F. ) ;
#36915 = DIRECTION ( 'NONE',  ( 0.000000000000000000, 0.000000000000000000, 1.000000000000000000 ) ) ;
#36916 = DIRECTION ( 'NONE',  ( -1.051347561198064495E-14, -1.000000000000000000, 0.000000000000000000 ) ) ;
#36917 = ORIENTED_EDGE ( 'NONE', *, *, #25976, .F. ) ;
#36918 = CIRCLE ( 'NONE', #20736, 2.000000000000001776 ) ;
#36919 = ADVANCED_FACE ( 'NONE', ( #31381 ), #5712, .T. ) ;
#36920 = ORIENTED_EDGE ( 'NONE', *, *, #17239, .F. ) ;
#36921 = FACE_OUTER_BOUND ( 'NONE', #11808, .T. ) ;
#36922 = DIRECTION ( 'NONE',  ( 0.000000000000000000, 0.000000000000000000, -1.000000000000000000 ) ) ;
#36923 = CARTESIAN_POINT ( 'NONE',  ( -101.4249800177817207, -31.43204461043823272, 27.50000000000000000 ) ) ;
#36924 = CYLINDRICAL_SURFACE ( 'NONE', #34676, 2.000000000000001776 ) ;
#36925 = EDGE_CURVE ( 'NONE', #23651, #18582, #8798, .T. ) ;
#36926 = ORIENTED_EDGE ( 'NONE', *, *, #11710, .T. ) ;
#36927 = UNCERTAINTY_MEASURE_WITH_UNIT (LENGTH_MEASURE( 1.000000000000000082E-05 ), #25929, 'distance_accuracy_value', 'NONE');
#36928 = EDGE_CURVE ( 'NONE', #26778, #11374, #25597, .T. ) ;
#36929 = AXIS2_PLACEMENT_3D ( 'NONE', #31186, #2502, #13924 ) ;
#36930 = VECTOR ( 'NONE', #23366, 1000.000000000000000 ) ;
#36931 = FACE_BOUND ( 'NONE', #20952, .T. ) ;
#36932 = VERTEX_POINT ( 'NONE', #30653 ) ;
#36933 = ORIENTED_EDGE ( 'NONE', *, *, #36084, .T. ) ;
#36934 = AXIS2_PLACEMENT_3D ( 'NONE', #23392, #32172, #23200 ) ;
#36935 = FACE_OUTER_BOUND ( 'NONE', #4714, .T. ) ;
#36936 = EDGE_LOOP ( 'NONE', ( #18080, #31585, #29045, #29016 ) ) ;
#36937 = CIRCLE ( 'NONE', #20753, 27.00000000000001421 ) ;
#36938 = EDGE_CURVE ( 'NONE', #32397, #34636, #8224, .T. ) ;
#36940 = AXIS2_PLACEMENT_3D ( 'NONE', #33687, #13815, #11169 ) ;
#36939 = SURFACE_SIDE_STYLE ('',( #31294 ) ) ;
#36941 = DIRECTION ( 'NONE',  ( 0.000000000000000000, 0.000000000000000000, -1.000000000000000000 ) ) ;
#36942 = CIRCLE ( 'NONE', #21951, 2.500000000000000000 ) ;
#36943 = ADVANCED_FACE ( 'NONE', ( #10958 ), #2154, .F. ) ;
#36944 = DIRECTION ( 'NONE',  ( 0.000000000000000000, 0.000000000000000000, 1.000000000000000000 ) ) ;
#36945 = VECTOR ( 'NONE', #4072, 1000.000000000000000 ) ;
#36946 = EDGE_CURVE ( 'NONE', #357, #245, #31032, .T. ) ;
#36947 = CARTESIAN_POINT ( 'NONE',  ( 0.3000000000000016542, 0.000000000000000000, 4.700000000000000178 ) ) ;
#36948 = ADVANCED_FACE ( 'NONE', ( #19959 ), #33491, .F. ) ;
#36949 = VERTEX_POINT ( 'NONE', #28033 ) ;
#36950 = ORIENTED_EDGE ( 'NONE', *, *, #25205, .T. ) ;
#36951 = VERTEX_POINT ( 'NONE', #25404 ) ;
#36952 = CIRCLE ( 'NONE', #24996, 27.00000000000001421 ) ;
#36953 = VERTEX_POINT ( 'NONE', #22398 ) ;
#36954 = VERTEX_POINT ( 'NONE', #2360 ) ;
#36955 = DIRECTION ( 'NONE',  ( 0.000000000000000000, 0.000000000000000000, 1.000000000000000000 ) ) ;
#36956 = CARTESIAN_POINT ( 'NONE',  ( 19.99999662536861678, -69.28203230275519786, 12.50000000000000000 ) ) ;
#36958 = AXIS2_PLACEMENT_3D ( 'NONE', #14360, #28600, #20507 ) ;
#36957 = DIRECTION ( 'NONE',  ( -1.000000000000000000, 0.000000000000000000, 0.000000000000000000 ) ) ;
#36959 = CYLINDRICAL_SURFACE ( 'NONE', #16928, 2.000000000000001776 ) ;
#36960 = DIRECTION ( 'NONE',  ( -1.000000000000000000, 0.000000000000000000, 0.000000000000000000 ) ) ;
#36961 = CIRCLE ( 'NONE', #6403, 2.000000000000001776 ) ;
#36962 = ORIENTED_EDGE ( 'NONE', *, *, #23295, .F. ) ;
#36963 = LINE ( 'NONE', #2837, #35084 ) ;
#36964 = AXIS2_PLACEMENT_3D ( 'NONE', #22325, #22509, #33596 ) ;
#36965 = LINE ( 'NONE', #4737, #31758 ) ;
#36966 = CIRCLE ( 'NONE', #35763, 27.00000000000001421 ) ;
#36967 = DIRECTION ( 'NONE',  ( 0.000000000000000000, 0.000000000000000000, 1.000000000000000000 ) ) ;
#36968 = ORIENTED_EDGE ( 'NONE', *, *, #2414, .F. ) ;
#36969 = DIRECTION ( 'NONE',  ( -1.000000000000000000, 0.000000000000000000, 0.000000000000000000 ) ) ;
#36970 = FACE_OUTER_BOUND ( 'NONE', #4803, .T. ) ;
#36971 = AXIS2_PLACEMENT_3D ( 'NONE', #15496, #12659, #21493 ) ;
#36972 = VERTEX_POINT ( 'NONE', #5364 ) ;
#36973 = AXIS2_PLACEMENT_3D ( 'NONE', #24936, #22298, #21927 ) ;
#36974 = EDGE_LOOP ( 'NONE', ( #22525, #29453, #22000, #31320, #27110, #17486 ) ) ;
#36975 = AXIS2_PLACEMENT_3D ( 'NONE', #2122, #21643, #25210 ) ;
#36976 = DIRECTION ( 'NONE',  ( -0.5000000000000098810, -0.8660254037844328234, 0.000000000000000000 ) ) ;
#36977 = CARTESIAN_POINT ( 'NONE',  ( -60.93295298010992411, -19.13981058454771755, 12.49999999999999822 ) ) ;
#36978 = FACE_OUTER_BOUND ( 'NONE', #18600, .T. ) ;
#36979 = CYLINDRICAL_SURFACE ( 'NONE', #11296, 100.0000000000000142 ) ;
#36980 = ORIENTED_EDGE ( 'NONE', *, *, #2801, .F. ) ;
#36981 = ORIENTED_EDGE ( 'NONE', *, *, #36845, .F. ) ;
#36982 = CARTESIAN_POINT ( 'NONE',  ( -72.28378166042018904, -61.53067111003240797, -49.22241343995298024 ) ) ;
#36983 = CIRCLE ( 'NONE', #31583, 3.000000000000002665 ) ;
#36984 = ORIENTED_EDGE ( 'NONE', *, *, #7262, .F. ) ;
#36985 = CIRCLE ( 'NONE', #19036, 3.000000000000000888 ) ;
#36986 = CYLINDRICAL_SURFACE ( 'NONE', #33366, 2.000000000000001776 ) ;
#36987 = EDGE_LOOP ( 'NONE', ( #19283, #25253 ) ) ;
#36988 = CIRCLE ( 'NONE', #29831, 2.000000000000001776 ) ;
#36989 = ORIENTED_EDGE ( 'NONE', *, *, #32810, .T. ) ;
#36990 = CARTESIAN_POINT ( 'NONE',  ( -25.00000337463121980, -77.94228634059963667, 17.49999999999999645 ) ) ;
#36991 = DIRECTION ( 'NONE',  ( 0.000000000000000000, 0.000000000000000000, 1.000000000000000000 ) ) ;
#36992 = FACE_BOUND ( 'NONE', #33452, .T. ) ;
#36993 = EDGE_CURVE ( 'NONE', #32864, #24448, #32724, .T. ) ;
#36994 = ORIENTED_EDGE ( 'NONE', *, *, #32773, .T. ) ;
#36995 = ORIENTED_EDGE ( 'NONE', *, *, #4034, .T. ) ;
#36996 = CYLINDRICAL_SURFACE ( 'NONE', #23935, 27.00000000000001066 ) ;
#36997 = DIRECTION ( 'NONE',  ( -1.000000000000000000, 0.000000000000000000, 0.000000000000000000 ) ) ;
#36998 = CIRCLE ( 'NONE', #5257, 33.00000000000001421 ) ;
#36999 = CARTESIAN_POINT ( 'NONE',  ( 72.99999662536835388, -25.98076211353319565, -5.000000000000000000 ) ) ;
#37000 = CARTESIAN_POINT ( 'NONE',  ( 12.99999662536863632, -77.94228634059960825, -9.999999999999998224 ) ) ;
#37001 = CIRCLE ( 'NONE', #22622, 2.000000000000001776 ) ;
#37002 = ORIENTED_EDGE ( 'NONE', *, *, #20004, .F. ) ;
#37003 = CYLINDRICAL_SURFACE ( 'NONE', #16563, 2.000000000000001776 ) ;
#37004 = FACE_BOUND ( 'NONE', #32960, .T. ) ;
#37005 = CARTESIAN_POINT ( 'NONE',  ( -18.00000337463123756, -69.28203230275522628, 12.50000000000000000 ) ) ;
#37006 = CARTESIAN_POINT ( 'NONE',  ( 74.99999662536836809, 43.30127018922198801, 12.50000000000000000 ) ) ;
#37007 = AXIS2_PLACEMENT_3D ( 'NONE', #17905, #17703, #97 ) ;
#37008 = FACE_OUTER_BOUND ( 'NONE', #29178, .T. ) ;
#37009 = CARTESIAN_POINT ( 'NONE',  ( 5.244818697407745312, -2.029379090245567951, -4.190884354498995101 ) ) ;
#37010 = PRODUCT ( 'socket head cap screw_iso_ISO 4762 M6 x 30 - 30N', 'socket head cap screw_iso_ISO 4762 M6 x 30 - 30N', '', ( #3516 ) ) ;
#37011 = CARTESIAN_POINT ( 'NONE',  ( 5.089798887113564874, 119.6083602675371651, 27.49998799999999477 ) ) ;
#37012 = AXIS2_PLACEMENT_3D ( 'NONE', #28534, #16918, #2662 ) ;
#37013 = CARTESIAN_POINT ( 'NONE',  ( -85.00000337463092137, -8.660254037844422825, -5.000000000000000000 ) ) ;
#37014 = VERTEX_POINT ( 'NONE', #19240 ) ;
#37015 = DIRECTION ( 'NONE',  ( 1.000000000000000000, 0.000000000000000000, 0.000000000000000000 ) ) ;
#37016 = CIRCLE ( 'NONE', #4061, 1.999999999999998224 ) ;
#37017 = CIRCLE ( 'NONE', #12447, 2.000000000000001776 ) ;
#37018 = CARTESIAN_POINT ( 'NONE',  ( -5.000000000000000000, -0.9835753746177081647, -0.05800540215399103972 ) ) ;
#37019 = CARTESIAN_POINT ( 'NONE',  ( -37.50000000000000000, 103.4105893997321743, 32.50000000000000000 ) ) ;
#37020 = EDGE_CURVE ( 'NONE', #111, #28932, #36837, .T. ) ;
#37021 = ADVANCED_FACE ( 'NONE', ( #22593 ), #8357, .F. ) ;
#37022 = AXIS2_PLACEMENT_3D ( 'NONE', #8222, #33554, #7860 ) ;
#37023 = ORIENTED_EDGE ( 'NONE', *, *, #16020, .F. ) ;
#37024 = ORIENTED_EDGE ( 'NONE', *, *, #17191, .F. ) ;
#37025 = ORIENTED_EDGE ( 'NONE', *, *, #32366, .T. ) ;
#37026 = DIRECTION ( 'NONE',  ( 1.000000000000000000, 0.000000000000000000, 0.000000000000000000 ) ) ;
#37027 = CARTESIAN_POINT ( 'NONE',  ( 0.000000000000000000, 89.94802294027088863, 32.49999999999999289 ) ) ;
#37028 = DIRECTION ( 'NONE',  ( -0.8660254037844449249, -0.4999999999999888423, 0.000000000000000000 ) ) ;
#37029 = VERTEX_POINT ( 'NONE', #28386 ) ;
#37030 = LINE ( 'NONE', #11333, #14905 ) ;
#37031 = EDGE_CURVE ( 'NONE', #28688, #24619, #23796, .T. ) ;
#37032 = ORIENTED_EDGE ( 'NONE', *, *, #16503, .F. ) ;
#37033 = CARTESIAN_POINT ( 'NONE',  ( -43.00331345287344931, -60.50675932581249583, 12.50000000000000000 ) ) ;
#37034 = ORIENTED_EDGE ( 'NONE', *, *, #23789, .T. ) ;
#37035 = DIRECTION ( 'NONE',  ( -0.000000000000000000, -0.000000000000000000, 1.000000000000000000 ) ) ;
#37036 = CIRCLE ( 'NONE', #32827, 2.000000000000001776 ) ;
#37037 = ORIENTED_EDGE ( 'NONE', *, *, #23918, .T. ) ;
#37038 = VERTEX_POINT ( 'NONE', #31755 ) ;
#37039 = CARTESIAN_POINT ( 'NONE',  ( -0.8192951148925873284, 5.300482436767278926, -5.801655677627841179 ) ) ;
#37040 = DIRECTION ( 'NONE',  ( -1.000000000000000000, 0.000000000000000000, 0.000000000000000000 ) ) ;
#37041 = CIRCLE ( 'NONE', #32857, 3.000000000000003997 ) ;
#37042 = EDGE_CURVE ( 'NONE', #27070, #36437, #17346, .T. ) ;
#37043 = ORIENTED_EDGE ( 'NONE', *, *, #36270, .T. ) ;
#37044 = CARTESIAN_POINT ( 'NONE',  ( 67.99999662536838230, 17.32050807568879236, -9.999999999999998224 ) ) ;
#37045 = AXIS2_PLACEMENT_3D ( 'NONE', #34158, #8454, #10 ) ;
#37046 = AXIS2_PLACEMENT_3D ( 'NONE', #19423, #30842, #13410 ) ;
#37047 = CARTESIAN_POINT ( 'NONE',  ( 145.0000000000000568, -5.056524707326808249E-13, 32.50000000000000000 ) ) ;
#37048 = DIRECTION ( 'NONE',  ( 0.000000000000000000, 0.000000000000000000, 1.000000000000000000 ) ) ;
#37049 = ORIENTED_EDGE ( 'NONE', *, *, #8831, .T. ) ;
#37050 = CARTESIAN_POINT ( 'NONE',  ( 3.000000000000000000, 0.000000000000000000, 0.000000000000000000 ) ) ;
#37051 = CARTESIAN_POINT ( 'NONE',  ( 42.99999662536850309, -60.62177826491080168, 17.49999999999999645 ) ) ;
#37052 = ORIENTED_EDGE ( 'NONE', *, *, #15282, .F. ) ;
#37053 = CARTESIAN_POINT ( 'NONE',  ( 29.99999662536857770, -69.28203230275519786, -5.000000000000000000 ) ) ;
#37054 = CYLINDRICAL_SURFACE ( 'NONE', #23877, 2.000000000000001776 ) ;
#37055 = DIRECTION ( 'NONE',  ( 1.000000000000000000, 0.000000000000000000, 0.000000000000000000 ) ) ;
#37056 = AXIS2_PLACEMENT_3D ( 'NONE', #31699, #34723, #26271 ) ;
#37057 = CARTESIAN_POINT ( 'NONE',  ( 139.0000000000000284, -5.056524707326808249E-13, 27.50000000000000000 ) ) ;
#37058 = AXIS2_PLACEMENT_3D ( 'NONE', #17476, #28350, #14482 ) ;
#37059 = ORIENTED_EDGE ( 'NONE', *, *, #24071, .T. ) ;
#37060 = EDGE_CURVE ( 'NONE', #19941, #2260, #7634, .T. ) ;
#37061 = EDGE_LOOP ( 'NONE', ( #12978, #21223, #8901, #2590 ) ) ;
#37062 = LINE ( 'NONE', #34072, #23149 ) ;
#37063 = FACE_OUTER_BOUND ( 'NONE', #23223, .T. ) ;
#37064 = EDGE_CURVE ( 'NONE', #18201, #4131, #33383, .T. ) ;
#37065 = ORIENTED_EDGE ( 'NONE', *, *, #8068, .F. ) ;
#37066 = VERTEX_POINT ( 'NONE', #6454 ) ;
#37067 = AXIS2_PLACEMENT_3D ( 'NONE', #21346, #32793, #7110 ) ;
#37068 = CARTESIAN_POINT ( 'NONE',  ( 79.99999662536833966, 34.64101615137759183, 17.49999999999999645 ) ) ;
#37069 = DIRECTION ( 'NONE',  ( -1.000000000000000000, 0.000000000000000000, 0.000000000000000000 ) ) ;
#37070 = ADVANCED_FACE ( 'NONE', ( #17508 ), #25955, .F. ) ;
#37071 = DIRECTION ( 'NONE',  ( -1.000000000000000000, 0.000000000000000000, 0.000000000000000000 ) ) ;
#37072 = ORIENTED_EDGE ( 'NONE', *, *, #2128, .F. ) ;
#37073 = ORIENTED_EDGE ( 'NONE', *, *, #32717, .F. ) ;
#37074 =( LENGTH_UNIT ( ) NAMED_UNIT ( * ) SI_UNIT ( .MILLI., .METRE. ) );
#37075 = EDGE_CURVE ( 'NONE', #35191, #8606, #26175, .T. ) ;
#37076 = CARTESIAN_POINT ( 'NONE',  ( 47.63139720814400846, -27.50000000000022737, 5.000000000000000888 ) ) ;
#37077 = ORIENTED_EDGE ( 'NONE', *, *, #36993, .F. ) ;
#37078 = CONICAL_SURFACE ( 'NONE', #28073, 3.000000000000000888, 0.9599310885968804774 ) ;
#37079 = CARTESIAN_POINT ( 'NONE',  ( -3.000003374631269981, -77.94228634059960825, -9.999999999999998224 ) ) ;
#37080 = ORIENTED_EDGE ( 'NONE', *, *, #5717, .F. ) ;
#37081 = DIRECTION ( 'NONE',  ( 0.000000000000000000, 0.000000000000000000, 1.000000000000000000 ) ) ;
#37082 = AXIS2_PLACEMENT_3D ( 'NONE', #6153, #18336, #1273 ) ;
#37083 = CIRCLE ( 'NONE', #24507, 2.000000000000000000 ) ;
#37084 = CARTESIAN_POINT ( 'NONE',  ( 4.279621169095998212, -62.97617850287780072, -4.999999999999997335 ) ) ;
#37085 = CARTESIAN_POINT ( 'NONE',  ( -55.00000337463109901, -60.62177826491083010, -9.999999999999998224 ) ) ;
#37086 = VECTOR ( 'NONE', #30251, 1000.000000000000000 ) ;
#37087 = ORIENTED_EDGE ( 'NONE', *, *, #13044, .F. ) ;
#37088 = CARTESIAN_POINT ( 'NONE',  ( 37.49999999999999289, 103.4105893997322596, -26.00000000000000000 ) ) ;
#37089 = DIRECTION ( 'NONE',  ( -0.000000000000000000, -0.000000000000000000, 1.000000000000000000 ) ) ;
#37090 = ADVANCED_FACE ( 'NONE', ( #252 ), #3461, .F. ) ;
#37091 = AXIS2_PLACEMENT_3D ( 'NONE', #22065, #10420, #7429 ) ;
#37092 = CARTESIAN_POINT ( 'NONE',  ( -3.374631289687624047E-06, -69.28203230275519786, 12.50000000000000000 ) ) ;
#37093 = DIRECTION ( 'NONE',  ( 0.000000000000000000, 0.000000000000000000, 1.000000000000000000 ) ) ;
#37094 = EDGE_LOOP ( 'NONE', ( #19391, #6984 ) ) ;
#37095 = CARTESIAN_POINT ( 'NONE',  ( 42.99999662536848888, 60.62177826491077326, 12.50000000000000000 ) ) ;
#37096 = AXIS2_PLACEMENT_3D ( 'NONE', #11100, #1932, #24817 ) ;
#37097 = LINE ( 'NONE', #31972, #468 ) ;
#37098 = CYLINDRICAL_SURFACE ( 'NONE', #2168, 2.000000000000001776 ) ;
#37099 = ADVANCED_FACE ( 'NONE', ( #640 ), #14892, .F. ) ;
#37100 = EDGE_LOOP ( 'NONE', ( #18708, #4286 ) ) ;
#37101 = ORIENTED_EDGE ( 'NONE', *, *, #9673, .T. ) ;
#37102 = CIRCLE ( 'NONE', #29888, 2.000000000000000000 ) ;
#37103 = EDGE_CURVE ( 'NONE', #19005, #21830, #15416, .T. ) ;
#37104 = ORIENTED_EDGE ( 'NONE', *, *, #9061, .T. ) ;
#37105 = AXIS2_PLACEMENT_3D ( 'NONE', #8935, #495, #31787 ) ;
#37106 = FACE_OUTER_BOUND ( 'NONE', #5351, .T. ) ;
#37107 = ORIENTED_EDGE ( 'NONE', *, *, #33172, .F. ) ;
#37108 = NEXT_ASSEMBLY_USAGE_OCCURRENCE ( 'NAUO1', ' ', ' ', #22359, #2674, $ ) ;
#37109 = NEXT_ASSEMBLY_USAGE_OCCURRENCE ( 'NAUO2', ' ', ' ', #22359, #377, $ ) ;
#37110 = NEXT_ASSEMBLY_USAGE_OCCURRENCE ( 'NAUO3', ' ', ' ', #22359, #6997, $ ) ;
#37111 = NEXT_ASSEMBLY_USAGE_OCCURRENCE ( 'NAUO4', ' ', ' ', #22359, #15978, $ ) ;
#37112 = NEXT_ASSEMBLY_USAGE_OCCURRENCE ( 'NAUO5', ' ', ' ', #22359, #1995, $ ) ;
#37113 = NEXT_ASSEMBLY_USAGE_OCCURRENCE ( 'NAUO6', ' ', ' ', #22359, #10927, $ ) ;
#37114 = NEXT_ASSEMBLY_USAGE_OCCURRENCE ( 'NAUO7', ' ', ' ', #22359, #14827, $ ) ;
#37115 = NEXT_ASSEMBLY_USAGE_OCCURRENCE ( 'NAUO8', ' ', ' ', #22359, #10927, $ ) ;
#37116 = NEXT_ASSEMBLY_USAGE_OCCURRENCE ( 'NAUO9', ' ', ' ', #22359, #9065, $ ) ;
#37117 = NEXT_ASSEMBLY_USAGE_OCCURRENCE ( 'NAUO10', ' ', ' ', #22359, #9065, $ ) ;
#37118 = NEXT_ASSEMBLY_USAGE_OCCURRENCE ( 'NAUO11', ' ', ' ', #22359, #9065, $ ) ;
#37119 = NEXT_ASSEMBLY_USAGE_OCCURRENCE ( 'NAUO12', ' ', ' ', #22359, #9065, $ ) ;
#37120 = NEXT_ASSEMBLY_USAGE_OCCURRENCE ( 'NAUO13', ' ', ' ', #22359, #9065, $ ) ;
#37121 = NEXT_ASSEMBLY_USAGE_OCCURRENCE ( 'NAUO14', ' ', ' ', #22359, #9065, $ ) ;
#37122 = NEXT_ASSEMBLY_USAGE_OCCURRENCE ( 'NAUO15', ' ', ' ', #22359, #10927, $ ) ;
#37123 = NEXT_ASSEMBLY_USAGE_OCCURRENCE ( 'NAUO16', ' ', ' ', #22359, #10927, $ ) ;
#37124 = NEXT_ASSEMBLY_USAGE_OCCURRENCE ( 'NAUO17', ' ', ' ', #22359, #10927, $ ) ;
#37125 = NEXT_ASSEMBLY_USAGE_OCCURRENCE ( 'NAUO18', ' ', ' ', #22359, #10927, $ ) ;
#37126 = NEXT_ASSEMBLY_USAGE_OCCURRENCE ( 'NAUO19', ' ', ' ', #22359, #15978, $ ) ;
#37127 = NEXT_ASSEMBLY_USAGE_OCCURRENCE ( 'NAUO20', ' ', ' ', #22359, #15978, $ ) ;
#37128 = NEXT_ASSEMBLY_USAGE_OCCURRENCE ( 'NAUO21', ' ', ' ', #22359, #14827, $ ) ;
#37129 = NEXT_ASSEMBLY_USAGE_OCCURRENCE ( 'NAUO22', ' ', ' ', #22359, #14827, $ ) ;
#37130 = NEXT_ASSEMBLY_USAGE_OCCURRENCE ( 'NAUO23', ' ', ' ', #22359, #14827, $ ) ;
#37131 = NEXT_ASSEMBLY_USAGE_OCCURRENCE ( 'NAUO24', ' ', ' ', #22359, #14827, $ ) ;
#37132 = NEXT_ASSEMBLY_USAGE_OCCURRENCE ( 'NAUO25', ' ', ' ', #22359, #14827, $ ) ;
#37133 = NEXT_ASSEMBLY_USAGE_OCCURRENCE ( 'NAUO26', ' ', ' ', #22359, #1995, $ ) ;
#37134 = NEXT_ASSEMBLY_USAGE_OCCURRENCE ( 'NAUO27', ' ', ' ', #22359, #1995, $ ) ;
#37135 = NEXT_ASSEMBLY_USAGE_OCCURRENCE ( 'NAUO28', ' ', ' ', #22359, #1995, $ ) ;
#37136 = NEXT_ASSEMBLY_USAGE_OCCURRENCE ( 'NAUO29', ' ', ' ', #22359, #1995, $ ) ;
#37137 = NEXT_ASSEMBLY_USAGE_OCCURRENCE ( 'NAUO30', ' ', ' ', #22359, #1995, $ ) ;
ENDSEC;
END-ISO-10303-21;
